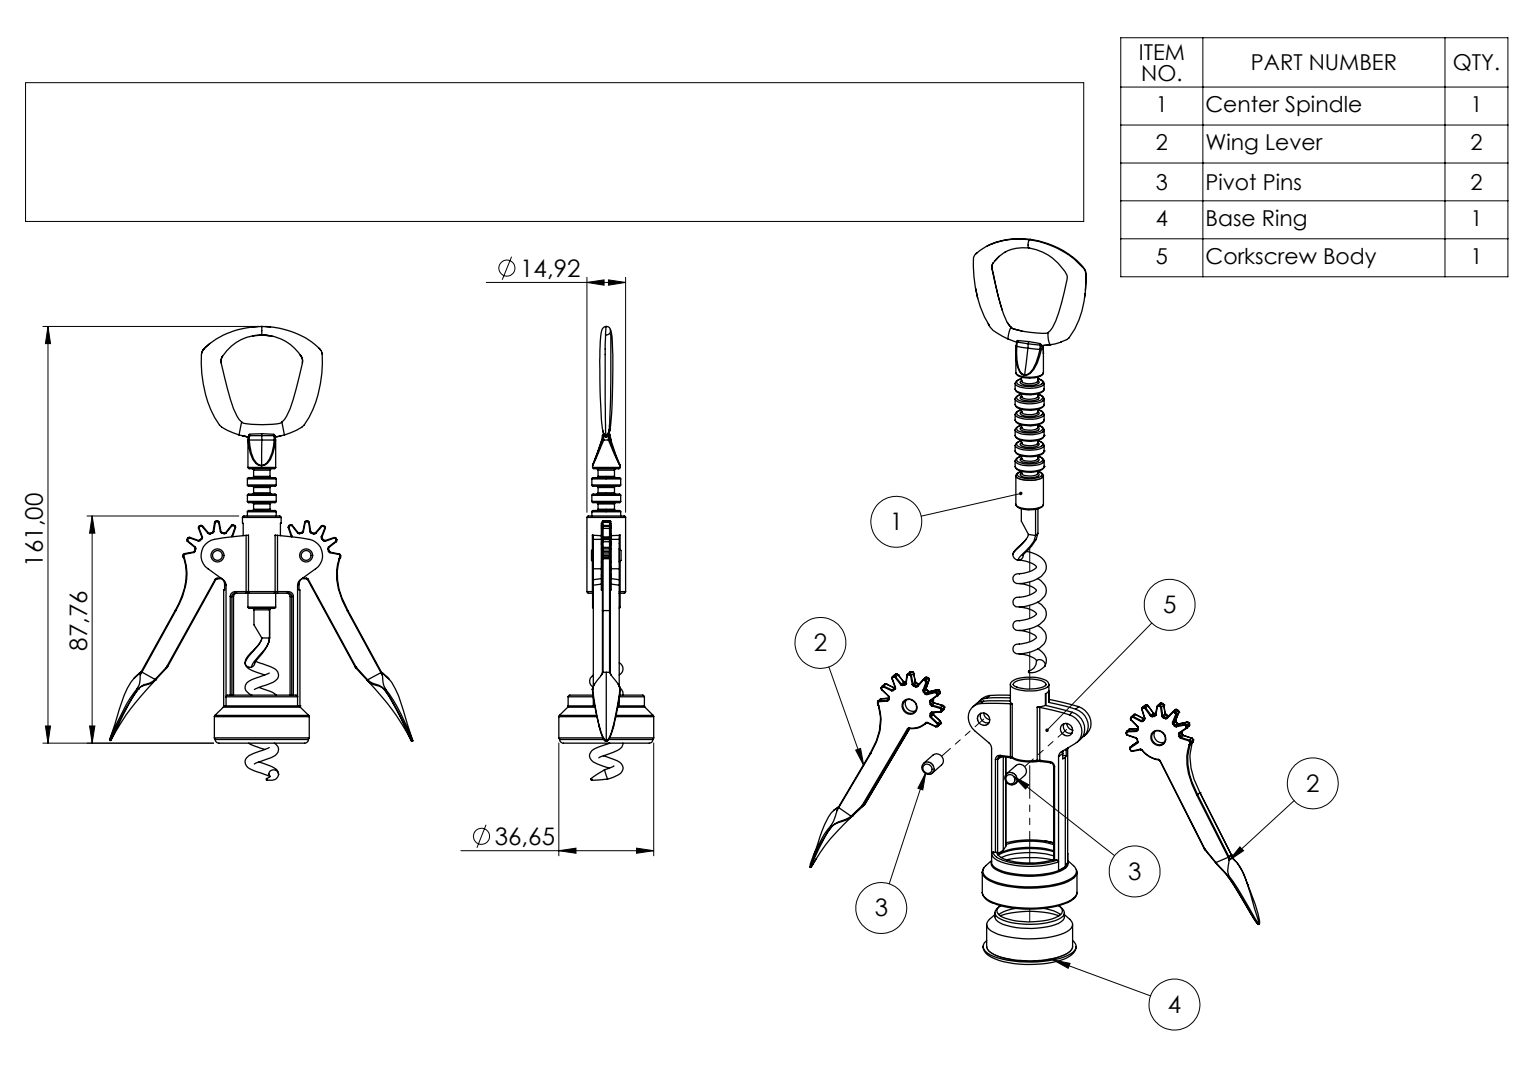
ISO-10303-21;
HEADER;
FILE_DESCRIPTION (('STEP AP214'),
    '1' );
FILE_NAME ('MAS-162',
    '2026-10-06T14:27:08',
    ( '' ),
    ( '' ),
    'SwSTEP 2.0',
    'SolidWorks 2020',
    '' );
FILE_SCHEMA (( 'AUTOMOTIVE_DESIGN' ));
ENDSEC;

DATA;
#1 = CARTESIAN_POINT ( 'NONE',  ( -2.902940568641317665, 107.8364052097302306, -4.470325690468441415 ) ) ;
#2 = CARTESIAN_POINT ( 'NONE',  ( 4.750191988411978095, 117.8920247151937843, 0.9103219801276267731 ) ) ;
#3 = CARTESIAN_POINT ( 'NONE',  ( 3.177488185987922709, -14.13217061847354472, 2.003775387181677026 ) ) ;
#4 = CARTESIAN_POINT ( 'NONE',  ( -6.473539731754439863, 155.4519854478747902, -1.179574399179393440 ) ) ;
#5 = CARTESIAN_POINT ( 'NONE',  ( -2.402553827781328089, 115.7029513687917017, -1.700315609833690900 ) ) ;
#6 = CARTESIAN_POINT ( 'NONE',  ( -3.112628982284441737, 108.2625926757257844, 4.181986096990026880 ) ) ;
#7 = CARTESIAN_POINT ( 'NONE',  ( -47.84919564605845466, 19.39087073395056393, 5.212699772323899694 ) ) ;
#8 = CARTESIAN_POINT ( 'NONE',  ( 0.1065646865914872399, 105.8844662015456777, -5.332932678536313809 ) ) ;
#9 = CARTESIAN_POINT ( 'NONE',  ( -8.921947645407078298, 154.9128698100208794, -1.713759150786742458 ) ) ;
#10 = CARTESIAN_POINT ( 'NONE',  ( 15.73471677570929117, 120.8416612192442159, 0.3144170877234249706 ) ) ;
#11 = CARTESIAN_POINT ( 'NONE',  ( -0.02969003158485089208, 157.1787724364823760, 1.485810588193620552 ) ) ;
#12 = CARTESIAN_POINT ( 'NONE',  ( -2.946616183681363133, 115.7030909710271231, 1.559688585259455307 ) ) ;
#13 = CARTESIAN_POINT ( 'NONE',  ( -5.328734912435950655, 121.3512789622145931, -0.03376412672994712899 ) ) ;
#14 = CARTESIAN_POINT ( 'NONE',  ( 3.102408547967445696, -0.5812848888516047863, -3.453265078539196509 ) ) ;
#16 = ORIENTED_EDGE ( 'NONE', *, *, #18091, .T. ) ;
#15 = CARTESIAN_POINT ( 'NONE',  ( 22.61937536341548238, 150.3405807453409579, 1.175526429919688587 ) ) ;
#17 = CARTESIAN_POINT ( 'NONE',  ( 16.60960244842765832, 9.026346327358513832, 0.000000000000000000 ) ) ;
#18 = CARTESIAN_POINT ( 'NONE',  ( 3.256234316240316229, -15.49904601598017706, 3.966862439782909533 ) ) ;
#19 = CARTESIAN_POINT ( 'NONE',  ( -19.06441997122223597, 145.0145856610025987, 1.755053680361626567 ) ) ;
#20 = CARTESIAN_POINT ( 'NONE',  ( 0.9007433063219677516, 2.300345052497278608, 0.3717552062572989091 ) ) ;
#21 = CARTESIAN_POINT ( 'NONE',  ( 0.003746264460233806812, 116.6481217037470373, -0.1874783927187336496 ) ) ;
#22 = CARTESIAN_POINT ( 'NONE',  ( -0.8226642509504364931, 2.890957568680109446, -0.5268263738024351328 ) ) ;
#23 = ORIENTED_EDGE ( 'NONE', *, *, #33925, .T. ) ;
#24 = CIRCLE ( 'NONE', #38114, 2.540000000000000480 ) ;
#25 = VERTEX_POINT ( 'NONE', #23978 ) ;
#26 = CARTESIAN_POINT ( 'NONE',  ( -45.52520984822221095, 18.49555408152312452, 0.5880787195337303652 ) ) ;
#27 = CARTESIAN_POINT ( 'NONE',  ( 4.040061035763102382, 117.6466181296975151, 0.9125624508345167030 ) ) ;
#28 = SHAPE_DEFINITION_REPRESENTATION ( #10271, #23419 ) ;
#29 = CARTESIAN_POINT ( 'NONE',  ( -1.787077659700294863, 156.4219299504922844, 0.8362026816545217178 ) ) ;
#30 = CARTESIAN_POINT ( 'NONE',  ( 3.821280252649200460, -11.76149679029331274, 0.6556923638117722053 ) ) ;
#31 = CARTESIAN_POINT ( 'NONE',  ( 12.33128838443251674, 153.5964916033214820, -1.587645809864455471 ) ) ;
#32 = CARTESIAN_POINT ( 'NONE',  ( -1.237267194679803950, 118.7146927282448132, -0.6928808259403732572 ) ) ;
#33 = CARTESIAN_POINT ( 'NONE',  ( -5.946078212987909062, 28.42590610009758123, 0.3016625663984517924 ) ) ;
#34 = CARTESIAN_POINT ( 'NONE',  ( 2.671714809844681238, -14.97371442308345380, 4.574436322856921144 ) ) ;
#35 = CARTESIAN_POINT ( 'NONE',  ( -2.623680569203113766, 34.84621527371866989, 1.140749429358363987 ) ) ;
#36 = CARTESIAN_POINT ( 'NONE',  ( 14.28939804845276740, 138.9852717218771261, -0.04639197223238045870 ) ) ;
#37 = ORIENTED_EDGE ( 'NONE', *, *, #18826, .T. ) ;
#38 = CYLINDRICAL_SURFACE ( 'NONE', #12263, 2.540000000000000480 ) ;
#39 = CARTESIAN_POINT ( 'NONE',  ( -8.428339483816529309, 74.57444062528223583, -1.523999999999996913 ) ) ;
#40 = CARTESIAN_POINT ( 'NONE',  ( -58.67410397513675235, -0.3138866149764163449, 0.3147537707000222507 ) ) ;
#41 = DIRECTION ( 'NONE',  ( -5.188838149069471174E-16, 1.699382548006136313E-16, 1.000000000000000000 ) ) ;
#42 = CARTESIAN_POINT ( 'NONE',  ( 15.65715779584547462, 120.8241032224722176, 0.2083191676592779373 ) ) ;
#43 = CARTESIAN_POINT ( 'NONE',  ( -6.321818188556177276, 120.0717973201777511, 0.2011600071967686865 ) ) ;
#44 = AXIS2_PLACEMENT_3D ( 'NONE', #23205, #7689, #33679 ) ;
#45 = CARTESIAN_POINT ( 'NONE',  ( -1.563156853714933625, 118.1287640443500351, 0.8777957133630984732 ) ) ;
#46 = CARTESIAN_POINT ( 'NONE',  ( -10.32169608105474090, 17.14500000000000313, 4.040823496909975887 ) ) ;
#47 = CARTESIAN_POINT ( 'NONE',  ( -0.1480340175562135652, 37.01381769933495747, -0.7398847138023396663 ) ) ;
#48 = CARTESIAN_POINT ( 'NONE',  ( 20.93418857319365500, 149.0309112320384486, 2.352213276463849034 ) ) ;
#49 = CARTESIAN_POINT ( 'NONE',  ( -2.673854242087471356, 19.56896771519852862, 3.769861741755948348 ) ) ;
#50 = CARTESIAN_POINT ( 'NONE',  ( -8.093932337251422027, 31.18171294578705854, -2.467657647566553258 ) ) ;
#51 = CARTESIAN_POINT ( 'NONE',  ( -2.171567613555696941, 116.7785827647842751, -0.5120155132742859605 ) ) ;
#52 = CARTESIAN_POINT ( 'NONE',  ( -2.327868625978157358, 124.9344662015457175, -0.04651635516647353863 ) ) ;
#53 = DIRECTION ( 'NONE',  ( -1.000000000000000000, -9.933992704233682996E-16, 0.000000000000000000 ) ) ;
#54 = CARTESIAN_POINT ( 'NONE',  ( 5.348924234570989533, 56.51499999999999346, 4.492130288940735738 ) ) ;
#55 = CARTESIAN_POINT ( 'NONE',  ( 3.195898997675873598, 105.1238757837674314, 4.272339236703191823 ) ) ;
#56 = CARTESIAN_POINT ( 'NONE',  ( 4.419457123578296454, 17.78516144714274105, -1.360477052881604143 ) ) ;
#57 = FACE_OUTER_BOUND ( 'NONE', #41013, .T. ) ;
#58 = DIRECTION ( 'NONE',  ( 0.6850534820564689875, -0.7284927773988614241, 8.537024980200769556E-16 ) ) ;
#59 = CARTESIAN_POINT ( 'NONE',  ( 2.461817612451524084, -15.00653475910608492, 4.866425834902347702 ) ) ;
#60 = CARTESIAN_POINT ( 'NONE',  ( 1.642663419667585778, 119.5945091202099348, -0.5769171603192788655 ) ) ;
#61 = CARTESIAN_POINT ( 'NONE',  ( -19.82178279981189206, 128.7876384977266468, 0.3398896782655025928 ) ) ;
#62 = ORIENTED_EDGE ( 'NONE', *, *, #26845, .T. ) ;
#63 = CARTESIAN_POINT ( 'NONE',  ( 5.241362157049035631, 88.73331249999999670, 5.310945289804168468 ) ) ;
#64 =( BOUNDED_SURFACE ( )  B_SPLINE_SURFACE ( 3, 2, ( 
 ( #13288, #26273, #2675 ),
 ( #25450, #22223, #6076 ),
 ( #23483, #20083, #948 ),
 ( #10925, #7750, #33106 ),
 ( #39712, #10513, #30310 ),
 ( #17523, #39496, #3725 ),
 ( #3937, #26910, #7329 ),
 ( #23697, #40345, #23915 ),
 ( #16896, #36508, #14119 ),
 ( #36717, #7538, #17320 ),
 ( #27333, #20287, #27119 ),
 ( #20500, #33315, #33527 ),
 ( #4144, #29899, #40134 ),
 ( #37135, #17106, #30523 ),
 ( #16684, #30108, #10716 ),
 ( #4360, #1154, #36307 ) ),
 .UNSPECIFIED., .F., .F., .T. ) 
 B_SPLINE_SURFACE_WITH_KNOTS ( ( 4, 2, 2, 2, 2, 2, 2, 4 ),
 ( 3, 3 ),
 ( -4.336808689942017736E-17, 0.002643305330645566355, 0.003964957995968371000, 0.005286610661291176079, 0.01057322132258239553, 0.01321652665322800395, 0.01585983198387361237, 0.02114644264516483269 ),
 ( 0.000000000000000000, 1.000000000000000000 ),
 .UNSPECIFIED. ) 
 GEOMETRIC_REPRESENTATION_ITEM ( )  RATIONAL_B_SPLINE_SURFACE ( (
 ( 1.000000000000000000, 0.7071067811865429098, 1.000000000000000000),
 ( 1.000000000000000000, 0.7071067811865429098, 1.000000000000000000),
 ( 1.000000000000000000, 0.7071067811865475727, 1.000000000000000000),
 ( 1.000000000000000000, 0.7071067811865475727, 1.000000000000000000),
 ( 1.000000000000000000, 0.7071067811865481278, 1.000000000000000000),
 ( 1.000000000000000000, 0.7071067811865481278, 1.000000000000000000),
 ( 1.000000000000000000, 0.7071067811865477948, 1.000000000000000000),
 ( 1.000000000000000000, 0.7071067811865477948, 1.000000000000000000),
 ( 1.000000000000000000, 0.7071067811865477948, 1.000000000000000000),
 ( 1.000000000000000000, 0.7071067811865477948, 1.000000000000000000),
 ( 1.000000000000000000, 0.7071067811865481278, 1.000000000000000000),
 ( 1.000000000000000000, 0.7071067811865481278, 1.000000000000000000),
 ( 1.000000000000000000, 0.7071067811865477948, 1.000000000000000000),
 ( 1.000000000000000000, 0.7071067811865477948, 1.000000000000000000),
 ( 1.000000000000000000, 0.7071067811865521247, 1.000000000000000000),
 ( 1.000000000000000000, 0.7071067811865521247, 1.000000000000000000) ) ) 
 REPRESENTATION_ITEM ( '' )  SURFACE ( )  );
#65 = ORIENTED_EDGE ( 'NONE', *, *, #10499, .F. ) ;
#66 = DIRECTION ( 'NONE',  ( -4.017660918040594346E-17, 1.000000000000000000, 2.376309959284834438E-19 ) ) ;
#67 = CARTESIAN_POINT ( 'NONE',  ( 6.083905389560601229, -14.65912421694762280, 0.09720023197589457153 ) ) ;
#68 = CARTESIAN_POINT ( 'NONE',  ( -10.16662615958544258, 120.4647147465577461, 1.171017801134732306 ) ) ;
#69 = AXIS2_PLACEMENT_3D ( 'NONE', #15499, #34901, #12099 ) ;
#70 = CARTESIAN_POINT ( 'NONE',  ( 8.033985789952966527, 118.2752802814886053, -0.7207832311977435680 ) ) ;
#71 = CARTESIAN_POINT ( 'NONE',  ( -0.9211762648548540433, 10.43857344512876040, -4.529598961101950927 ) ) ;
#72 = EDGE_CURVE ( 'NONE', #18166, #40365, #25788, .T. ) ;
#73 = CARTESIAN_POINT ( 'NONE',  ( -58.60980283399052837, -0.2526951616049680216, -0.4333512024961975739 ) ) ;
#74 = EDGE_LOOP ( 'NONE', ( #32492, #14883, #24594, #27507 ) ) ;
#75 = CARTESIAN_POINT ( 'NONE',  ( -58.36994270878630431, -0.2918297664318836304, -0.01629410684330124051 ) ) ;
#76 = CARTESIAN_POINT ( 'NONE',  ( 0.4140400251255503261, 124.3520329708341023, 0.07144784443200485891 ) ) ;
#77 = B_SPLINE_SURFACE_WITH_KNOTS ( 'NONE', 3, 3, ( 
 ( #14540, #40555, #8162, #21131, #40760, #17945, #30947, #37549, #8372, #19416, #22802, #3464, #6441, #12415, #15798, #3049, #32000, #22177, #35627, #273, #26019, #36045, #39028, #2839, #28807, #25407, #22595, #41823, #16428, #16007, #12820, #12617, #29006, #29432, #18996 ),
 ( #19831, #22385, #25604, #6860, #6034, #10045, #59, #38612, #9418, #35839, #19618, #35410, #16212, #32422, #23017, #6238, #6654, #19208, #2632, #3252, #41605, #32631, #32216, #38814, #42023, #29216, #13247, #25808, #13027, #9628, #26231, #38409, #9220, #39235, #9836 ),
 ( #15591, #28596, #35208, #26870, #26447, #30479, #39450, #29856, #33061, #694, #17063, #40089, #23872, #20042, #16640, #10253, #37096, #7710, #36677, #36467, #7498, #36892, #10469, #3892, #23226, #24086, #36258, #17280, #4316, #20458, #33274, #39878, #16856, #33487, #486 ),
 ( #4103, #13666, #30066, #7286, #903, #7914, #13877, #26658, #32846, #23438, #29648, #27081, #30269, #10884, #33696, #1110, #13459, #39665, #10675, #20248, #7079, #23657, #1323, #14078, #3676, #20672, #4520, #17482, #14280, #27290, #40305, #11098, #21294, #31110, #4939 ),
 ( #27704, #34322, #1947, #34530, #27909, #30900, #11305, #40711, #21497, #37923, #37498, #30685, #33904, #41344, #41127, #8113, #17898, #18520, #8746, #5150, #11507, #24493, #21088, #14906, #34732, #40916, #21708, #12146, #2370, #8323, #18105, #31311, #15115, #5356, #8537 ),
 ( #5563, #1740, #11722, #24709, #1535, #37714, #25138, #24925, #18309, #31526, #14490, #27503, #4733, #2155, #28118, #11933, #15328, #28335, #38142, #20879, #17685, #40511, #24290, #37295, #34112, #14699, #592, #26769, #26338, #33171, #13564, #29110, #29753, #3999, #6755 ),
 ( #10149, #19309, #22701, #16957, #32313, #6542, #9939, #19943, #29326, #23119, #22910, #25915, #35943, #35731, #35517, #19517, #6972, #20148, #10365, #3143, #38923, #29956, #26554, #23336, #13348, #16106, #32525, #19724, #9733, #42128, #382, #7189, #32962, #796, #3788 ),
 ( #32743, #170, #39344, #3356, #13140, #39560, #36155, #13772, #36373, #16323, #3576, #16537, #16748, #29548, #26132, #12924, #39133, #9522, #22489, #6338, #7389, #10573, #17998, #17787, #26978, #36783, #37396, #27595, #40197, #4423, #1220, #39988, #20775, #11404, #7813 ),
 ( #10779, #1425, #40604, #10992, #37191, #30371, #21185, #33374, #36573, #24391, #23760, #4627, #27183, #20350, #14382, #30996, #1636, #30586, #8213, #4206, #17170, #23552, #27391, #40402, #8013, #20984, #5043, #23974, #34005, #34214, #17582, #36992, #17381, #30169, #14179 ),
 ( #11196, #1837, #30786, #1010, #14590, #14801, #33799, #24182, #4835, #13974, #39779, #7599, #20561, #33590, #28228, #28442, #31422, #28011, #12468, #41234, #38459, #34415, #31637, #9277, #11830, #18415, #12037, #2687, #18203, #25028, #2264, #38031, #32055, #8851, #41020 ),
 ( #12253, #15228, #2893, #15439, #5675, #21815, #18633, #34841, #41448, #25246, #2047, #2478, #38249, #21389, #25463, #5248, #24817, #37812, #8637, #9066, #35060, #18843, #15012, #11613, #31204, #27804, #15644, #22032, #5881, #31847, #28649, #5455, #21600, #34628, #19050 ),
 ( #41660, #22235, #35263, #6087, #40812, #24597, #37604, #8431, #10316, #38669, #12878, #16274, #26288, #35685, #29494, #29278, #32271, #123, #29064, #41874, #42084, #13301, #26506, #16697, #25662, #3101, #39511, #20097, #32908, #6494, #335, #7140, #22651, #39296, #19472 ),
 ( #36109, #29702, #19678, #9476, #25867, #13087, #16062, #35469, #6710, #13517, #10103, #33121, #23075, #38873, #9685, #22440, #35899, #32479, #543, #26079, #39087, #3308, #9889, #23285, #22862, #36322, #32694, #15855, #3528, #16488, #28862, #19263, #12673, #6923, #19893 ),
 ( #6292, #3739, #33328, #961, #1591, #33962, #4373, #10730, #7553, #4158, #27134, #17742, #14132, #20937, #24347, #27557, #23711, #36730, #14335, #40357, #30538, #33541, #40147, #39727, #14548, #10526, #13930, #17120, #26925, #30324, #11152, #37147, #30121, #29912, #23496 ),
 ( #23929, #17333, #20513, #36523, #1168, #7969, #21140, #20729, #40564, #4791, #7342, #24139, #11362, #10940, #36944, #7765, #13725, #33753, #4579, #17537, #39938, #1377, #27345, #30742, #37354, #8172, #3950, #16911, #20301, #751, #26719, #18160, #24770, #5413, #9020 ),
 ( #2640, #38416, #21983, #11780, #5627, #25415, #40977, #18585, #37768, #9228, #8592, #18790, #18368, #21556, #5836, #17954, #28603, #12423, #31803, #27758, #1795, #25198, #31375, #34584, #40769, #2219, #15178, #21767, #14966, #28182, #12209, #24985, #34169, #35016, #41187 ),
 ( #31593, #11990, #2004, #24552, #37984, #34794, #15600, #8809, #14758, #4996, #30955, #38203, #21346, #31163, #41613, #11567, #2430, #15391, #28397, #34372, #41402, #37557, #8382, #5205, #27968, #3687, #42033, #12828, #32640, #16435, #6662, #9843, #67, #32429, #13037 ),
 ( #9635, #2847, #26027, #6246, #22810, #32007, #35418, #16648, #15807, #19215, #22603, #3473, #25816, #35848, #35635, #38622, #6449, #32225, #6042, #3057, #19625, #32855, #23025, #28815, #9425, #29655, #26456, #39245, #38824, #29442, #13467, #29013, #281, #19423, #39460 ),
 ( #36055, #39036, #41830, #16014, #3260, #22395, #12624, #13254, #19841, #26238, #22186, #10054, #16220, #29226, #25612, #6868, #495, #35216, #19004, #20465, #36474, #10683, #37103, #26666, #11104, #7506, #27510, #30074, #33282, #1541, #13675, #17692, #7717, #39674, #10477 ),
 ( #30486, #23446, #7294, #7921, #40311, #23664, #17071, #13885, #20255, #33494, #24093, #4324, #27296, #30691, #33911, #911, #26878, #20681, #4526, #36898, #40096, #30277, #17288, #1118, #14087, #23879, #10892, #4111, #39886, #27088, #3901, #20887, #16864, #36684, #33705 ),
 ( #17490, #1329, #14287, #14496, #4739, #10261, #23234, #36269, #7089, #20051, #29864, #33070, #704, #15553, #15125, #21933, #31536, #17905, #18531, #34962, #37723, #34742, #28128, #2380, #41354, #2166, #8120, #11515, #40924, #27711, #30909, #31322, #38152, #21718, #31750 ),
 ( #40720, #21094, #18320, #24500, #12156, #11730, #8547, #37505, #24719, #25148, #14706, #8965, #21506, #40518, #18112, #21301, #2593, #1747, #5785, #37933, #8331, #34330, #15340, #28345, #5158, #11944, #41138, #18740, #31117, #11310, #1954, #24297, #24935, #37303, #34118 ),
 ( #4945, #14914, #27918, #34539, #8756, #5573, #5365, #16167, #6400, #38774, #19370, #9585, #18, #29172, #2799, #15964, #22554, #22135, #26189, #35164, #25562, #28761, #38566, #12777, #35794, #19577, #15756, #12371, #5991, #32804, #3418, #32376, #32169, #3205, #32585 ),
 ( #18954, #19785, #31960, #12984, #25977, #38985, #28962, #35584, #12575, #9794, #38364, #41775, #22973, #9178, #9379, #41978, #22761, #6196, #6606, #25767, #22343, #16385, #35366, #25359, #19165, #29390, #39193, #230, #3005, #13206, #10001, #3635, #36003, #6815, #28555 ),
 ( #41563, #13413, #26831, #7457, #39838, #30229, #4270, #33021, #4062, #10635, #10210, #14240, #23180, #13623, #16814, #26614, #860, #23827, #7666, #3850, #443, #36215, #20836, #33654, #20414, #20207, #33443, #20624, #36429, #29816, #7036, #7874, #20003, #1068, #14036 ),
 ( #13833, #33234, #23614, #26402, #17233, #23397, #17021, #39621, #30020, #27040, #36635, #655, #1282, #40049, #27246, #10427, #10842, #40262, #7248, #36847, #4479, #17439, #30436, #11056, #24041, #37056, #33860, #16599, #29608, #39407, #24452, #1490, #41086, #21453, #24883 ),
 ( #8280, #18477, #30647, #41299, #25092, #31482, #40470, #14447, #37880, #31064, #21250, #11261, #18061, #37456, #34483, #27659, #34280, #8703, #37673, #8912, #5519, #11462, #5109, #14865, #18266, #11677, #14655, #37255, #1902, #5315, #21666, #27868, #27457, #17645, #38097 ),
 ( #31269, #2111, #12103, #34072, #34690, #21047, #21878, #15075, #24247, #2327, #40876, #24664, #4899, #8496, #15287, #28075, #11894, #28292, #4689, #8073, #17854, #30855, #1700, #40670, #12937, #29341, #32120, #38515, #15914, #2541, #22503, #41718, #35320, #2749, #6147 ) ),
 .UNSPECIFIED., .T., .F., .F.,
 ( 4, 2, 2, 2, 1, 2, 2, 2, 2, 2, 2, 1, 2, 2, 4 ),
 ( 4, 1, 1, 1, 1, 1, 1, 1, 1, 1, 1, 1, 1, 1, 1, 1, 1, 1, 1, 1, 1, 1, 1, 1, 1, 1, 1, 1, 1, 1, 1, 1, 4 ),
 ( 0.000000000000000000, 0.06249999999999900080, 0.1249999999999978906, 0.2499999999999956701, 0.2812499999999951150, 0.3749999999999934497, 0.4374999999999933387, 0.5000000000000000000, 0.5624999999999930056, 0.6249999999999928946, 0.7500000000000000000, 0.7812499999999951150, 0.8749999999999963363, 0.9374999999999982236, 1.000000000000000000 ),
 ( 0.000000000000000000, 0.02711375962671787321, 0.05385523109991235263, 0.08027126036152537614, 0.1064096946071439176, 0.1323192412471900226, 0.1580495177521483718, 0.1882118685537063907, 0.2182788543618764954, 0.2483346178351386324, 0.2784631806910429774, 0.3054937156393619513, 0.3327069032348308197, 0.3601597580799023035, 0.3879077415152338837, 0.4160045136367338525, 0.4445017332217630623, 0.4734489055539064517, 0.5028932750457014711, 0.5328797594123376724, 0.5634509204570880003, 0.5946469669818265080, 0.6265057848166851739, 0.6590629893014032792, 0.6923519956652609553, 0.7264041031822485728, 0.7612485893105871426, 0.7986318966073006065, 0.8369441774603861850, 0.8762126957585177900, 0.9164627945539034481, 0.9577180065289634392, 1.000000000000000000 ),
 .UNSPECIFIED. ) ;
#78 = CARTESIAN_POINT ( 'NONE',  ( -11.07124803888946296, 123.5714170083676748, 1.086458317614992231 ) ) ;
#79 = DIRECTION ( 'NONE',  ( -0.8745520943968315697, 0.4849315768086414624, -4.878299988686196152E-16 ) ) ;
#80 = CARTESIAN_POINT ( 'NONE',  ( 14.75721126660338811, 152.8628051715174365, -1.735400109512246880 ) ) ;
#81 = AXIS2_PLACEMENT_3D ( 'NONE', #23637, #14261, #11485 ) ;
#82 = CARTESIAN_POINT ( 'NONE',  ( -13.57054970571782704, 121.9345505566020194, -1.704910367088877221 ) ) ;
#83 = CARTESIAN_POINT ( 'NONE',  ( -6.072850655491211391, 78.87349744216251679, 4.348040511725084656 ) ) ;
#84 = ORIENTED_EDGE ( 'NONE', *, *, #36137, .T. ) ;
#85 = CARTESIAN_POINT ( 'NONE',  ( 4.532197386373657544, 118.1209942587670980, -0.4791226501333581411 ) ) ;
#86 = EDGE_CURVE ( 'NONE', #35923, #21980, #18976, .T. ) ;
#87 = CARTESIAN_POINT ( 'NONE',  ( 16.10174665100975488, 146.3760696504137684, -0.5323012926561621061 ) ) ;
#88 = ORIENTED_EDGE ( 'NONE', *, *, #11328, .F. ) ;
#89 = CARTESIAN_POINT ( 'NONE',  ( -17.42038752474488561, 148.2779598588913643, -2.227836471057101697 ) ) ;
#90 = CARTESIAN_POINT ( 'NONE',  ( 3.162278034637682200, -15.50568859125470134, 4.121945908858189789 ) ) ;
#91 = CARTESIAN_POINT ( 'NONE',  ( -3.552207995971087051, 105.1233060067599610, -3.981573230609858793 ) ) ;
#92 = CARTESIAN_POINT ( 'NONE',  ( 5.106395947886037234, 78.95054594174946772, -1.904999999999999583 ) ) ;
#93 = B_SPLINE_CURVE_WITH_KNOTS ( 'NONE', 3,
 ( #362, #13328, #570, #10344 ),
 .UNSPECIFIED., .F., .F.,
 ( 4, 4 ),
 ( 0.5010344700412979746, 1.000000000000000000 ),
 .UNSPECIFIED. ) ;
#94 = CARTESIAN_POINT ( 'NONE',  ( -4.827457070893626856, 117.7658616683732618, 0.8357213340295019943 ) ) ;
#95 = CARTESIAN_POINT ( 'NONE',  ( 7.266810130343707819, 121.1388872696715282, 1.097806971394259312 ) ) ;
#96 = CARTESIAN_POINT ( 'NONE',  ( -46.78089565521681692, 25.32111429335293451, 1.738356225806948929 ) ) ;
#97 = AXIS2_PLACEMENT_3D ( 'NONE', #15136, #24944, #28139 ) ;
#98 = CARTESIAN_POINT ( 'NONE',  ( 1.523114390242035210, -9.429190846093893796, -8.291516064885865234 ) ) ;
#99 = CARTESIAN_POINT ( 'NONE',  ( 4.578033532675482853, 121.1907927009877000, 0.1597499619731680698 ) ) ;
#100 = DIRECTION ( 'NONE',  ( 0.9998501190848640974, 0.01731298258485272981, 8.537024980200786319E-16 ) ) ;
#101 = ADVANCED_FACE ( 'NONE', ( #2270 ), #4717, .T. ) ;
#102 = EDGE_CURVE ( 'NONE', #36001, #40376, #18003, .T. ) ;
#104 = EDGE_LOOP ( 'NONE', ( #16225, #25822, #7892, #35896 ) ) ;
#103 = CARTESIAN_POINT ( 'NONE',  ( -49.81365592435692236, 14.60358288955459294, -2.185970286000775253 ) ) ;
#105 = CARTESIAN_POINT ( 'NONE',  ( -2.180832807216472435, 116.2031176879599599, -0.1302529176791268339 ) ) ;
#106 = CARTESIAN_POINT ( 'NONE',  ( 13.43845804798103316, 156.9141898299356512, 0.2685323735513602261 ) ) ;
#107 = VECTOR ( 'NONE', #35757, 1000.000000000000000 ) ;
#108 = FACE_OUTER_BOUND ( 'NONE', #15765, .T. ) ;
#109 = CARTESIAN_POINT ( 'NONE',  ( -48.74093372970734350, 18.21380663047653314, 5.157544856658800470 ) ) ;
#110 = CARTESIAN_POINT ( 'NONE',  ( 5.078986093043053707, 79.34146620154574236, 0.1014902294541244060 ) ) ;
#111 = ADVANCED_FACE ( 'NONE', ( #24605 ), #3343, .T. ) ;
#112 = CARTESIAN_POINT ( 'NONE',  ( -5.241362157049125337, 53.58606250000000415, 5.310945289804168468 ) ) ;
#113 = CYLINDRICAL_SURFACE ( 'NONE', #28014, 3.175000000000001155 ) ;
#114 = CARTESIAN_POINT ( 'NONE',  ( -53.63638764239521350, 11.23543775674477807, 3.971736527645110648 ) ) ;
#115 = CARTESIAN_POINT ( 'NONE',  ( -55.41603145274652320, 6.826612083464994818, 3.210495615568572436 ) ) ;
#116 = CARTESIAN_POINT ( 'NONE',  ( -23.30518390908433091, 149.0397177335360652, -0.1341373440727923194 ) ) ;
#117 = VERTEX_POINT ( 'NONE', #21192 ) ;
#118 = CARTESIAN_POINT ( 'NONE',  ( -51.90232906080404263, 16.51944673254565643, -2.845700375512763891 ) ) ;
#119 = CARTESIAN_POINT ( 'NONE',  ( 6.067968699521611775, 121.4399612899160843, 0.1149339127001053201 ) ) ;
#120 = VERTEX_POINT ( 'NONE', #22037 ) ;
#121 = CARTESIAN_POINT ( 'NONE',  ( 4.588798433226582318, 115.7029491485453150, -1.333296534009075662 ) ) ;
#122 = CARTESIAN_POINT ( 'NONE',  ( -5.931002064882670233, 121.5392726388429168, -0.1896088198168328631 ) ) ;
#123 = CARTESIAN_POINT ( 'NONE',  ( 4.852936394019410571, -14.31369683153947747, 4.236952399839363892 ) ) ;
#124 = CARTESIAN_POINT ( 'NONE',  ( -13.60293432442229999, 121.5020190402118203, 1.066732574264078748 ) ) ;
#125 = CARTESIAN_POINT ( 'NONE',  ( 5.974493989214552769, 78.88147413144905329, -5.016499999999998849 ) ) ;
#126 = CARTESIAN_POINT ( 'NONE',  ( 16.12231377365572982, 121.3783152868344075, 0.5570369914769761621 ) ) ;
#127 = CARTESIAN_POINT ( 'NONE',  ( 9.090272512956175888, 124.2201288364615266, 0.2714231486187235198 ) ) ;
#128 = CARTESIAN_POINT ( 'NONE',  ( -25.81615557310160369, 74.46796499802707103, -1.270000000000005791 ) ) ;
#129 = CARTESIAN_POINT ( 'NONE',  ( 0.7643174330569572072, 9.588751494893990923, -0.6113830025413525826 ) ) ;
#130 = CARTESIAN_POINT ( 'NONE',  ( -13.61156529719784558, 119.6358206793323404, -0.4233406866235920885 ) ) ;
#131 = DIRECTION ( 'NONE',  ( -5.206863593109713661E-17, 1.000000000000000000, -1.077750396879097183E-30 ) ) ;
#132 = DIRECTION ( 'NONE',  ( -0.1538570343431813203, -0.9876883405951371042, -0.02827993697916746443 ) ) ;
#133 = CARTESIAN_POINT ( 'NONE',  ( 8.672122787176258285, 118.2242029276344510, 0.9375713879804109530 ) ) ;
#134 = ORIENTED_EDGE ( 'NONE', *, *, #31655, .T. ) ;
#135 = CARTESIAN_POINT ( 'NONE',  ( -58.30601194912756569, -0.1568608524855368003, -0.3211567528579405972 ) ) ;
#136 = CARTESIAN_POINT ( 'NONE',  ( 14.23594795111937295, 121.8555783441548073, 1.592150851459066319 ) ) ;
#137 = CARTESIAN_POINT ( 'NONE',  ( 19.51325853822217127, 141.0981142166620259, -1.725252114789138203 ) ) ;
#138 = CARTESIAN_POINT ( 'NONE',  ( -0.1482875670852983607, 5.528424516503947395, -0.9633795868741713564 ) ) ;
#140 = AXIS2_PLACEMENT_3D ( 'NONE', #10662, #17050, #30466 ) ;
#139 = CARTESIAN_POINT ( 'NONE',  ( -0.4581589521676752153, 10.92003791307801208, 8.418874016967684781 ) ) ;
#141 = CARTESIAN_POINT ( 'NONE',  ( -12.23848595143957141, 156.6574886424908470, -1.779988832801368437 ) ) ;
#142 = CARTESIAN_POINT ( 'NONE',  ( 4.767275108742798473, 117.8956358391749717, -0.7413279629693602102 ) ) ;
#143 = CIRCLE ( 'NONE', #8295, 14.91798719394653716 ) ;
#144 = CARTESIAN_POINT ( 'NONE',  ( 9.138499898145592937, 117.7878261280527425, 0.1826089763859914672 ) ) ;
#145 = CARTESIAN_POINT ( 'NONE',  ( 4.403754988258198111, 120.5100497556178567, -0.5130326506441984513 ) ) ;
#146 = CARTESIAN_POINT ( 'NONE',  ( -11.83770080265077951, 152.0103986367769551, -0.1887002032782128802 ) ) ;
#147 = ORIENTED_EDGE ( 'NONE', *, *, #35169, .T. ) ;
#148 = CARTESIAN_POINT ( 'NONE',  ( -16.28588378367234313, 151.0861551944122141, -2.361334407247334788 ) ) ;
#149 = CARTESIAN_POINT ( 'NONE',  ( 5.396943489592968213, -15.24705710738187570, 2.503009974473451749 ) ) ;
#150 = CARTESIAN_POINT ( 'NONE',  ( 4.782580095254411745, 118.5931160184169073, 0.9661571381561826488 ) ) ;
#151 = CARTESIAN_POINT ( 'NONE',  ( -47.20791569504334717, 21.28685671521062517, -4.803936552638846891 ) ) ;
#152 = ORIENTED_EDGE ( 'NONE', *, *, #37062, .F. ) ;
#153 = CARTESIAN_POINT ( 'NONE',  ( 4.244755607818279763, 119.7015364213435333, 0.9259100998607280308 ) ) ;
#154 = DIRECTION ( 'NONE',  ( -0.9998004120163609398, 0.000000000000000000, -0.01997839162482749689 ) ) ;
#155 = ADVANCED_FACE ( 'NONE', ( #14807 ), #32569, .T. ) ;
#156 = CARTESIAN_POINT ( 'NONE',  ( -9.795036404550216957, 65.29837086945681790, -1.523999999999996025 ) ) ;
#157 = CARTESIAN_POINT ( 'NONE',  ( -5.575611629172074757, 123.3023672762779910, -0.03632235649590531690 ) ) ;
#158 = CARTESIAN_POINT ( 'NONE',  ( 7.184910528696541121, -14.53812136005497280, -4.413989948622978332 ) ) ;
#159 = CARTESIAN_POINT ( 'NONE',  ( 9.525206088249063896, 124.2661852542617709, 0.6183897905712308907 ) ) ;
#160 = CARTESIAN_POINT ( 'NONE',  ( 4.852593915752285270, 117.2114307359545649, -0.4396237197203589631 ) ) ;
#161 = CARTESIAN_POINT ( 'NONE',  ( -4.854186777038641765, 117.7557277303023966, -0.9091791526384296329 ) ) ;
#162 = DIRECTION ( 'NONE',  ( -1.000000000000000000, 1.365923996832131856E-16, 0.000000000000000000 ) ) ;
#163 = AXIS2_PLACEMENT_3D ( 'NONE', #1534, #902, #4938 ) ;
#164 = ADVANCED_FACE ( 'NONE', ( #34633 ), #16332, .T. ) ;
#165 = CARTESIAN_POINT ( 'NONE',  ( -15.96050253218469983, 121.0385544001969436, -0.3018840724360822847 ) ) ;
#166 = ORIENTED_EDGE ( 'NONE', *, *, #11201, .F. ) ;
#167 = CARTESIAN_POINT ( 'NONE',  ( 8.259156552716179434, 120.4369397177006960, -1.103309705185253842 ) ) ;
#168 = CARTESIAN_POINT ( 'NONE',  ( 23.29144772315967771, 149.3526176766912101, 0.4654185560736371352 ) ) ;
#169 = CARTESIAN_POINT ( 'NONE',  ( -9.418980095613695980, 123.9587481073520223, -0.7032982658115916053 ) ) ;
#170 = CARTESIAN_POINT ( 'NONE',  ( 2.004955844419833877, -15.09631637516548075, 5.820374350103214134 ) ) ;
#171 = CARTESIAN_POINT ( 'NONE',  ( -31.57591258916109922, 52.94298397416076085, 1.523999999999993582 ) ) ;
#172 = CARTESIAN_POINT ( 'NONE',  ( 20.51686376604209983, 129.1072961674477710, 0.4099757654675942331 ) ) ;
#173 = ORIENTED_EDGE ( 'NONE', *, *, #9182, .T. ) ;
#174 = CARTESIAN_POINT ( 'NONE',  ( -0.9211762648548540433, 10.43857344512876040, -4.529598961101950927 ) ) ;
#175 = CARTESIAN_POINT ( 'NONE',  ( -8.216926545874587262, 117.5004104479096583, -0.1641937475849288286 ) ) ;
#176 = CARTESIAN_POINT ( 'NONE',  ( -16.86202032626315628, 155.2029898760372646, -0.3369432954968343275 ) ) ;
#177 = DIRECTION ( 'NONE',  ( -0.8745520943968251304, 0.4849315768086532863, -5.424246918827961050E-16 ) ) ;
#178 = CARTESIAN_POINT ( 'NONE',  ( -6.120715547033301007, 121.1078720221529466, 0.4856508595550485530 ) ) ;
#179 = AXIS2_PLACEMENT_3D ( 'NONE', #33313, #30308, #33738 ) ;
#180 = CARTESIAN_POINT ( 'NONE',  ( 3.087053954869741101, 14.59627045569285286, -3.440871586639639990 ) ) ;
#181 = CARTESIAN_POINT ( 'NONE',  ( 21.46783008853678609, 136.6907720476960435, 1.692068800591147282 ) ) ;
#182 = CARTESIAN_POINT ( 'NONE',  ( -0.08519874065850288614, 108.5751225745497948, 4.263693374914160117 ) ) ;
#184 = CARTESIAN_POINT ( 'NONE',  ( 2.800559387825661606, 158.6924860557018064, -1.442603686385967032 ) ) ;
#183 = FACE_OUTER_BOUND ( 'NONE', #18213, .T. ) ;
#185 = CARTESIAN_POINT ( 'NONE',  ( 4.506137822554599381, 3.376467715207942533, 1.027655576270160243 ) ) ;
#186 = CARTESIAN_POINT ( 'NONE',  ( -14.63850908477053991, 156.0817623197167450, -1.342817726712510318 ) ) ;
#187 = ORIENTED_EDGE ( 'NONE', *, *, #10423, .F. ) ;
#188 = CARTESIAN_POINT ( 'NONE',  ( -15.46148294186166439, 147.8441550597069352, 0.1409636975754419985 ) ) ;
#189 = CARTESIAN_POINT ( 'NONE',  ( 3.228727248129140026, -15.23899909574484646, 5.612614099740361517 ) ) ;
#190 = CARTESIAN_POINT ( 'NONE',  ( -6.615214180512292604E-14, 94.32746620154571815, -2.829521569843129660E-18 ) ) ;
#191 = CARTESIAN_POINT ( 'NONE',  ( 2.969447359227861405, -13.80100253337253946, 0.9847735008004718793 ) ) ;
#192 = ORIENTED_EDGE ( 'NONE', *, *, #36999, .T. ) ;
#193 = CARTESIAN_POINT ( 'NONE',  ( 2.329084838958874748, 118.9063233352275972, 0.7992829875212342783 ) ) ;
#194 = DIRECTION ( 'NONE',  ( 1.000000000000000000, 0.000000000000000000, 0.000000000000000000 ) ) ;
#195 = DIRECTION ( 'NONE',  ( -1.000000000000000000, 9.627370216492861475E-17, 0.000000000000000000 ) ) ;
#196 = CARTESIAN_POINT ( 'NONE',  ( -22.74464968533201414, 149.4207734315791072, 0.6238039466385616461 ) ) ;
#197 = CARTESIAN_POINT ( 'NONE',  ( 23.16228472148464235, 149.2833505036244048, -0.1324855245534189985 ) ) ;
#198 = EDGE_CURVE ( 'NONE', #31926, #33162, #2052, .T. ) ;
#199 = CARTESIAN_POINT ( 'NONE',  ( -5.354045385512117505, 57.14999999999997726, -5.213862164334880589 ) ) ;
#200 = CARTESIAN_POINT ( 'NONE',  ( -46.74948388161530488, 25.87427737361800339, 1.400905913749466380 ) ) ;
#201 = CARTESIAN_POINT ( 'NONE',  ( -47.14788814370446346, 23.76379789425250166, 2.690610990139707059 ) ) ;
#203 = ADVANCED_FACE ( 'NONE', ( #18208 ), #14201, .F. ) ;
#202 = CARTESIAN_POINT ( 'NONE',  ( 2.109804961112711652, -15.28918944155240034, 5.362628413980365494 ) ) ;
#204 = CARTESIAN_POINT ( 'NONE',  ( -53.68435271313694557, 11.12367579685427721, 3.945100831076007619 ) ) ;
#205 = DIRECTION ( 'NONE',  ( -5.206863593109713661E-17, 1.000000000000000000, -1.077750396879097183E-30 ) ) ;
#206 = CARTESIAN_POINT ( 'NONE',  ( -4.535815920756029129, 118.0878757016629521, 0.6031417657034798818 ) ) ;
#207 = PLANE ( 'NONE',  #933 ) ;
#208 = ORIENTED_EDGE ( 'NONE', *, *, #17060, .T. ) ;
#209 = ORIENTED_EDGE ( 'NONE', *, *, #20675, .T. ) ;
#210 = CARTESIAN_POINT ( 'NONE',  ( -0.3650308193387738487, 118.7629491485454025, -1.279690690685891807 ) ) ;
#211 = CARTESIAN_POINT ( 'NONE',  ( 6.034264073414651541, 119.2911550975486676, -1.026770045858946823 ) ) ;
#212 = CARTESIAN_POINT ( 'NONE',  ( -3.903247448917784190, 109.8183322527596602, -3.677532532511333052 ) ) ;
#213 = CARTESIAN_POINT ( 'NONE',  ( 4.607970095737445426, 117.9806936862427449, 0.9111728063042895398 ) ) ;
#214 = CARTESIAN_POINT ( 'NONE',  ( -46.68395179480138069, 26.03198510454123848, -1.397000000000007569 ) ) ;
#215 = CARTESIAN_POINT ( 'NONE',  ( -10.17133788503933900, 124.0743415861677903, -1.120692231141950934 ) ) ;
#216 = AXIS2_PLACEMENT_3D ( 'NONE', #23878, #24296, #37504 ) ;
#217 = CARTESIAN_POINT ( 'NONE',  ( -2.225528185412928295, 115.7029491485453576, -1.707866438218498040 ) ) ;
#218 = CARTESIAN_POINT ( 'NONE',  ( -2.874359970738451509, 107.8415691140158543, 4.365465615796717103 ) ) ;
#219 = CARTESIAN_POINT ( 'NONE',  ( -4.791894246051028539, 117.8359990171110780, -0.9363294005345770277 ) ) ;
#220 = CARTESIAN_POINT ( 'NONE',  ( 5.257173101725930664, 116.1034411669277375, -1.028648520082846352 ) ) ;
#221 = CARTESIAN_POINT ( 'NONE',  ( -10.56433624517455705, 123.7931190674884050, -1.348085882050163331 ) ) ;
#222 = CARTESIAN_POINT ( 'NONE',  ( -13.51785991797445341, 17.08228783296376818, -5.016500000000000625 ) ) ;
#223 = CARTESIAN_POINT ( 'NONE',  ( -0.01596947694136538129, 156.4635559983122448, 0.7991779281049289363 ) ) ;
#224 = CARTESIAN_POINT ( 'NONE',  ( -2.827941042956166662, 115.7033332087140138, 1.571145331901102171 ) ) ;
#225 = CARTESIAN_POINT ( 'NONE',  ( -15.78496548096122076, 146.2362003282640615, -0.2482417383768280028 ) ) ;
#226 = CARTESIAN_POINT ( 'NONE',  ( 1.360477052538118681, -3.804838552850991817, 4.419457122809256511 ) ) ;
#228 = ORIENTED_EDGE ( 'NONE', *, *, #36703, .T. ) ;
#227 = CARTESIAN_POINT ( 'NONE',  ( 23.03149411880787767, 148.7220611141358404, 1.316198435982438797 ) ) ;
#229 = DIRECTION ( 'NONE',  ( -0.8745520943968235761, 0.4849315768086558398, -5.691349986800547879E-16 ) ) ;
#230 = CARTESIAN_POINT ( 'NONE',  ( 3.491209331645790837, -14.97137451562302601, 1.144833103274278230 ) ) ;
#231 = CARTESIAN_POINT ( 'NONE',  ( -8.255438862926547827, 156.5149677146980309, 1.736665298733278906 ) ) ;
#232 = CARTESIAN_POINT ( 'NONE',  ( 0.5639076275445228381, 13.94848098472073161, -0.7944722417661187475 ) ) ;
#233 = CARTESIAN_POINT ( 'NONE',  ( -21.68922513019262510, 151.4054434770023363, -1.149106048033103011 ) ) ;
#234 = CIRCLE ( 'NONE', #18562, 0.6350000000000036726 ) ;
#235 = CARTESIAN_POINT ( 'NONE',  ( 0.6857505489063979720, -9.425274534614802135, -0.6942005185601292094 ) ) ;
#236 = ORIENTED_EDGE ( 'NONE', *, *, #38437, .F. ) ;
#237 = CARTESIAN_POINT ( 'NONE',  ( -43.02406770836220318, 21.15087974136648086, 0.6363192884523977133 ) ) ;
#238 = CARTESIAN_POINT ( 'NONE',  ( 7.588497335288401757, 124.2943531750336490, 0.1606663149101728583 ) ) ;
#239 = SHAPE_DEFINITION_REPRESENTATION ( #33079, #30767 ) ;
#240 = CARTESIAN_POINT ( 'NONE',  ( -11.01086703061210414, 126.1652090859982707, 0.5547642914263289926 ) ) ;
#241 = CARTESIAN_POINT ( 'NONE',  ( 2.933303798676236696, -14.66982100897798524, 5.370674165220748364 ) ) ;
#242 = CARTESIAN_POINT ( 'NONE',  ( 4.329049305160035388, 120.0471566133196291, -0.6733469523851639549 ) ) ;
#243 = CARTESIAN_POINT ( 'NONE',  ( -16.05419991788312473, 128.5601350900737998, -2.191829208737125612 ) ) ;
#244 = CARTESIAN_POINT ( 'NONE',  ( -11.66725022231030628, 17.14499999999999957, -5.016499999999999737 ) ) ;
#245 = CARTESIAN_POINT ( 'NONE',  ( 2.663950356258127705, -13.19741034273377878, 0.1528337951401303463 ) ) ;
#246 = CARTESIAN_POINT ( 'NONE',  ( -5.943370056925232348, 31.21256582444267380, 0.1301312493255015745 ) ) ;
#247 = CARTESIAN_POINT ( 'NONE',  ( 11.97065782032992587, 130.4318746828361100, 0.03484989721007641927 ) ) ;
#248 = ORIENTED_EDGE ( 'NONE', *, *, #30050, .T. ) ;
#249 = CARTESIAN_POINT ( 'NONE',  ( -4.780654621982846741, 111.8765634536314906, 2.439804913899639605 ) ) ;
#250 = DIRECTION ( 'NONE',  ( -5.188838149069471174E-16, 1.699382548006136313E-16, 1.000000000000000000 ) ) ;
#251 = CIRCLE ( 'NONE', #36280, 5.588000000000006295 ) ;
#252 = CARTESIAN_POINT ( 'NONE',  ( -6.135835944515187101, 77.40800365160224317, 1.270000000000003793 ) ) ;
#253 = CARTESIAN_POINT ( 'NONE',  ( -58.64207371057519680, -0.3086014758121452539, 0.3447476069572601998 ) ) ;
#254 = AXIS2_PLACEMENT_3D ( 'NONE', #10805, #1032, #33194 ) ;
#255 = CARTESIAN_POINT ( 'NONE',  ( 3.297133786507668418, 159.4684106755469202, 0.01890815954692008985 ) ) ;
#256 = CARTESIAN_POINT ( 'NONE',  ( -6.540839804427584170, 120.6338824379019172, 0.1347920106280767472 ) ) ;
#257 = CIRCLE ( 'NONE', #34949, 0.6350000000000006750 ) ;
#258 = CARTESIAN_POINT ( 'NONE',  ( -1.044188858242598439, 115.6909491485452435, 1.710615210114453166 ) ) ;
#259 = CARTESIAN_POINT ( 'NONE',  ( 4.529186081025091681, -11.15152372915077095, -0.9203776863585164669 ) ) ;
#260 = CARTESIAN_POINT ( 'NONE',  ( -2.340953058884871485, 34.37024003021338103, 0.7097582906893736832 ) ) ;
#261 = EDGE_CURVE ( 'NONE', #2461, #25488, #15017, .T. ) ;
#262 = CARTESIAN_POINT ( 'NONE',  ( 14.62144676724393300, 123.3142630313093377, 1.799443978378394648 ) ) ;
#263 = CARTESIAN_POINT ( 'NONE',  ( -2.394960105286914942, 16.54535949628658997, -3.951836011466995036 ) ) ;
#264 = CARTESIAN_POINT ( 'NONE',  ( -4.020893062959163267, -8.947226795047690473, 7.425401991387179379 ) ) ;
#265 = CARTESIAN_POINT ( 'NONE',  ( -5.483673445576510375, 117.2147343480241091, -0.8092650553969497063 ) ) ;
#266 = CARTESIAN_POINT ( 'NONE',  ( -0.8420595575569044255, 109.5507526474568607, -3.867914470699519658 ) ) ;
#267 = DIRECTION ( 'NONE',  ( -5.188838149069471174E-16, 1.699382548006136313E-16, 1.000000000000000000 ) ) ;
#268 = CARTESIAN_POINT ( 'NONE',  ( -9.638062024671791406, 56.51499999999998636, 3.341163682266966022E-16 ) ) ;
#269 = CARTESIAN_POINT ( 'NONE',  ( -2.880622083164609215, 104.6144662015456959, 4.502939351893831876 ) ) ;
#270 = CARTESIAN_POINT ( 'NONE',  ( 3.979181138743986601, 26.09377549647152961, 2.406711837290479661 ) ) ;
#271 = CARTESIAN_POINT ( 'NONE',  ( 2.081416901521091933, -15.50639809317535089, 5.943648939154567934 ) ) ;
#272 = CARTESIAN_POINT ( 'NONE',  ( -14.60500000000000220, 71.11999999999999034, -5.080000000000000959 ) ) ;
#273 = CARTESIAN_POINT ( 'NONE',  ( 3.216700609619024931, -14.42020774479446921, 2.887214088933996337 ) ) ;
#274 = CARTESIAN_POINT ( 'NONE',  ( 2.327868625978029016, 124.9344662015457175, 0.04651635516647314311 ) ) ;
#275 = CARTESIAN_POINT ( 'NONE',  ( -14.42641459765142820, 120.3907653763288579, 0.3011401359519875198 ) ) ;
#276 = VERTEX_POINT ( 'NONE', #11409 ) ;
#277 = DIRECTION ( 'NONE',  ( 0.8572391118119510045, 0.5149185422762100339, 3.573031421855330583E-16 ) ) ;
#278 = ORIENTED_EDGE ( 'NONE', *, *, #32111, .F. ) ;
#279 = CARTESIAN_POINT ( 'NONE',  ( -5.174735437441460917, 115.7029491485453576, 1.071059064073374589 ) ) ;
#280 = AXIS2_PLACEMENT_3D ( 'NONE', #23824, #4267, #36844 ) ;
#281 = CARTESIAN_POINT ( 'NONE',  ( 5.898825546834660649, -14.84738759216856785, 0.02597052417917125600 ) ) ;
#282 = CARTESIAN_POINT ( 'NONE',  ( -13.14453721617490523, 122.4605402651681487, 1.292199650740640138 ) ) ;
#283 = CARTESIAN_POINT ( 'NONE',  ( 9.329873057606279829, 118.8811571165754941, -0.8296725728930305355 ) ) ;
#284 = CARTESIAN_POINT ( 'NONE',  ( -4.627450822138572839, 2.892058097378844117, -0.1328416527703782657 ) ) ;
#285 = CARTESIAN_POINT ( 'NONE',  ( -58.63219855361986532, -0.2943491849813937300, -0.3701125355236437042 ) ) ;
#286 = EDGE_LOOP ( 'NONE', ( #24202, #14041, #34463, #28082 ) ) ;
#287 = CARTESIAN_POINT ( 'NONE',  ( -17.76856900107737403, 61.81127730225986738, 1.269999999999999352 ) ) ;
#288 = CARTESIAN_POINT ( 'NONE',  ( 0.2094794444022589075, 111.5577547982948801, 3.149697633913104866 ) ) ;
#289 = CARTESIAN_POINT ( 'NONE',  ( -4.765692302950382597, 117.6625622553268471, 0.9423543906840938789 ) ) ;
#290 = CARTESIAN_POINT ( 'NONE',  ( -17.01014995307831867, 147.0740084267719396, 1.247012517048586844 ) ) ;
#291 = CARTESIAN_POINT ( 'NONE',  ( 5.111850311340921493, 116.9863990472329931, 0.4425446553583142206 ) ) ;
#292 = CARTESIAN_POINT ( 'NONE',  ( 5.080524353911745727, 119.7208665877771665, -0.8394179162009564044 ) ) ;
#293 = CARTESIAN_POINT ( 'NONE',  ( 0.02969037535068572500, 158.7301711276701894, -1.485827791648137053 ) ) ;
#294 = CARTESIAN_POINT ( 'NONE',  ( -57.83637253161431602, 2.237724655402451024, -1.757929103219309397 ) ) ;
#295 = CIRCLE ( 'NONE', #24741, 0.7620000000000015650 ) ;
#296 = VERTEX_POINT ( 'NONE', #28017 ) ;
#297 = CARTESIAN_POINT ( 'NONE',  ( 4.483427315476480324, 118.1297255826064401, -0.5360345877169139239 ) ) ;
#298 = CARTESIAN_POINT ( 'NONE',  ( 9.732488649496215061, 124.0009531390599591, -0.4956537337270181531 ) ) ;
#299 = ORIENTED_EDGE ( 'NONE', *, *, #22158, .F. ) ;
#300 = CARTESIAN_POINT ( 'NONE',  ( -1.368713796474945177, 119.6596719632383383, -0.6021288208518275065 ) ) ;
#301 = CARTESIAN_POINT ( 'NONE',  ( 3.819321967970790599, -15.20641387874817418, 0.06971680219106241028 ) ) ;
#302 = EDGE_CURVE ( 'NONE', #37691, #28646, #26431, .T. ) ;
#303 = AXIS2_PLACEMENT_3D ( 'NONE', #10017, #38788, #25577 ) ;
#304 = CARTESIAN_POINT ( 'NONE',  ( -4.782196433634765320, 105.1214876792004560, -2.388545300328469345 ) ) ;
#305 = CARTESIAN_POINT ( 'NONE',  ( -16.04309792416813707, 12.96416000000000146, 5.016499999999999737 ) ) ;
#306 = ADVANCED_FACE ( 'NONE', ( #31428 ), #28233, .F. ) ;
#307 = CARTESIAN_POINT ( 'NONE',  ( -4.980589814694351247, 117.5315369307823801, 0.7737963060445882668 ) ) ;
#308 = CARTESIAN_POINT ( 'NONE',  ( 17.04317705290379692, 148.4623951536435698, 2.145728921095965358 ) ) ;
#309 = CARTESIAN_POINT ( 'NONE',  ( -2.803395127021860223, 31.26063551530791074, 0.8708390753670083306 ) ) ;
#310 = AXIS2_PLACEMENT_3D ( 'NONE', #29921, #20311, #10947 ) ;
#311 = EDGE_CURVE ( 'NONE', #34241, #32706, #19639, .T. ) ;
#312 = CARTESIAN_POINT ( 'NONE',  ( 8.369700380136936957, -11.69135346447765933, 0.7700151973242596037 ) ) ;
#313 = CARTESIAN_POINT ( 'NONE',  ( 9.115443861533906400, 124.0847320388339625, 0.2671161660598814769 ) ) ;
#314 = DIRECTION ( 'NONE',  ( -0.8745520943968235761, 0.4849315768086558398, -5.691349986800547879E-16 ) ) ;
#315 =( BOUNDED_SURFACE ( )  B_SPLINE_SURFACE ( 3, 1, ( 
 ( #22075, #40860 ),
 ( #8688, #31254 ),
 ( #11879, #24648 ),
 ( #15059, #5300 ),
 ( #28059, #24868 ),
 ( #9112, #41495 ),
 ( #34264, #31896 ),
 ( #12300, #21650 ),
 ( #38293, #41069 ),
 ( #37864, #18888 ),
 ( #31468, #35102 ),
 ( #2311, #28277 ),
 ( #8896, #41282 ),
 ( #5720, #18676 ),
 ( #31683, #2733 ),
 ( #28487, #15688 ) ),
 .UNSPECIFIED., .T., .F., .T. ) 
 B_SPLINE_SURFACE_WITH_KNOTS ( ( 4, 1, 1, 1, 1, 1, 2, 1, 1, 1, 1, 1, 4 ),
 ( 2, 2 ),
 ( 0.000000000000000000, 0.02374999999999993783, 0.1365624999999999478, 0.2493749999999999578, 0.3621874999999999956, 0.4749999999999999778, 0.5000000000000000000, 0.5250000000000000222, 0.6378125000000000044, 0.7506249999999999867, 0.8634374999999999689, 0.9762499999999999512, 1.000000000000000000 ),
 ( 0.000000000000000000, 1.000000000000000000 ),
 .UNSPECIFIED. ) 
 GEOMETRIC_REPRESENTATION_ITEM ( )  RATIONAL_B_SPLINE_SURFACE ( (
 ( 1.000000000000000000, 1.000000000000000000),
 ( 1.000000000000000222, 1.000000000000000000),
 ( 0.8208939328743548591, 1.000000000000000000),
 ( 0.5876145654044752087, 1.000000000000000000),
 ( 0.4813067448364888867, 1.000000000000000000),
 ( 0.5852845309810671415, 1.000000000000000000),
 ( 0.8180077452667815496, 1.000000000000000000),
 ( 0.9982788296041308351, 1.000000000000000000),
 ( 0.9982788296041308351, 1.000000000000000000),
 ( 0.8180077452667815496, 1.000000000000000000),
 ( 0.5852845309810672525, 1.000000000000000000),
 ( 0.4813067448364889422, 1.000000000000000000),
 ( 0.5876145654044749866, 1.000000000000000000),
 ( 0.8208939328743545261, 1.000000000000000000),
 ( 1.000000000000000000, 1.000000000000000000),
 ( 1.000000000000000000, 1.000000000000000000) ) ) 
 REPRESENTATION_ITEM ( '' )  SURFACE ( )  );
#316 = CARTESIAN_POINT ( 'NONE',  ( -46.49274047292066570, 18.53875678104565594, -2.063467562158697088 ) ) ;
#317 = CARTESIAN_POINT ( 'NONE',  ( 5.564716835327648603, 116.6996553459067485, 0.05384121919325710742 ) ) ;
#318 = DIRECTION ( 'NONE',  ( -0.8572391118119438991, -0.5149185422762221354, -3.573031421855274870E-16 ) ) ;
#319 = CARTESIAN_POINT ( 'NONE',  ( -46.79329363240532302, 25.76054971305726937, -1.464668473915645253 ) ) ;
#320 = DIRECTION ( 'NONE',  ( -5.206863593109713661E-17, 1.000000000000000000, -1.077750396879097183E-30 ) ) ;
#321 = CARTESIAN_POINT ( 'NONE',  ( -4.855072294470598848, 115.7029491485453718, 1.279409886141107178 ) ) ;
#322 = CARTESIAN_POINT ( 'NONE',  ( -5.305748947172281405, 65.30181249999996851, 5.247078976224250013 ) ) ;
#323 = CARTESIAN_POINT ( 'NONE',  ( -14.73200000000000109, 57.78499999999998948, 0.000000000000000000 ) ) ;
#324 = CARTESIAN_POINT ( 'NONE',  ( -25.56614996202194590, 73.65611136973726047, -1.524000000000005572 ) ) ;
#325 = CARTESIAN_POINT ( 'NONE',  ( -57.34105142390577470, 4.241571993195747403, 0.1395372036359874557 ) ) ;
#326 = CARTESIAN_POINT ( 'NONE',  ( -57.57967628038989005, 1.451576601202181349, 1.494865757154131725 ) ) ;
#327 = EDGE_CURVE ( 'NONE', #29906, #24559, #18939, .T. ) ;
#328 = CARTESIAN_POINT ( 'NONE',  ( -6.912985389844515716, 117.2044255678715814, 0.04371034868568312443 ) ) ;
#329 = VERTEX_POINT ( 'NONE', #35268 ) ;
#330 = CARTESIAN_POINT ( 'NONE',  ( -50.78366386294959511, 19.84645248585079003, -1.614153572948420212 ) ) ;
#331 = CARTESIAN_POINT ( 'NONE',  ( -6.058547263772821267, 121.4334988323120683, -0.1247128170359407956 ) ) ;
#332 = VERTEX_POINT ( 'NONE', #9690 ) ;
#333 = CARTESIAN_POINT ( 'NONE',  ( -5.332922648341591909, 115.7029491485453718, -0.1072025963776009894 ) ) ;
#334 = CARTESIAN_POINT ( 'NONE',  ( -15.38115207166226561, 147.8278496344100859, -0.4352178850651138853 ) ) ;
#335 = CARTESIAN_POINT ( 'NONE',  ( 5.987854329437395151, -12.83555092537783082, 1.339350064115379935 ) ) ;
#336 = CARTESIAN_POINT ( 'NONE',  ( -20.77691070360842929, 149.9184980045912425, 1.462349339025473371 ) ) ;
#337 = CARTESIAN_POINT ( 'NONE',  ( 1.325333094648095011, 19.28447512809159292, -4.440015753949128730 ) ) ;
#338 = CARTESIAN_POINT ( 'NONE',  ( 23.02690842483876565, 149.8694456586574972, 0.9127416204503947528 ) ) ;
#339 = CARTESIAN_POINT ( 'NONE',  ( 2.116771290498892899, -15.66388792789737217, 5.610892275307695520 ) ) ;
#340 = CARTESIAN_POINT ( 'NONE',  ( 4.771882511409050842, 118.5266822147775940, -0.8399436299859415200 ) ) ;
#341 = CARTESIAN_POINT ( 'NONE',  ( 0.8400667230086624748, -1.857414735510459547, 0.5005776846920441114 ) ) ;
#342 = CARTESIAN_POINT ( 'NONE',  ( 0.001640166039734963777, 159.6041700698465036, -0.08208061555506483697 ) ) ;
#343 = CARTESIAN_POINT ( 'NONE',  ( -0.1058213901579529159, 105.9761915687834914, 5.295735085524055030 ) ) ;
#344 = DIRECTION ( 'NONE',  ( -1.000000000000000000, -6.353134868986659519E-16, 0.000000000000000000 ) ) ;
#345 = ORIENTED_EDGE ( 'NONE', *, *, #41321, .T. ) ;
#346 = CARTESIAN_POINT ( 'NONE',  ( -5.552382799689717707, 117.0635824090028194, 0.4511715980537314707 ) ) ;
#347 = ORIENTED_EDGE ( 'NONE', *, *, #18115, .F. ) ;
#348 = CARTESIAN_POINT ( 'NONE',  ( -7.569905091580626078, 156.0351187175861867, 1.610277000873165276 ) ) ;
#349 = FACE_OUTER_BOUND ( 'NONE', #29106, .T. ) ;
#350 = CARTESIAN_POINT ( 'NONE',  ( 16.25125256408137986, 125.3309463260932830, 1.843050201054562187 ) ) ;
#351 = CARTESIAN_POINT ( 'NONE',  ( 1.119065284002195959, 158.2739225783580537, -1.587016747512054016 ) ) ;
#352 = CARTESIAN_POINT ( 'NONE',  ( -0.6988831915142799112, -0.7227331674307564402, 0.6786060147580050828 ) ) ;
#353 = CARTESIAN_POINT ( 'NONE',  ( -20.44519586420853585, 150.9797539340098069, -2.100688152434084799 ) ) ;
#354 = CARTESIAN_POINT ( 'NONE',  ( 4.677671540821375373, 117.9838357377442293, -0.6916929324824377945 ) ) ;
#355 = DIRECTION ( 'NONE',  ( -0.8745520943968243532, 0.4849315768086547296, -6.829619984160642269E-16 ) ) ;
#356 = EDGE_CURVE ( 'NONE', #12580, #5531, #25752, .T. ) ;
#357 = CARTESIAN_POINT ( 'NONE',  ( 16.46834812293193195, 148.4304801786341272, -1.248264531716813286 ) ) ;
#358 = CARTESIAN_POINT ( 'NONE',  ( -0.0005468344959711694646, 156.3034662015456604, 0.02736583427618486872 ) ) ;
#359 = VERTEX_POINT ( 'NONE', #29070 ) ;
#360 = CARTESIAN_POINT ( 'NONE',  ( -3.340139884075267851, 119.4525916976722897, -0.8552862985148331765 ) ) ;
#361 = CARTESIAN_POINT ( 'NONE',  ( 5.741009826001572947, -15.03722989464144355, 1.207582410354154145 ) ) ;
#362 = CARTESIAN_POINT ( 'NONE',  ( -5.332935381406168851, 115.7029491485442634, -0.1065653510733624160 ) ) ;
#363 = EDGE_CURVE ( 'NONE', #1559, #17444, #28654, .T. ) ;
#364 = CARTESIAN_POINT ( 'NONE',  ( -47.07934102874902749, 22.98505637820369429, -3.579966862081945145 ) ) ;
#365 = ORIENTED_EDGE ( 'NONE', *, *, #1402, .T. ) ;
#366 = CARTESIAN_POINT ( 'NONE',  ( -0.03153862713815891450, 157.4657262375360176, 1.578321868909182690 ) ) ;
#367 = CYLINDRICAL_SURFACE ( 'NONE', #41319, 0.2540000000000012248 ) ;
#368 = CARTESIAN_POINT ( 'NONE',  ( 5.011242901787458237, 115.7029491485453008, 1.398755999327908839 ) ) ;
#369 = CARTESIAN_POINT ( 'NONE',  ( -2.226623034866326289, 116.5145642697238344, 1.365476420808193536 ) ) ;
#370 = CARTESIAN_POINT ( 'NONE',  ( -3.240848860066210868, 23.83156553091082230, 7.781828003744739597 ) ) ;
#371 = CARTESIAN_POINT ( 'NONE',  ( 4.491182069977868174, 120.9948550335633115, 0.4087774027959020229 ) ) ;
#372 = CARTESIAN_POINT ( 'NONE',  ( 15.41192216945090898, 121.3506620944898060, -0.4643526128083734772 ) ) ;
#373 = FACE_OUTER_BOUND ( 'NONE', #39695, .T. ) ;
#374 = CARTESIAN_POINT ( 'NONE',  ( -58.36930655268525214, -0.2905277127126757453, 0.02713858147964411452 ) ) ;
#375 = EDGE_CURVE ( 'NONE', #4024, #2187, #33931, .T. ) ;
#376 = CARTESIAN_POINT ( 'NONE',  ( -3.302029177305334073, 159.4671159221996959, -0.06598240135525369754 ) ) ;
#377 = MECHANICAL_DESIGN_GEOMETRIC_PRESENTATION_REPRESENTATION (  '', ( #2412 ), #24155 ) ;
#378 = ORIENTED_EDGE ( 'NONE', *, *, #26047, .T. ) ;
#379 = CARTESIAN_POINT ( 'NONE',  ( -6.605722241764236280, 120.6764655449730981, -1.089203411656264553 ) ) ;
#380 = CARTESIAN_POINT ( 'NONE',  ( 2.112156314984550143, -15.50190413873483664, 5.930787297944131176 ) ) ;
#381 = CARTESIAN_POINT ( 'NONE',  ( -10.47888833811902920, 153.0637448873655728, -0.6176438153593468705 ) ) ;
#382 = CARTESIAN_POINT ( 'NONE',  ( 4.301541689408341362, -12.13840576482722078, 1.420409876116004222 ) ) ;
#383 = CARTESIAN_POINT ( 'NONE',  ( -15.08259856265902599, 121.6710330000183546, 0.7362983101480767845 ) ) ;
#384 = CARTESIAN_POINT ( 'NONE',  ( -7.784012322544769269, 122.6313477034873074, -0.1555430911242075831 ) ) ;
#385 = CARTESIAN_POINT ( 'NONE',  ( 15.19377495473398021, 156.0906695176550443, 0.3258312939631712868 ) ) ;
#386 = ORIENTED_EDGE ( 'NONE', *, *, #4860, .T. ) ;
#387 = CARTESIAN_POINT ( 'NONE',  ( -0.2480930319908794535, 10.21371511114847053, -4.635561276548324727 ) ) ;
#388 = CARTESIAN_POINT ( 'NONE',  ( -2.732111087507159475, 116.5293111276780849, -0.05459408159141344169 ) ) ;
#389 = DIRECTION ( 'NONE',  ( -0.9998004120163608288, 0.000000000000000000, -0.01997839162482747608 ) ) ;
#390 = DIRECTION ( 'NONE',  ( -0.8745520943968240202, 0.4849315768086553402, -6.829619984160650158E-16 ) ) ;
#391 = CARTESIAN_POINT ( 'NONE',  ( -5.945396627788727351, 120.3459718913957772, 0.7896226015759897354 ) ) ;
#392 = EDGE_CURVE ( 'NONE', #39604, #25560, #6092, .T. ) ;
#393 = CARTESIAN_POINT ( 'NONE',  ( 2.298459491326434900, 5.325542553220859787, -4.024866414273244430 ) ) ;
#394 = CARTESIAN_POINT ( 'NONE',  ( 13.98195098595639152, 120.5923583732999873, 1.177051350580812894 ) ) ;
#395 = CARTESIAN_POINT ( 'NONE',  ( -6.580517660824093636E-14, 85.69146620154573668, -4.881702850681514412E-18 ) ) ;
#397 = CARTESIAN_POINT ( 'NONE',  ( 3.107221341096611855, 117.9340107969418341, -0.6831876054667451736 ) ) ;
#396 = CARTESIAN_POINT ( 'NONE',  ( -14.38915334913366806, 80.27078028363496287, -1.270000000000000906 ) ) ;
#398 = CARTESIAN_POINT ( 'NONE',  ( 4.615940417482057967, 3.801270455692813410, -0.2501868467277520436 ) ) ;
#399 = CARTESIAN_POINT ( 'NONE',  ( -3.857972943339743388, 117.0975898859979054, -0.5726864223607189830 ) ) ;
#400 = ORIENTED_EDGE ( 'NONE', *, *, #39413, .T. ) ;
#401 = LINE ( 'NONE', #26358, #32745 ) ;
#402 = CARTESIAN_POINT ( 'NONE',  ( -15.34424630368622999, 148.0267799683202554, 0.1426181633603112453 ) ) ;
#403 = ADVANCED_FACE ( 'NONE', ( #6714 ), #2778, .F. ) ;
#404 = CARTESIAN_POINT ( 'NONE',  ( 2.294645149923727701, -15.44887909491890454, 5.922367448919703570 ) ) ;
#405 = CARTESIAN_POINT ( 'NONE',  ( -46.47694366848595848, 20.52739116796146135, 4.723822614977957635 ) ) ;
#406 = EDGE_CURVE ( 'NONE', #11585, #11444, #23712, .T. ) ;
#407 = CARTESIAN_POINT ( 'NONE',  ( -0.4875235816601763972, 105.8261742744559513, -5.318508263945600945 ) ) ;
#408 = ORIENTED_EDGE ( 'NONE', *, *, #24603, .T. ) ;
#409 = CARTESIAN_POINT ( 'NONE',  ( 19.37512658372770602, 148.3988719805327037, 2.511650730565585299 ) ) ;
#410 = CARTESIAN_POINT ( 'NONE',  ( 3.009276887026298031, 50.42904571186020490, -1.210121013456480377 ) ) ;
#411 = CARTESIAN_POINT ( 'NONE',  ( 9.049782359939477772, 124.0675141969884692, 0.1808361888366267212 ) ) ;
#412 = CARTESIAN_POINT ( 'NONE',  ( -6.906891541952466795, 117.5897289630162987, 0.4768185843253518463 ) ) ;
#413 = CARTESIAN_POINT ( 'NONE',  ( -8.406874004389072397, 27.76653542065474056, -0.1818807619882521764 ) ) ;
#414 = CARTESIAN_POINT ( 'NONE',  ( 18.50641704078256566, 154.1703991122031994, -0.1853567545699118246 ) ) ;
#415 = CARTESIAN_POINT ( 'NONE',  ( -5.813542725971299063, 56.51499999999999346, -4.384680539058477322 ) ) ;
#416 = CARTESIAN_POINT ( 'NONE',  ( -48.72131418994864305, 18.20897304993750865, 5.123370244626707759 ) ) ;
#417 = CARTESIAN_POINT ( 'NONE',  ( -49.93085365557847410, 21.08514737284949803, 1.613137678015111209 ) ) ;
#418 = CARTESIAN_POINT ( 'NONE',  ( 2.033723713787972009, -15.06201970758669262, 5.669216239185479012 ) ) ;
#419 = CARTESIAN_POINT ( 'NONE',  ( -53.17586183559576085, 10.67386474145934372, 4.017225210190868978 ) ) ;
#420 = CARTESIAN_POINT ( 'NONE',  ( -58.76893202732499333, -0.3048440090616499898, 0.2012342470266328676 ) ) ;
#421 = CARTESIAN_POINT ( 'NONE',  ( -4.380715115686576233, 118.1845394087038272, 0.4311985218286477073 ) ) ;
#422 = CARTESIAN_POINT ( 'NONE',  ( -58.11144429832075531, 0.1746852717545294142, -1.017628075538466478E-14 ) ) ;
#423 = PRODUCT_DEFINITION_SHAPE ( 'NONE', 'NONE',  #42165 ) ;
#424 = ORIENTED_EDGE ( 'NONE', *, *, #18869, .T. ) ;
#425 = CARTESIAN_POINT ( 'NONE',  ( -47.11704014324646295, 20.18577099567727373, 5.127035723291425207 ) ) ;
#426 = CARTESIAN_POINT ( 'NONE',  ( 8.373209961036389259, 119.8814485504210126, -1.110484165621906660 ) ) ;
#427 = CARTESIAN_POINT ( 'NONE',  ( -7.277551686224490446, 123.0424313102424492, -0.2142739940110133801 ) ) ;
#428 = CARTESIAN_POINT ( 'NONE',  ( 4.615868816244335981, 118.0368944136972971, 0.7918170276731736346 ) ) ;
#429 = CARTESIAN_POINT ( 'NONE',  ( -15.92638198489195211, 148.2453349897154737, -1.585317681524597733 ) ) ;
#430 = CARTESIAN_POINT ( 'NONE',  ( -2.661596506648667759, 115.7033367343655073, -1.688174420981334078 ) ) ;
#431 = CARTESIAN_POINT ( 'NONE',  ( -6.059261036834475256, 57.15000000000000568, 5.016499999999999737 ) ) ;
#432 = CARTESIAN_POINT ( 'NONE',  ( 5.069034061154215287, 114.3796182124986984, -1.753882200456532425 ) ) ;
#433 = EDGE_CURVE ( 'NONE', #15317, #27003, #40662, .T. ) ;
#434 = CARTESIAN_POINT ( 'NONE',  ( -13.21686059441255701, 128.5100244389050204, -1.738961528769450426 ) ) ;
#435 = CARTESIAN_POINT ( 'NONE',  ( -6.529493367164978770E-14, 72.99146620154573384, -7.899616498973244731E-18 ) ) ;
#436 = CARTESIAN_POINT ( 'NONE',  ( -0.02156508032628448243, 159.2730288250082538, 1.079204802879467850 ) ) ;
#437 = AXIS2_PLACEMENT_3D ( 'NONE', #20686, #27092, #27925 ) ;
#438 = CARTESIAN_POINT ( 'NONE',  ( 8.107080057029456555, 121.1657703571624012, -0.9663533087782769648 ) ) ;
#439 = CARTESIAN_POINT ( 'NONE',  ( -9.093843756948800205, 124.2201256219595251, -0.09191904702568627628 ) ) ;
#440 = CARTESIAN_POINT ( 'NONE',  ( 0.4343283552818534288, -9.202337043772711667, -4.603842121470758997 ) ) ;
#441 = CARTESIAN_POINT ( 'NONE',  ( 15.72348727998148732, 121.4292885696920621, 0.9291061361373527117 ) ) ;
#442 = DIRECTION ( 'NONE',  ( -5.188838149069472160E-16, 1.699382548006136559E-16, 1.000000000000000000 ) ) ;
#443 = CARTESIAN_POINT ( 'NONE',  ( 3.393951437975996743, -15.00105261681208901, 2.580228093083809071 ) ) ;
#444 = CARTESIAN_POINT ( 'NONE',  ( -19.24794053165973295, 147.9830121424878939, 1.736014841626597693 ) ) ;
#445 = CARTESIAN_POINT ( 'NONE',  ( 0.9605196170170531289, 3.153480984720312019, -0.1630338022177024171 ) ) ;
#446 = CARTESIAN_POINT ( 'NONE',  ( -15.70934801585154439, 121.2535323456646523, -0.8362899507430229251 ) ) ;
#447 = CARTESIAN_POINT ( 'NONE',  ( 0.9581433470387596962, -10.92824219907890360, 0.1848338584972420151 ) ) ;
#448 = B_SPLINE_CURVE_WITH_KNOTS ( 'NONE', 3,
 ( #28992, #13011, #471, #26642, #39436, #9405, #45, #10239, #29633, #3877 ),
 .UNSPECIFIED., .F., .F.,
 ( 4, 2, 2, 2, 4 ),
 ( 0.0001363461699588103975, 0.001296643753711174303, 0.002456941337463538263, 0.003617238921215902223, 0.004777536504968266616 ),
 .UNSPECIFIED. ) ;
#449 = VERTEX_POINT ( 'NONE', #15861 ) ;
#450 = VERTEX_POINT ( 'NONE', #12678 ) ;
#451 = CARTESIAN_POINT ( 'NONE',  ( -46.43071087740785430, 19.11736041196146374, 2.831212230509037031 ) ) ;
#452 = CARTESIAN_POINT ( 'NONE',  ( 7.253313547007579132, 123.0461458356614628, 0.2138788351844319036 ) ) ;
#453 = CARTESIAN_POINT ( 'NONE',  ( -9.588254403178179786, 123.8224200044116827, 0.4900104160083063043 ) ) ;
#454 = CARTESIAN_POINT ( 'NONE',  ( 3.745401017337624872, -13.88268793655436717, 4.204469449000409753 ) ) ;
#455 = CARTESIAN_POINT ( 'NONE',  ( 17.22014391273205547, 144.2986879860016529, -1.480874425454277166 ) ) ;
#456 = CARTESIAN_POINT ( 'NONE',  ( -12.70548372655400904, 122.4237789811383550, -1.817438969878694577 ) ) ;
#457 = DIRECTION ( 'NONE',  ( 5.188838149069472160E-16, -1.699382548006136559E-16, -1.000000000000000000 ) ) ;
#458 = EDGE_CURVE ( 'NONE', #25310, #10068, #9439, .T. ) ;
#459 = CARTESIAN_POINT ( 'NONE',  ( 3.197553254331486183, -13.99644925588092192, 2.254757065552156714 ) ) ;
#460 = CARTESIAN_POINT ( 'NONE',  ( -5.685436017834463840, 31.78209642239458788, 1.206328258593732272 ) ) ;
#461 = CARTESIAN_POINT ( 'NONE',  ( 11.88810549871044486, 151.9737369308441544, -0.07145411264644065119 ) ) ;
#462 = ORIENTED_EDGE ( 'NONE', *, *, #9429, .T. ) ;
#463 = CARTESIAN_POINT ( 'NONE',  ( -3.729000260451577731, 109.6950671057684588, 3.590446461533148170 ) ) ;
#464 = DIRECTION ( 'NONE',  ( 0.000000000000000000, 0.000000000000000000, 1.000000000000000000 ) ) ;
#465 = CARTESIAN_POINT ( 'NONE',  ( 4.560443946511397506, -11.68866997254031936, 0.6947937310338139216 ) ) ;
#466 = VECTOR ( 'NONE', #25714, 1000.000000000000000 ) ;
#467 = FACE_OUTER_BOUND ( 'NONE', #8526, .T. ) ;
#468 = TOROIDAL_SURFACE ( 'NONE', #24241, 0.7620000000000000107, 0.2540000000000000036 ) ;
#469 = CARTESIAN_POINT ( 'NONE',  ( 23.10641284836728815, 149.8968678342272653, 0.3080169626343542966 ) ) ;
#470 = CARTESIAN_POINT ( 'NONE',  ( -4.503688181905225463, 111.2539628214143903, 2.957939639849824776 ) ) ;
#471 = CARTESIAN_POINT ( 'NONE',  ( -3.877963262798508559, 118.0214462806859927, 0.8169714283994556903 ) ) ;
#472 = FACE_OUTER_BOUND ( 'NONE', #6866, .T. ) ;
#473 = CARTESIAN_POINT ( 'NONE',  ( -2.920903721094229244, 32.16307183204811082, 0.9800304932835676164 ) ) ;
#474 = CARTESIAN_POINT ( 'NONE',  ( 6.753855533487119978, 118.7881172115286148, 1.217991184693928863 ) ) ;
#475 = CARTESIAN_POINT ( 'NONE',  ( 3.308978306493741250, 24.09187545982852541, -3.235542752117448018 ) ) ;
#476 = CARTESIAN_POINT ( 'NONE',  ( -4.294125178196657622, -12.16697637372164564, -7.253078015393731981 ) ) ;
#477 = CARTESIAN_POINT ( 'NONE',  ( 5.557917761466073969, 117.8868906345641676, -0.8474712118571966490 ) ) ;
#478 = CARTESIAN_POINT ( 'NONE',  ( -0.6699575554302183988, 116.0160817474902331, -1.654834682733560491 ) ) ;
#479 = CARTESIAN_POINT ( 'NONE',  ( -5.749535644243536581, 78.89971493812807068, 5.036102041843079746 ) ) ;
#480 = CARTESIAN_POINT ( 'NONE',  ( -7.921807157844599878, 72.80702234259206307, 1.524000000000002242 ) ) ;
#481 = CARTESIAN_POINT ( 'NONE',  ( 0.8028203427309564821, 104.6144662015435216, 5.284712525425792506 ) ) ;
#482 = CIRCLE ( 'NONE', #24259, 6.350000000000004974 ) ;
#483 = CARTESIAN_POINT ( 'NONE',  ( -4.598301960400187127, 22.30806413504685537, 0.5496829067130363233 ) ) ;
#484 = DIRECTION ( 'NONE',  ( 5.188838149069472160E-16, -1.699382548006136559E-16, -1.000000000000000000 ) ) ;
#485 = CARTESIAN_POINT ( 'NONE',  ( -19.21741104974024594, 79.92823415920659613, -1.270000000000003348 ) ) ;
#486 = CARTESIAN_POINT ( 'NONE',  ( 2.744913772555794385, -12.89811552070117884, 0.2544447123532062038 ) ) ;
#487 = CARTESIAN_POINT ( 'NONE',  ( 3.315449255180855204, 124.9344662015457743, 0.06625056644921985260 ) ) ;
#488 = CARTESIAN_POINT ( 'NONE',  ( -19.54046365593634960, 128.7319734376252143, 0.5398260955622252721 ) ) ;
#489 = CARTESIAN_POINT ( 'NONE',  ( 4.976458764963934023, 117.4076063131326606, -0.8841951503558329595 ) ) ;
#490 = ORIENTED_EDGE ( 'NONE', *, *, #7890, .T. ) ;
#491 = CARTESIAN_POINT ( 'NONE',  ( -6.589702033682734540E-14, 87.97746620154572383, -4.338478393988997516E-18 ) ) ;
#492 = CONICAL_SURFACE ( 'NONE', #1854, 13.46199999999999619, 0.7853981633974482790 ) ;
#493 = ORIENTED_EDGE ( 'NONE', *, *, #10911, .T. ) ;
#494 = DIRECTION ( 'NONE',  ( -0.9998004120163608288, 0.000000000000000000, -0.01997839162482749342 ) ) ;
#495 = CARTESIAN_POINT ( 'NONE',  ( 4.389818247250405037, -15.68135102926887470, 3.766867903159812681 ) ) ;
#496 = CARTESIAN_POINT ( 'NONE',  ( -20.02944843481990844, 148.6304843473828043, 1.700276915703844427 ) ) ;
#497 = CARTESIAN_POINT ( 'NONE',  ( 19.32406529451186117, 152.1947311750261065, -1.288948053361433033 ) ) ;
#498 = CARTESIAN_POINT ( 'NONE',  ( 0.9442757308971110319, 28.15415565245834628, -0.2560175424543267297 ) ) ;
#499 = CARTESIAN_POINT ( 'NONE',  ( -58.67914983968596232, -0.3139907887120958474, -0.3103399889725807492 ) ) ;
#500 = VERTEX_POINT ( 'NONE', #19477 ) ;
#501 = CARTESIAN_POINT ( 'NONE',  ( -4.881263862402589027, 117.4111615705287477, -1.144645852924967455 ) ) ;
#502 = AXIS2_PLACEMENT_3D ( 'NONE', #34156, #17941, #1783 ) ;
#503 = CARTESIAN_POINT ( 'NONE',  ( 0.3562073053188078986, 119.8383472832136931, 0.7014361403029917286 ) ) ;
#504 = CARTESIAN_POINT ( 'NONE',  ( 4.807157299559274399, 117.4049453230273343, 1.198158832445191724 ) ) ;
#505 = CARTESIAN_POINT ( 'NONE',  ( -16.58715205660940128, 148.2569838091642964, 1.247478730927799928 ) ) ;
#506 = CARTESIAN_POINT ( 'NONE',  ( -7.213960532363663525, 83.56599999999998829, -1.904999999999999805 ) ) ;
#507 = CARTESIAN_POINT ( 'NONE',  ( 18.50543525367148945, 148.3462492009778373, -1.698196615343024574 ) ) ;
#508 = CARTESIAN_POINT ( 'NONE',  ( -14.76979702826417196, 154.6636077862465015, -2.174438252133946481 ) ) ;
#509 = CARTESIAN_POINT ( 'NONE',  ( -57.69570286664291103, 2.558035660193719529, -1.875687456014384802 ) ) ;
#510 = ORIENTED_EDGE ( 'NONE', *, *, #6687, .F. ) ;
#511 = CARTESIAN_POINT ( 'NONE',  ( 4.371200167350260735, 118.1836009977106272, -0.4408363070965656827 ) ) ;
#512 = CARTESIAN_POINT ( 'NONE',  ( 8.277497327054904375, 122.7564308547279666, -0.2971990107970637895 ) ) ;
#513 = B_SPLINE_CURVE_WITH_KNOTS ( 'NONE', 3,
 ( #3567, #25496, #16528, #3780, #22481, #13341 ),
 .UNSPECIFIED., .F., .F.,
 ( 4, 2, 4 ),
 ( 0.000000000000000000, 0.0001547602548093537271, 0.0003095205096187074543 ),
 .UNSPECIFIED. ) ;
#514 = VERTEX_POINT ( 'NONE', #32485 ) ;
#515 = CARTESIAN_POINT ( 'NONE',  ( -17.73873607445684186, 146.7645792007554633, -2.242890973037755309 ) ) ;
#516 = CARTESIAN_POINT ( 'NONE',  ( 2.233744238265779281, -15.22787141332636374, 5.055619554762198931 ) ) ;
#517 = CARTESIAN_POINT ( 'NONE',  ( -3.676066591212550527, 105.1230425560760011, -3.867827736016857809 ) ) ;
#518 = VECTOR ( 'NONE', #3109, 1000.000000000000114 ) ;
#519 = CARTESIAN_POINT ( 'NONE',  ( -58.36994270878681590, -0.2918297664328134422, 0.01629410684326380171 ) ) ;
#520 = CARTESIAN_POINT ( 'NONE',  ( 2.298459491326434900, 5.325542553220859787, -4.024866414273244430 ) ) ;
#521 = CARTESIAN_POINT ( 'NONE',  ( 17.47633463031920797, 147.2926247242496345, 2.162249527696345375 ) ) ;
#522 = CARTESIAN_POINT ( 'NONE',  ( -2.535133856325437751, 31.19167863242842742, 1.091392955096686768 ) ) ;
#523 = CARTESIAN_POINT ( 'NONE',  ( 3.263621351691376571, 8.939281053574255509, -3.290156819607050753 ) ) ;
#524 = CARTESIAN_POINT ( 'NONE',  ( 11.89867495700680067, 130.3805625696445816, 0.3456363086864550627 ) ) ;
#525 = DIRECTION ( 'NONE',  ( -5.188838149069471174E-16, 1.699382548006136313E-16, 1.000000000000000000 ) ) ;
#526 = VECTOR ( 'NONE', #36681, 1000.000000000000000 ) ;
#527 = CARTESIAN_POINT ( 'NONE',  ( -55.83515739322318439, 4.224161455597882586, -1.000857388952954637E-14 ) ) ;
#528 = CARTESIAN_POINT ( 'NONE',  ( 8.798384430222753849, 117.6845712652260545, 0.1566951038920376127 ) ) ;
#529 = CARTESIAN_POINT ( 'NONE',  ( 5.078986093043054595, 66.13346620154574396, 0.1014902294541243921 ) ) ;
#530 = CARTESIAN_POINT ( 'NONE',  ( -6.640726327341849406E-14, 100.6774662015457409, -1.320564745697255449E-18 ) ) ;
#531 = CARTESIAN_POINT ( 'NONE',  ( -7.842268484490568348, 73.30875693322846587, -1.269999999999996243 ) ) ;
#532 = CARTESIAN_POINT ( 'NONE',  ( -5.177913976931302287, 77.01756250000002524, 5.372099999999996989 ) ) ;
#533 = DIRECTION ( 'NONE',  ( -1.000000000000000000, 1.011795553208986377E-16, 0.000000000000000000 ) ) ;
#534 = CARTESIAN_POINT ( 'NONE',  ( -57.40598286442868670, 3.481741809872221260, 1.566274799519910887 ) ) ;
#535 = CARTESIAN_POINT ( 'NONE',  ( -58.24002838079472610, 0.001074765447070524793, 0.6562585879479657658 ) ) ;
#536 = CARTESIAN_POINT ( 'NONE',  ( -5.806485631242245482, 116.9771394561422539, 0.05772921648981179515 ) ) ;
#537 = VERTEX_POINT ( 'NONE', #16279 ) ;
#538 = CARTESIAN_POINT ( 'NONE',  ( -51.27035844764527184, 15.91047978596967560, -4.316378984520668816 ) ) ;
#539 = CARTESIAN_POINT ( 'NONE',  ( 6.066927103458539250, 121.4399465332669052, 0.1138985383779980987 ) ) ;
#540 = ORIENTED_EDGE ( 'NONE', *, *, #11582, .F. ) ;
#541 = CARTESIAN_POINT ( 'NONE',  ( -5.237832120027548832, 115.7029491485453860, -1.023639123012231034 ) ) ;
#542 = CARTESIAN_POINT ( 'NONE',  ( -15.26387433774262803, 148.0131224598485744, -0.4327379813662101671 ) ) ;
#543 = CARTESIAN_POINT ( 'NONE',  ( 5.090702275550843758, -14.49510550894771121, 4.025111979839017806 ) ) ;
#544 = CARTESIAN_POINT ( 'NONE',  ( -18.63828149932700740, 131.8045874826418071, 1.403896228398082258 ) ) ;
#545 = CARTESIAN_POINT ( 'NONE',  ( 3.465721614298269415, 18.43485028915299750, -3.064284189100199729 ) ) ;
#546 = CARTESIAN_POINT ( 'NONE',  ( 14.67516008282137108, 120.3119357913517291, 0.6057029122735548832 ) ) ;
#547 = CIRCLE ( 'NONE', #3954, 0.3810000000000032250 ) ;
#548 = CARTESIAN_POINT ( 'NONE',  ( 2.077680606031648836, -15.60673140158441718, 5.873410514533511595 ) ) ;
#549 = CARTESIAN_POINT ( 'NONE',  ( 4.619096255015035624, 27.05588869245799089, -0.3994036469054788596 ) ) ;
#550 = CARTESIAN_POINT ( 'NONE',  ( -0.9568942166608355171, -5.529307923341535869, 0.1941686039811585662 ) ) ;
#551 = CARTESIAN_POINT ( 'NONE',  ( -23.31615218609863760, 149.0517038676186417, -0.6965919665178228470 ) ) ;
#552 = CARTESIAN_POINT ( 'NONE',  ( 6.059261036834406866, 57.14999999999999858, -5.016499999999999737 ) ) ;
#553 = DIRECTION ( 'NONE',  ( 0.9876665170007974393, -0.1565721916417901483, 8.537024980200831679E-16 ) ) ;
#554 = CARTESIAN_POINT ( 'NONE',  ( 2.189241082030666696, 116.2106850124662998, 0.08689766813257669698 ) ) ;
#555 = ORIENTED_EDGE ( 'NONE', *, *, #38050, .F. ) ;
#556 = CARTESIAN_POINT ( 'NONE',  ( -17.70889067045670373, 148.6960320134204210, 1.618934763233637719 ) ) ;
#557 = CARTESIAN_POINT ( 'NONE',  ( -58.01365450750562047, 0.4748094611197187787, -0.8404086423206994505 ) ) ;
#558 = CARTESIAN_POINT ( 'NONE',  ( 13.54946078406806542, 121.5020190402118203, 1.609302047640725153 ) ) ;
#559 = CARTESIAN_POINT ( 'NONE',  ( 10.86053312202623289, 155.9024031350590462, -1.736732359437422657 ) ) ;
#560 = CARTESIAN_POINT ( 'NONE',  ( -0.9711860326002300647, -2.018343210913434493, -0.07513956953184577903 ) ) ;
#561 = CARTESIAN_POINT ( 'NONE',  ( -14.08892660837143396, 121.3807765770047666, -1.491720297716245369 ) ) ;
#562 = CARTESIAN_POINT ( 'NONE',  ( 4.543474876628542880, 118.0888849834743155, -0.5958067675172851185 ) ) ;
#563 = CARTESIAN_POINT ( 'NONE',  ( -3.527324519276147541, 50.63946620154572997, 1.707870599815379364 ) ) ;
#564 = EDGE_CURVE ( 'NONE', #9964, #36869, #25095, .T. ) ;
#565 = CARTESIAN_POINT ( 'NONE',  ( 16.45208226155726550, 147.1833543704171348, -0.9460114105336799861 ) ) ;
#566 = CARTESIAN_POINT ( 'NONE',  ( -4.591655703643919395, 121.2030596905490540, -0.06445270968432167957 ) ) ;
#567 = ORIENTED_EDGE ( 'NONE', *, *, #41507, .F. ) ;
#568 = CARTESIAN_POINT ( 'NONE',  ( -18.52244049926389025, 148.0519089404264150, -2.440181727699358483 ) ) ;
#569 = CARTESIAN_POINT ( 'NONE',  ( 2.674787014790545481, -15.76824019788006304, 5.299902074303234123 ) ) ;
#570 = CARTESIAN_POINT ( 'NONE',  ( -5.317765600491472178, 115.7029491485453718, 0.5108555054852879085 ) ) ;
#571 = CARTESIAN_POINT ( 'NONE',  ( -4.547255095654547219, 118.0358984568298268, -0.8569604299583566398 ) ) ;
#572 = CARTESIAN_POINT ( 'NONE',  ( -47.16890147375937659, 22.20336809214646578, -4.187060126831891438 ) ) ;
#573 = LINE ( 'NONE', #23318, #10916 ) ;
#574 = CARTESIAN_POINT ( 'NONE',  ( 12.61679319894177809, 153.7453525671159298, 2.178569956567485200 ) ) ;
#575 = CARTESIAN_POINT ( 'NONE',  ( -27.88833342972739615, 78.11058938209563962, -1.270000000000007345 ) ) ;
#576 =( BOUNDED_CURVE ( )  B_SPLINE_CURVE ( 3, ( #39758, #26535, #19706, #13752, #26747, #39538, #23315 ),
 .UNSPECIFIED., .F., .T. ) 
 B_SPLINE_CURVE_WITH_KNOTS ( ( 4, 3, 4 ),
 ( 0.9253411388830656836, 0.9999999999991224797, 1.000260013143586590 ),
 .UNSPECIFIED. ) 
 CURVE ( )  GEOMETRIC_REPRESENTATION_ITEM ( )  RATIONAL_B_SPLINE_CURVE ( ( 0.7459561198782405089, 0.8157735584700518405, 0.9004548518439716709, 1.000000000000000000, 0.9996533158073767078, 0.9993068118996475402, 0.9989604882768124972 ) ) 
 REPRESENTATION_ITEM ( '' )  );
#577 = CARTESIAN_POINT ( 'NONE',  ( 11.74288454345096788, 118.7273140689154616, 0.2346507796901760867 ) ) ;
#578 =( GEOMETRIC_REPRESENTATION_CONTEXT ( 3 ) GLOBAL_UNCERTAINTY_ASSIGNED_CONTEXT ( ( #38497 ) ) GLOBAL_UNIT_ASSIGNED_CONTEXT ( ( #8767, #25159, #21514 ) ) REPRESENTATION_CONTEXT ( 'NONE', 'WORKASPACE' ) );
#579 = CARTESIAN_POINT ( 'NONE',  ( -5.114723271350774425, 118.2545999410811106, 0.5144770513779390875 ) ) ;
#580 = CARTESIAN_POINT ( 'NONE',  ( -8.093932337251422027, 31.18171294578705854, -2.467657647566553258 ) ) ;
#581 = CARTESIAN_POINT ( 'NONE',  ( 12.02994987064020371, 151.9703418938154584, 0.9209848757141020359 ) ) ;
#582 = CARTESIAN_POINT ( 'NONE',  ( 14.73113557689540798, 120.8948172685174001, -0.5329945393104402740 ) ) ;
#583 = CARTESIAN_POINT ( 'NONE',  ( 5.965356522962858676, 57.14999999999998437, 5.016499999999999737 ) ) ;
#584 = ORIENTED_EDGE ( 'NONE', *, *, #327, .T. ) ;
#585 = FACE_BOUND ( 'NONE', #36365, .T. ) ;
#586 = EDGE_CURVE ( 'NONE', #26988, #6334, #37150, .T. ) ;
#587 = CARTESIAN_POINT ( 'NONE',  ( -23.45022726768242549, 146.8469795362756258, -0.4427096500589554617 ) ) ;
#588 = VERTEX_POINT ( 'NONE', #40151 ) ;
#589 = CARTESIAN_POINT ( 'NONE',  ( 6.820670703200751639, 121.2541756018108714, -0.6270318998841969416 ) ) ;
#590 = CARTESIAN_POINT ( 'NONE',  ( -6.085514072855107208E-14, 88.48546620154573361, 9.693882645925084535E-17 ) ) ;
#591 = CARTESIAN_POINT ( 'NONE',  ( -15.85571122620645390, 146.2799285973741519, -0.7709397856434241358 ) ) ;
#592 = CARTESIAN_POINT ( 'NONE',  ( 3.951736590037845609, -12.73914099834651203, 2.215835717905272784 ) ) ;
#593 = CARTESIAN_POINT ( 'NONE',  ( -14.74288075364469464, 121.6338672040446767, 0.8423781477486337321 ) ) ;
#594 = CARTESIAN_POINT ( 'NONE',  ( -1.561582345843753217, 156.2588034088681184, -0.03120413162939504950 ) ) ;
#595 = CARTESIAN_POINT ( 'NONE',  ( 8.067923148479861695, 158.6666700270975525, 0.2162342711943723572 ) ) ;
#596 = ORIENTED_EDGE ( 'NONE', *, *, #19285, .T. ) ;
#597 = CARTESIAN_POINT ( 'NONE',  ( -2.070226828232369254, -8.352695179381779411, -4.151654383260235726 ) ) ;
#598 = CARTESIAN_POINT ( 'NONE',  ( 4.980330008247731755, 105.1217463992231984, 1.919414732010889413 ) ) ;
#599 = DIRECTION ( 'NONE',  ( 1.000000000000000000, 0.000000000000000000, -3.035386659626960118E-16 ) ) ;
#600 = CARTESIAN_POINT ( 'NONE',  ( 3.884039321165668746, 109.3893297329433381, 3.664381571631352141 ) ) ;
#601 = CARTESIAN_POINT ( 'NONE',  ( 6.775796848276115725, 120.4130524060792169, 1.184928199607375943 ) ) ;
#602 = CARTESIAN_POINT ( 'NONE',  ( 1.391598188199559161, 15.24595356501894017, -4.406646451508545503 ) ) ;
#603 = CARTESIAN_POINT ( 'NONE',  ( 14.80859988127084925, 121.7713424311148032, 1.438396347550856991 ) ) ;
#604 = CARTESIAN_POINT ( 'NONE',  ( -47.85244527695891037, 19.39403540832955386, -5.219971639306618449 ) ) ;
#606 = CARTESIAN_POINT ( 'NONE',  ( 6.856369467415130536, 157.9234729166680040, -1.555392933271966927 ) ) ;
#605 = CARTESIAN_POINT ( 'NONE',  ( 6.059261036834405978, 57.14999999999999858, 5.016500000000000625 ) ) ;
#607 = CARTESIAN_POINT ( 'NONE',  ( 2.099109474952898236, -4.195072059908932616, -4.137704358558784712 ) ) ;
#608 = CARTESIAN_POINT ( 'NONE',  ( -18.14731753714293205, 154.1160801429439857, -1.378418044792611319 ) ) ;
#609 = CARTESIAN_POINT ( 'NONE',  ( -5.177913976931298734, 78.94499979771843812, 5.372100000000002318 ) ) ;
#610 = EDGE_CURVE ( 'NONE', #41136, #7000, #5386, .T. ) ;
#611 = ORIENTED_EDGE ( 'NONE', *, *, #26444, .T. ) ;
#612 = CARTESIAN_POINT ( 'NONE',  ( -14.75792966017397312, 148.8440819608433969, 0.1510343195432204133 ) ) ;
#614 = CARTESIAN_POINT ( 'NONE',  ( 3.432440172432007053, -15.40242305089609154, 5.447709670318832131 ) ) ;
#613 = AXIS2_PLACEMENT_3D ( 'NONE', #33524, #14532, #31148 ) ;
#615 = AXIS2_PLACEMENT_3D ( 'NONE', #13234, #13012, #26005 ) ;
#616 = DIRECTION ( 'NONE',  ( -0.4849315768086427392, -0.8745520943968311256, -4.371515779989697137E-15 ) ) ;
#617 = CARTESIAN_POINT ( 'NONE',  ( 3.075357915497110017, -13.94103813162880989, 1.416127232796946966 ) ) ;
#618 = ADVANCED_FACE ( 'NONE', ( #13731 ), #41434, .T. ) ;
#619 = ORIENTED_EDGE ( 'NONE', *, *, #5064, .T. ) ;
#620 = CARTESIAN_POINT ( 'NONE',  ( 19.13795181553994951, 149.5120288530235655, 2.492102325696694987 ) ) ;
#621 = DIRECTION ( 'NONE',  ( -5.206863593109713661E-17, 1.000000000000000000, -1.077750396879097183E-30 ) ) ;
#622 = DIRECTION ( 'NONE',  ( -4.017660918040594346E-17, 1.000000000000000000, 2.376309959284834438E-19 ) ) ;
#623 = CARTESIAN_POINT ( 'NONE',  ( -22.36672427266407936, 142.2114994846844240, 0.8677673306393178798 ) ) ;
#624 = CARTESIAN_POINT ( 'NONE',  ( 5.482275759465073506, 24.31437370403141784, -6.390863428313894978 ) ) ;
#625 = CARTESIAN_POINT ( 'NONE',  ( 8.534279067096685267, 122.4751019636825049, 0.9739960529120708088 ) ) ;
#626 = CARTESIAN_POINT ( 'NONE',  ( 21.27466159042545613, 132.4531229209162575, -0.1171209876626083529 ) ) ;
#627 = CARTESIAN_POINT ( 'NONE',  ( -6.059261036834475256, 57.14999999999997016, -5.016499999999997961 ) ) ;
#628 = CARTESIAN_POINT ( 'NONE',  ( -4.958249173792594888, 117.6484007699707206, 0.6696174729038590900 ) ) ;
#629 = CARTESIAN_POINT ( 'NONE',  ( -47.23483502501005660, 23.02499599010462816, 3.263444997004413484 ) ) ;
#630 = CARTESIAN_POINT ( 'NONE',  ( -4.757248705868250660, 117.4032733054483799, -1.206458839318209408 ) ) ;
#631 = CARTESIAN_POINT ( 'NONE',  ( -55.03109054507046238, 6.816801101491506643, 3.135084751894912980 ) ) ;
#632 = CARTESIAN_POINT ( 'NONE',  ( -58.18166364753805908, 0.6689161199004037828, 1.158115574925229874 ) ) ;
#633 = EDGE_CURVE ( 'NONE', #4427, #35981, #26379, .T. ) ;
#634 = CARTESIAN_POINT ( 'NONE',  ( -4.483631243783302800, 118.1297507219403826, 0.5359420136376905619 ) ) ;
#635 = DIRECTION ( 'NONE',  ( -4.017660918040594346E-17, 1.000000000000000000, 2.376309959284834438E-19 ) ) ;
#636 = EDGE_LOOP ( 'NONE', ( #9709, #30418, #35800, #17027 ) ) ;
#637 = CARTESIAN_POINT ( 'NONE',  ( -43.24646561529713296, 21.63922848039483071, 2.381786957946262273 ) ) ;
#638 = ADVANCED_FACE ( 'NONE', ( #39516 ), #20691, .T. ) ;
#639 = CIRCLE ( 'NONE', #1999, 5.080000000000006288 ) ;
#640 = CARTESIAN_POINT ( 'NONE',  ( 3.984814155878985797, 119.0966718691183956, -0.7651888519286457191 ) ) ;
#641 = CARTESIAN_POINT ( 'NONE',  ( -2.913298842129383281, 107.8271213589905386, -4.473571949258134950 ) ) ;
#642 = CARTESIAN_POINT ( 'NONE',  ( 4.528137707338466100, 118.0895881931546825, 0.7656966491790531126 ) ) ;
#643 = CARTESIAN_POINT ( 'NONE',  ( -16.14046266016593023, 146.7365623387580342, -1.292066526867235776 ) ) ;
#644 = EDGE_CURVE ( 'NONE', #33497, #18509, #30539, .T. ) ;
#645 = DIRECTION ( 'NONE',  ( -0.01997839162482737546, -1.040247600000940825E-18, 0.9998004120163610509 ) ) ;
#646 = CARTESIAN_POINT ( 'NONE',  ( 5.274668375481190274, 116.0897965414613964, -1.029904101180854514 ) ) ;
#647 = CARTESIAN_POINT ( 'NONE',  ( -12.92681072397291864, 152.2092440956282076, -1.775214794609845326 ) ) ;
#648 = CARTESIAN_POINT ( 'NONE',  ( -5.306918775014303868, 116.0444662015457169, 1.063204892635948307 ) ) ;
#649 = CARTESIAN_POINT ( 'NONE',  ( -0.008148259816615344500, 159.5682499516715040, 0.4077722408685187649 ) ) ;
#650 = DIRECTION ( 'NONE',  ( -4.017660918040594346E-17, 1.000000000000000000, 2.376309959284834438E-19 ) ) ;
#651 = CARTESIAN_POINT ( 'NONE',  ( -4.198627658836969090, 155.8781008607725767, 0.05950270295165668161 ) ) ;
#652 = CARTESIAN_POINT ( 'NONE',  ( 3.895047602890354010, -2.730319773039217690, 2.488009491782988469 ) ) ;
#653 = CARTESIAN_POINT ( 'NONE',  ( 6.894332492628085340, 117.4533518774869947, 0.6472591412684411960 ) ) ;
#654 = CARTESIAN_POINT ( 'NONE',  ( 5.219197883255967341, 105.1221402665274525, -1.156025970443059991 ) ) ;
#655 = CARTESIAN_POINT ( 'NONE',  ( 2.944601773672358203, -15.01875103642165499, 4.065120351795452613 ) ) ;
#656 = CARTESIAN_POINT ( 'NONE',  ( -11.73216920131865670, 154.7938929448963279, 1.733846838993656547 ) ) ;
#657 = CARTESIAN_POINT ( 'NONE',  ( -0.8194340683325834762, 6.824753112428224355, -0.5254904297167376503 ) ) ;
#658 = CARTESIAN_POINT ( 'NONE',  ( -23.13755856728675653, 142.6111785389246336, -1.063510652947476931 ) ) ;
#659 = CARTESIAN_POINT ( 'NONE',  ( 0.8486417380921021936, -9.850041244260159701, -0.4793021190969105616 ) ) ;
#660 = ORIENTED_EDGE ( 'NONE', *, *, #1717, .T. ) ;
#661 = CARTESIAN_POINT ( 'NONE',  ( -45.37978287637889707, 19.43610829578849675, 1.699483007375117261 ) ) ;
#662 = CARTESIAN_POINT ( 'NONE',  ( 5.131660560485880929, 115.4810986995850755, 1.508144361588664051 ) ) ;
#663 = CONTEXT_DEPENDENT_SHAPE_REPRESENTATION ( #35242, #33422 ) ;
#664 = CARTESIAN_POINT ( 'NONE',  ( -1.530333064024551160, 120.5919059741422217, 0.2783515840389084728 ) ) ;
#665 = CARTESIAN_POINT ( 'NONE',  ( 4.230101149094581459, -11.70512343023444402, 0.7321030916320588888 ) ) ;
#666 = CARTESIAN_POINT ( 'NONE',  ( 17.26811951358304498, 148.1877419978735873, -1.462309189260816655 ) ) ;
#667 = CARTESIAN_POINT ( 'NONE',  ( -13.59052456474564430, 154.1626644387825991, -2.292254590369200873 ) ) ;
#668 = CARTESIAN_POINT ( 'NONE',  ( 1.938979755120314952, 104.6144662015456959, 4.428504999179026846 ) ) ;
#669 = CARTESIAN_POINT ( 'NONE',  ( 3.220330141560203696, -14.30903721375789317, 2.546581355196453345 ) ) ;
#670 = CARTESIAN_POINT ( 'NONE',  ( -4.860329684765736680, 117.5461367057571636, -1.119675193854307249 ) ) ;
#671 = CARTESIAN_POINT ( 'NONE',  ( 9.105893302116596644, 123.9936668703698075, 0.02250835519154697345 ) ) ;
#672 = ORIENTED_EDGE ( 'NONE', *, *, #20953, .T. ) ;
#673 = CARTESIAN_POINT ( 'NONE',  ( -3.563491213075201891, 108.3861669196204360, 3.960735735213689157 ) ) ;
#674 = DIRECTION ( 'NONE',  ( -5.188838149069472160E-16, 1.699382548006136559E-16, 1.000000000000000000 ) ) ;
#675 = AXIS2_PLACEMENT_3D ( 'NONE', #9781, #12563, #22749 ) ;
#676 = DIRECTION ( 'NONE',  ( 6.353134868986659519E-16, -1.000000000000000000, -0.000000000000000000 ) ) ;
#677 = EDGE_CURVE ( 'NONE', #32690, #22720, #25591, .T. ) ;
#678 = CARTESIAN_POINT ( 'NONE',  ( 22.98049992366328809, 150.1579452496398801, 0.3057203305217678357 ) ) ;
#679 = CARTESIAN_POINT ( 'NONE',  ( -5.302326897023659669, 116.4520502601644409, 0.8833424955642700249 ) ) ;
#680 = CARTESIAN_POINT ( 'NONE',  ( -1.614223865627344434, 118.7629491485454167, 1.182319156186325548 ) ) ;
#681 = CARTESIAN_POINT ( 'NONE',  ( 11.42297701379736097, 55.88459609804032624, 4.463034230327253660 ) ) ;
#682 = CARTESIAN_POINT ( 'NONE',  ( -4.975175664203050907, 32.06598106186588382, 0.7459204072935275986 ) ) ;
#683 = CARTESIAN_POINT ( 'NONE',  ( 17.00694855514563741, 128.5677977248401476, 2.111551361116177361 ) ) ;
#684 = CARTESIAN_POINT ( 'NONE',  ( 4.518289034361447243, 23.24227448397437001, -0.9983406360900146659 ) ) ;
#685 = CARTESIAN_POINT ( 'NONE',  ( 7.419718609332475623, 16.48482641057854892, 3.982871883899435250 ) ) ;
#686 = CARTESIAN_POINT ( 'NONE',  ( -8.622446851455114469, 118.4541269161059773, -1.064047717557140116 ) ) ;
#687 = CARTESIAN_POINT ( 'NONE',  ( -1.585818144368670746, 119.1892773189224783, -0.7268676395674203983 ) ) ;
#688 = CARTESIAN_POINT ( 'NONE',  ( -6.057513928997661168, 86.35999999999998522, 1.904999999999996030 ) ) ;
#689 = CARTESIAN_POINT ( 'NONE',  ( -3.682264917456323783, 84.67546620154573134, -0.07358041635423968885 ) ) ;
#690 = CARTESIAN_POINT ( 'NONE',  ( -4.247245584637960647, 22.75789413176893206, 1.861891798430825862 ) ) ;
#691 = EDGE_CURVE ( 'NONE', #32986, #18705, #32617, .T. ) ;
#692 = DIRECTION ( 'NONE',  ( 0.1565721916417901483, 0.9876665170007974393, 0.000000000000000000 ) ) ;
#693 = CARTESIAN_POINT ( 'NONE',  ( -15.56076557484951906, 120.7233670659557419, -0.3109411287493939469 ) ) ;
#694 = CARTESIAN_POINT ( 'NONE',  ( 2.781118144868611974, -14.77119122201073154, 4.489572933734862659 ) ) ;
#695 = CARTESIAN_POINT ( 'NONE',  ( 3.315740949751757149, 124.7872298565087021, 0.06001882965729966185 ) ) ;
#696 = CARTESIAN_POINT ( 'NONE',  ( -22.01496335533490978, 136.8935083344700558, 0.5016514318445888243 ) ) ;
#697 = AXIS2_PLACEMENT_3D ( 'NONE', #7791, #34985, #20752 ) ;
#698 = ADVANCED_FACE ( 'NONE', ( #22165 ), #38397, .F. ) ;
#699 = CARTESIAN_POINT ( 'NONE',  ( -4.095482865093057256, 71.62450171983788039, -1.523999999999994026 ) ) ;
#700 = VERTEX_POINT ( 'NONE', #35196 ) ;
#701 = CARTESIAN_POINT ( 'NONE',  ( -8.539387426415398608, 74.43734692935288422, 1.270000000000002460 ) ) ;
#702 = VERTEX_POINT ( 'NONE', #31989 ) ;
#703 = CARTESIAN_POINT ( 'NONE',  ( 1.122158211225881885, 34.81801111161350804, -0.09678150280622686841 ) ) ;
#704 = CARTESIAN_POINT ( 'NONE',  ( 3.555176734920527437, -15.70662665601262020, 4.164229356387482817 ) ) ;
#705 = CARTESIAN_POINT ( 'NONE',  ( -4.664640489119783240, 158.0471523224993859, 1.621167461353164807 ) ) ;
#706 = CARTESIAN_POINT ( 'NONE',  ( 14.11223987312410522, 121.6707806233237363, -1.016201875498928153 ) ) ;
#707 = CARTESIAN_POINT ( 'NONE',  ( 4.560200836559435977, -11.68919918208664122, 0.6963878748952898601 ) ) ;
#708 = CARTESIAN_POINT ( 'NONE',  ( -58.61966295912883140, -0.2719594648587958519, -0.4054877843427013850 ) ) ;
#709 = ORIENTED_EDGE ( 'NONE', *, *, #5033, .T. ) ;
#710 = CARTESIAN_POINT ( 'NONE',  ( -4.784543075752243801, 117.4060574113812265, -1.200192385861798883 ) ) ;
#711 = CARTESIAN_POINT ( 'NONE',  ( 2.096106201831287930, 122.9394440205640961, 0.1965313455681951260 ) ) ;
#712 = CARTESIAN_POINT ( 'NONE',  ( -16.63213601294270561, 144.0643239018434940, 1.266953209168787176 ) ) ;
#713 = DIRECTION ( 'NONE',  ( 0.4849315768086534528, 0.8745520943968250194, 1.030032898892974942E-16 ) ) ;
#714 = CARTESIAN_POINT ( 'NONE',  ( 16.09548914235255168, 150.9843922791743296, -1.671617783681723424 ) ) ;
#715 = CARTESIAN_POINT ( 'NONE',  ( -8.897726962874944689, 119.7003323559047061, -1.444919796022273051 ) ) ;
#716 = DIRECTION ( 'NONE',  ( -4.017660918040594346E-17, 1.000000000000000000, 2.376309959284832031E-19 ) ) ;
#717 = ORIENTED_EDGE ( 'NONE', *, *, #6839, .T. ) ;
#718 = CARTESIAN_POINT ( 'NONE',  ( 4.529352846675309685, 118.1222063800068867, -0.4828943068153593865 ) ) ;
#719 = CARTESIAN_POINT ( 'NONE',  ( 15.67979071779206457, 147.9168465093495399, -0.5330609057418901342 ) ) ;
#720 = EDGE_LOOP ( 'NONE', ( #24810, #4180, #22560, #38384 ) ) ;
#721 = CARTESIAN_POINT ( 'NONE',  ( 3.208040786519721355, -14.49217647381938257, 1.686337311097440894 ) ) ;
#722 = CARTESIAN_POINT ( 'NONE',  ( -4.030424611563636184, 105.1222741834141345, -3.510259462146176013 ) ) ;
#723 = FACE_OUTER_BOUND ( 'NONE', #37524, .T. ) ;
#724 = CARTESIAN_POINT ( 'NONE',  ( -1.290833045837797455, 0.8901568857254957834, 4.466177308409287505 ) ) ;
#725 = CARTESIAN_POINT ( 'NONE',  ( 9.120583164541022470, 155.0058477609193801, 1.824713877226967984 ) ) ;
#726 = CARTESIAN_POINT ( 'NONE',  ( 2.802822085653141837, 37.46604678162410096, -0.5169543402998219017 ) ) ;
#727 = CARTESIAN_POINT ( 'NONE',  ( 2.003160574663116034, 15.61121511114846960, 4.187759092076685619 ) ) ;
#728 = CARTESIAN_POINT ( 'NONE',  ( 14.68908181661150358, 148.8396455022467535, 0.5202010721049652453 ) ) ;
#729 = CARTESIAN_POINT ( 'NONE',  ( -3.836572904814790075, 108.9297306800247895, 3.710741818055595775 ) ) ;
#730 = EDGE_CURVE ( 'NONE', #19419, #35057, #10104, .T. ) ;
#731 = CARTESIAN_POINT ( 'NONE',  ( -55.75614604655159923, 4.795084387130554404, -1.238208353029769393 ) ) ;
#732 = CARTESIAN_POINT ( 'NONE',  ( 5.563298544691044789, 116.7240770658327449, -0.06738706188448287393 ) ) ;
#733 = DIRECTION ( 'NONE',  ( -0.8745520943968235761, 0.4849315768086558398, -4.268512490100410909E-16 ) ) ;
#734 = DIRECTION ( 'NONE',  ( 5.188838149069472160E-16, -1.699382548006136559E-16, -1.000000000000000000 ) ) ;
#735 = CARTESIAN_POINT ( 'NONE',  ( -5.719305292821792008, 76.92870498041706639, -1.523999999999995802 ) ) ;
#736 = CARTESIAN_POINT ( 'NONE',  ( -26.07955644221209113, 72.55303096390359485, -1.524000000000005794 ) ) ;
#737 = VECTOR ( 'NONE', #34279, 1000.000000000000000 ) ;
#738 = EDGE_CURVE ( 'NONE', #20977, #19747, #15581, .T. ) ;
#739 = CARTESIAN_POINT ( 'NONE',  ( -5.706177858098648414, 57.14999999999999147, 5.041924732081957572 ) ) ;
#740 = CARTESIAN_POINT ( 'NONE',  ( -14.50851225146815615, 78.09971119798315442, -5.392902600000144986 ) ) ;
#741 = CARTESIAN_POINT ( 'NONE',  ( -58.07447437077728125, 1.735896131820596766, 1.499107834811089557 ) ) ;
#742 = CARTESIAN_POINT ( 'NONE',  ( -58.40597088826705630, 0.2738206778524349128, 0.9753506901443759203 ) ) ;
#743 = CARTESIAN_POINT ( 'NONE',  ( -15.83110339195400051, 121.2341309109925334, 0.1099079758964732340 ) ) ;
#744 = ORIENTED_EDGE ( 'NONE', *, *, #5220, .T. ) ;
#745 = CARTESIAN_POINT ( 'NONE',  ( -57.87117896969294861, 2.397448601660856493, -0.9757051360025802422 ) ) ;
#746 = CARTESIAN_POINT ( 'NONE',  ( 6.987640295846608396, 121.9536763068500846, 0.09064736684296234581 ) ) ;
#747 = ORIENTED_EDGE ( 'NONE', *, *, #36377, .F. ) ;
#748 = FACE_OUTER_BOUND ( 'NONE', #31178, .T. ) ;
#750 = CARTESIAN_POINT ( 'NONE',  ( -9.144532176012628355, 124.1724329610943300, -0.2170005234668579974 ) ) ;
#749 = VECTOR ( 'NONE', #9550, 1000.000000000000114 ) ;
#751 = CARTESIAN_POINT ( 'NONE',  ( 6.243909332557862513, -14.15813981987112946, 1.248599486541194681 ) ) ;
#752 = CARTESIAN_POINT ( 'NONE',  ( -0.01023305610376992747, 117.8848902025789158, 0.5121039721716188486 ) ) ;
#753 = CARTESIAN_POINT ( 'NONE',  ( -3.290491044589036740, 30.52917213649525507, -3.264312889705288878 ) ) ;
#754 = CARTESIAN_POINT ( 'NONE',  ( 11.61197380483875818, 118.7506923092098674, 0.5208889651483786798 ) ) ;
#755 = CARTESIAN_POINT ( 'NONE',  ( 15.63882844255756055, 147.2230043458672242, 0.5131701251512970074 ) ) ;
#756 = CARTESIAN_POINT ( 'NONE',  ( 2.739727753987758252, 28.35525327666260864, -3.728201022356329553 ) ) ;
#757 = CARTESIAN_POINT ( 'NONE',  ( -0.5327793704965378963, 2.243135046448306191, -0.8176680881360027797 ) ) ;
#758 = CARTESIAN_POINT ( 'NONE',  ( 0.003073183581686570603, 116.5806198863164838, -0.1537946732117059789 ) ) ;
#759 = CARTESIAN_POINT ( 'NONE',  ( -30.44847906516384128, 70.61110078258337808, -1.270000000000007345 ) ) ;
#760 = CARTESIAN_POINT ( 'NONE',  ( 4.973296405157103806, 117.3984635962171126, 0.9753329598428331915 ) ) ;
#761 = CARTESIAN_POINT ( 'NONE',  ( -2.216312923931310408, 116.2476184459632691, 0.05817610133434990283 ) ) ;
#762 = CARTESIAN_POINT ( 'NONE',  ( -15.69153790699154349, 150.8349565870724120, 1.587821608835076725 ) ) ;
#763 = CARTESIAN_POINT ( 'NONE',  ( -57.81393215990352275, 0.9072688167287735750, -1.084054936344124753 ) ) ;
#764 = CARTESIAN_POINT ( 'NONE',  ( 2.782193507150679590, 158.7847427699215928, 1.504205172470084895 ) ) ;
#765 = CARTESIAN_POINT ( 'NONE',  ( 0.03245814172804981773, 158.1186941186938952, -1.624338139048501439 ) ) ;
#766 = CARTESIAN_POINT ( 'NONE',  ( 0.8497018901738310204, -5.914940278964642140, -0.4796499176142879906 ) ) ;
#767 = CARTESIAN_POINT ( 'NONE',  ( -2.957233306982606447, 159.1263692740743068, -1.212116333074086061 ) ) ;
#768 = CARTESIAN_POINT ( 'NONE',  ( 4.620269582450577062, 118.0223433806428233, -0.6741668739178967584 ) ) ;
#769 = DIRECTION ( 'NONE',  ( 0.9734199927291280474, 0.2290273297124694185, 8.537024980200812943E-16 ) ) ;
#770 = CARTESIAN_POINT ( 'NONE',  ( 8.403980202277340439, 154.6912814427390970, -0.9387012965349952331 ) ) ;
#771 = CARTESIAN_POINT ( 'NONE',  ( -2.829134042005175598, 121.0305217392013759, -0.03030232591675474305 ) ) ;
#772 = ORIENTED_EDGE ( 'NONE', *, *, #41947, .T. ) ;
#773 = CARTESIAN_POINT ( 'NONE',  ( -4.201129436297949660, 119.4047208153655646, -0.9741049750989214662 ) ) ;
#774 = CARTESIAN_POINT ( 'NONE',  ( 1.930844028328122519, -15.65960119559217745, 5.531553210582124791 ) ) ;
#775 = CARTESIAN_POINT ( 'NONE',  ( -10.39456080247343905, 81.94606122948148652, -1.523999999999999133 ) ) ;
#776 = CARTESIAN_POINT ( 'NONE',  ( -4.688800654935717738, 117.9735489986441905, -0.8264284708620113218 ) ) ;
#777 = CIRCLE ( 'NONE', #24537, 0.5079999999999997851 ) ;
#778 = CARTESIAN_POINT ( 'NONE',  ( -49.66210360255988832, 16.76989353321783227, -4.946330335750499962 ) ) ;
#779 = CARTESIAN_POINT ( 'NONE',  ( 4.065926199369043204, 118.2429491485453354, 0.3080910687088499467 ) ) ;
#780 = CARTESIAN_POINT ( 'NONE',  ( 2.417314592637331394, 119.3768144667271542, 0.7569762546260364600 ) ) ;
#781 = CARTESIAN_POINT ( 'NONE',  ( -5.878298779570172883, 78.21245918282636467, -1.269999999999996243 ) ) ;
#782 = VECTOR ( 'NONE', #16189, 1000.000000000000227 ) ;
#783 = CARTESIAN_POINT ( 'NONE',  ( 17.31377588638417819, 122.7721875394316555, 0.3459704467065360944 ) ) ;
#784 = CARTESIAN_POINT ( 'NONE',  ( 5.116497545627949783, 15.83618160547830911, 6.690270154343205711 ) ) ;
#785 = CARTESIAN_POINT ( 'NONE',  ( 10.59645057104354926, 153.0636280899912549, 0.8695332296301788721 ) ) ;
#786 = CARTESIAN_POINT ( 'NONE',  ( 22.63811803559990921, 149.3758529064199934, -0.7269731895922278975 ) ) ;
#787 = CARTESIAN_POINT ( 'NONE',  ( -44.21430376968341847, 21.24218795319825404, -2.931160726117711945 ) ) ;
#788 = ORIENTED_EDGE ( 'NONE', *, *, #21628, .T. ) ;
#789 = DIRECTION ( 'NONE',  ( 0.5149185422762221354, -0.8572391118119438991, 4.128606161907600514E-16 ) ) ;
#790 = EDGE_CURVE ( 'NONE', #20793, #10681, #4692, .T. ) ;
#791 = CARTESIAN_POINT ( 'NONE',  ( -23.35271726849064322, 148.8653451956335516, -0.3123667622787952292 ) ) ;
#792 = EDGE_LOOP ( 'NONE', ( #21978, #15513, #15968, #18508 ) ) ;
#793 = CARTESIAN_POINT ( 'NONE',  ( -5.638488239624087406, 120.9463007187987529, -0.6439909558628548192 ) ) ;
#794 = DIRECTION ( 'NONE',  ( 0.8745520943968249084, -0.4849315768086533418, 5.311926654347176508E-16 ) ) ;
#795 = CARTESIAN_POINT ( 'NONE',  ( -6.089391457280442843, 155.3491548655973133, -0.5861119247043796721 ) ) ;
#796 = CARTESIAN_POINT ( 'NONE',  ( 4.230101149094581459, -11.70512343023444402, 0.7321030916320588888 ) ) ;
#797 = CARTESIAN_POINT ( 'NONE',  ( -22.13784291382281566, 148.5290936231802448, 1.147597636374165342 ) ) ;
#798 = CARTESIAN_POINT ( 'NONE',  ( 10.92199999999999704, 56.51500000000000057, 5.016499999999999737 ) ) ;
#799 = AXIS2_PLACEMENT_3D ( 'NONE', #34127, #41784, #3016 ) ;
#800 = CARTESIAN_POINT ( 'NONE',  ( 5.779653879267166339, 116.9360814311326777, 0.1581498910197089158 ) ) ;
#801 = ORIENTED_EDGE ( 'NONE', *, *, #5335, .F. ) ;
#802 = CARTESIAN_POINT ( 'NONE',  ( -2.395914033174281865, 1.367755174955888275, -3.957843245732672877 ) ) ;
#803 = CARTESIAN_POINT ( 'NONE',  ( -16.17518884900012566, 121.2571949256804089, -0.3403554851049457319 ) ) ;
#804 = PLANE ( 'NONE',  #34407 ) ;
#805 = DIRECTION ( 'NONE',  ( 0.01997839162482749689, 1.040247600000945640E-18, -0.9998004120163610509 ) ) ;
#806 = CARTESIAN_POINT ( 'NONE',  ( -8.182749385635133876, 120.8045967382623473, 1.052528022748003167 ) ) ;
#807 = CARTESIAN_POINT ( 'NONE',  ( -4.227217475240903077, -11.31673468295422147, -1.889206449475258509 ) ) ;
#808 = CARTESIAN_POINT ( 'NONE',  ( 12.77893255256110372, 120.0678233105195716, 1.216039656670922398 ) ) ;
#809 = CARTESIAN_POINT ( 'NONE',  ( -57.60629982073510291, 1.412843483090786334, -1.546595473639808871 ) ) ;
#811 = CARTESIAN_POINT ( 'NONE',  ( 1.179722549733654091, 118.0995038195805904, -0.6028833020595596448 ) ) ;
#810 = DIRECTION ( 'NONE',  ( -0.8745520943968243532, 0.4849315768086547296, -6.829619984160642269E-16 ) ) ;
#812 = AXIS2_PLACEMENT_3D ( 'NONE', #2923, #3130, #15676 ) ;
#813 = CARTESIAN_POINT ( 'NONE',  ( -4.324967070706027705, -0.5217348546298695711, 1.653223044864502222 ) ) ;
#814 = CARTESIAN_POINT ( 'NONE',  ( -21.30289582938792847, 151.2846570542378117, -1.588627997894106247 ) ) ;
#815 = EDGE_LOOP ( 'NONE', ( #35010, #24388, #10696, #2697 ) ) ;
#816 = CARTESIAN_POINT ( 'NONE',  ( -9.242439611670359767, 123.9961275534082148, 0.1349267066575720320 ) ) ;
#817 = CARTESIAN_POINT ( 'NONE',  ( 6.086938242954471612, -13.85866328171454853, 1.967354546201298682 ) ) ;
#818 = CARTESIAN_POINT ( 'NONE',  ( 5.586884702347364673, 92.04146620154574521, 0.1116392523995368424 ) ) ;
#819 = CARTESIAN_POINT ( 'NONE',  ( -6.439703808512989190E-14, 63.33946620154573282, 4.463794035948134848E-29 ) ) ;
#820 = ORIENTED_EDGE ( 'NONE', *, *, #9466, .T. ) ;
#821 = CARTESIAN_POINT ( 'NONE',  ( 18.52749500581553477, 150.2488615152233820, 2.471439233876493446 ) ) ;
#822 = CARTESIAN_POINT ( 'NONE',  ( 4.914877656105587356, 117.6230825708500305, 0.9484198851692730026 ) ) ;
#823 = CARTESIAN_POINT ( 'NONE',  ( -46.59331663807144253, 25.66825226916589031, -1.575831774160291188 ) ) ;
#824 = VECTOR ( 'NONE', #37244, 1000.000000000000000 ) ;
#825 = TOROIDAL_SURFACE ( 'NONE', #25283, 3.683000000000000718, 0.5080000000000000071 ) ;
#826 = CARTESIAN_POINT ( 'NONE',  ( -0.007599820978812334323, 117.2191897141855179, 0.3803261187632672735 ) ) ;
#827 = CARTESIAN_POINT ( 'NONE',  ( 1.329249052905784323, 1.652534479431654546, 8.327223686629459110 ) ) ;
#828 = CARTESIAN_POINT ( 'NONE',  ( 16.04436118421907054, 148.0691544347876345, 1.589228464704729005 ) ) ;
#829 = CARTESIAN_POINT ( 'NONE',  ( -18.10310074716289819, 60.88085900918027704, 4.514343177587270439 ) ) ;
#830 = EDGE_CURVE ( 'NONE', #3380, #4530, #15208, .T. ) ;
#831 = CARTESIAN_POINT ( 'NONE',  ( 21.71781664064052464, 151.4054434770023363, -0.2817300504337350020 ) ) ;
#832 = CARTESIAN_POINT ( 'NONE',  ( 5.332935397695204749, 62.83146620154573014, 0.1065647409268304785 ) ) ;
#833 = CARTESIAN_POINT ( 'NONE',  ( -55.83462464969977646, 5.104280077925408499, 2.555929569707788396 ) ) ;
#834 = CARTESIAN_POINT ( 'NONE',  ( -49.70354115100154502, 23.42381831551578486, 0.3024929150989305038 ) ) ;
#835 = CARTESIAN_POINT ( 'NONE',  ( -4.426222872263863906, 117.3993836135536952, 1.092072450647614046 ) ) ;
#836 = CARTESIAN_POINT ( 'NONE',  ( -56.80697847991661575, 4.636179106009441497, 2.484889565616565488 ) ) ;
#837 = CARTESIAN_POINT ( 'NONE',  ( -58.62921133459555989, -0.2893463222253165879, 0.3783962402783414003 ) ) ;
#838 = ADVANCED_FACE ( 'NONE', ( #21965 ), #39369, .T. ) ;
#839 = CARTESIAN_POINT ( 'NONE',  ( -4.462445684601345164, 118.1590134028923700, 0.4283344254013793928 ) ) ;
#840 = CARTESIAN_POINT ( 'NONE',  ( 3.729890348113323650, 109.6950698699627225, -3.590377456412748636 ) ) ;
#841 = ORIENTED_EDGE ( 'NONE', *, *, #41067, .T. ) ;
#842 = CARTESIAN_POINT ( 'NONE',  ( -45.39816439898302036, 21.06106408185672763, 4.080402960186377825 ) ) ;
#843 = AXIS2_PLACEMENT_3D ( 'NONE', #9004, #2627, #21753 ) ;
#844 = CARTESIAN_POINT ( 'NONE',  ( 6.071325138224676898, 119.3725698982003394, -1.023810605546056074 ) ) ;
#845 = CARTESIAN_POINT ( 'NONE',  ( -1.375939976466558967, 106.2431249238853894, -5.170880015306797084 ) ) ;
#846 = CARTESIAN_POINT ( 'NONE',  ( 4.574376597671965250, 118.0199863044615256, 0.8705714316668682340 ) ) ;
#847 = CARTESIAN_POINT ( 'NONE',  ( -6.483461908857862888, 121.4942169270607053, -0.6390524964423260901 ) ) ;
#848 = CARTESIAN_POINT ( 'NONE',  ( -0.7503968993307388313, 115.7029095610640184, -1.755757167250588280 ) ) ;
#849 = CARTESIAN_POINT ( 'NONE',  ( 0.8116844938904650419, 118.1651004003055618, -0.8535674157383565941 ) ) ;
#850 = CARTESIAN_POINT ( 'NONE',  ( 5.793465281260485433, 118.4310156723767307, -0.4331262667984489556 ) ) ;
#851 = CARTESIAN_POINT ( 'NONE',  ( -10.28893712963056117, 123.4707319107414492, -1.320145760562476678 ) ) ;
#852 = EDGE_CURVE ( 'NONE', #35513, #25, #28474, .T. ) ;
#853 = LINE ( 'NONE', #4473, #7845 ) ;
#854 = CARTESIAN_POINT ( 'NONE',  ( -46.50210365330781315, 20.51386735866382693, 4.739171082384512346 ) ) ;
#855 = CARTESIAN_POINT ( 'NONE',  ( 8.330184522151043325, 120.0920323058251000, -1.118340454250545735 ) ) ;
#856 = CARTESIAN_POINT ( 'NONE',  ( -5.969990878950643065, 121.5454240333526599, -0.007965473844366978071 ) ) ;
#857 = CARTESIAN_POINT ( 'NONE',  ( 4.886022116125724679, 117.7561648045584519, -0.7145573245312663024 ) ) ;
#858 = CARTESIAN_POINT ( 'NONE',  ( 22.95323918608228198, 146.5883926500602001, 1.439717189780889806 ) ) ;
#859 = CARTESIAN_POINT ( 'NONE',  ( 5.965356522962838248, 88.73331249999999670, -5.016499999999999737 ) ) ;
#860 = CARTESIAN_POINT ( 'NONE',  ( 3.283982329611080608, -15.09957111342241731, 3.272784416514652239 ) ) ;
#861 = CARTESIAN_POINT ( 'NONE',  ( -12.09213366837452419, 122.8144071692085504, 1.302296015248258110 ) ) ;
#862 = CARTESIAN_POINT ( 'NONE',  ( -0.09096679801628397566, 0.3556511065658448656, 0.9697834404811940257 ) ) ;
#863 = CARTESIAN_POINT ( 'NONE',  ( -1.385657586283601583, 159.5796833544862352, -0.3718886678235073240 ) ) ;
#864 = TOROIDAL_SURFACE ( 'NONE', #11023, 0.3810000000000005604, 0.2540000000000000036 ) ;
#865 = CARTESIAN_POINT ( 'NONE',  ( 0.07244829501375356362, -8.348772924205562163, -0.9745465824848156267 ) ) ;
#866 = ORIENTED_EDGE ( 'NONE', *, *, #18744, .T. ) ;
#867 = CARTESIAN_POINT ( 'NONE',  ( -44.09535491252989203, 20.89266065238331294, 2.220044762595780874 ) ) ;
#868 = CARTESIAN_POINT ( 'NONE',  ( 2.472230802051491150, 107.2388417251876547, 4.724420784806152795 ) ) ;
#869 = CARTESIAN_POINT ( 'NONE',  ( -0.01133107913651526001, 156.3792106723807649, 0.5670535347366658652 ) ) ;
#870 = EDGE_CURVE ( 'NONE', #12283, #10681, #20973, .T. ) ;
#871 = CARTESIAN_POINT ( 'NONE',  ( 2.867264926914522949, -14.81558118910870903, 5.578245215537346979 ) ) ;
#872 = CARTESIAN_POINT ( 'NONE',  ( 17.62053193735413714, 147.9903219242534078, -1.529691019407824815 ) ) ;
#873 = CARTESIAN_POINT ( 'NONE',  ( -4.990993783036518749, 119.0545008048120366, -1.104648745759416073 ) ) ;
#874 = CARTESIAN_POINT ( 'NONE',  ( -3.831877602099685198, 71.07198261757335445, 1.270000000000004459 ) ) ;
#875 = CARTESIAN_POINT ( 'NONE',  ( 1.831848720338793202, -15.17974794010013007, 5.463771816453670382 ) ) ;
#876 = CARTESIAN_POINT ( 'NONE',  ( -4.848458278871826010, 117.4106395692391516, -1.171953005487281096 ) ) ;
#877 = EDGE_CURVE ( 'NONE', #14016, #35273, #12805, .T. ) ;
#878 = CARTESIAN_POINT ( 'NONE',  ( 6.494470876743749344, 121.7611753534313550, 0.002333837952680517004 ) ) ;
#879 = VECTOR ( 'NONE', #18768, 1000.000000000000000 ) ;
#880 = ORIENTED_EDGE ( 'NONE', *, *, #26050, .F. ) ;
#881 = CYLINDRICAL_SURFACE ( 'NONE', #38363, 0.6349999999999998979 ) ;
#882 = CARTESIAN_POINT ( 'NONE',  ( 3.744664645882537890, 109.0594030058402240, 3.805231549001048208 ) ) ;
#883 = CARTESIAN_POINT ( 'NONE',  ( 5.177913976931214357, 57.15000000000004832, 5.372099999999999653 ) ) ;
#884 = ADVANCED_FACE ( 'NONE', ( #39437, #36878 ), #33047, .F. ) ;
#885 = DIRECTION ( 'NONE',  ( -0.8745520943968241312, 0.4849315768086548406, -5.691349986800536046E-16 ) ) ;
#886 = CARTESIAN_POINT ( 'NONE',  ( 15.18069129733350309, 156.1124880001465556, 0.1695137023582059255 ) ) ;
#887 = VECTOR ( 'NONE', #18519, 1000.000000000000000 ) ;
#888 = CARTESIAN_POINT ( 'NONE',  ( 1.887249359699314732, -15.69731392916340340, 5.578901855154127176 ) ) ;
#889 = DIRECTION ( 'NONE',  ( -0.8745520943968240202, 0.4849315768086551737, -5.361993529360572958E-16 ) ) ;
#890 = CARTESIAN_POINT ( 'NONE',  ( -3.065505632821621251, 31.52364725955965952, 0.7739196574294696651 ) ) ;
#891 = CARTESIAN_POINT ( 'NONE',  ( 20.20973109032203396, 149.9354415288716780, 2.375026552130124369 ) ) ;
#892 = ORIENTED_EDGE ( 'NONE', *, *, #14638, .F. ) ;
#893 = CARTESIAN_POINT ( 'NONE',  ( 6.048790893839320226, 16.06121166075865148, 5.875566521300903844 ) ) ;
#894 = CARTESIAN_POINT ( 'NONE',  ( 5.512831477515243606, 117.4993864815744189, -0.7243090542875012527 ) ) ;
#895 = CARTESIAN_POINT ( 'NONE',  ( -2.170296427606285050, 116.5145642697238344, -1.453337335755149784 ) ) ;
#896 = CARTESIAN_POINT ( 'NONE',  ( -5.285751105923923276, 78.93631598568865115, 5.267410652559463280 ) ) ;
#897 = CARTESIAN_POINT ( 'NONE',  ( -1.761767052800523148, 106.7073752071930102, -4.966636964334769644 ) ) ;
#898 = CARTESIAN_POINT ( 'NONE',  ( -5.074705355603877699, 104.6144662015446869, 1.652004153191725999 ) ) ;
#899 = AXIS2_PLACEMENT_3D ( 'NONE', #27632, #8047, #4662 ) ;
#900 = CARTESIAN_POINT ( 'NONE',  ( 4.219463811995017188, -1.205994944679912306, -1.932895124392335573 ) ) ;
#901 = DIRECTION ( 'NONE',  ( 0.4849315768086556733, 0.8745520943968236871, -8.647447314816538780E-15 ) ) ;
#902 = DIRECTION ( 'NONE',  ( 5.188838149069472160E-16, -1.699382548006136559E-16, -1.000000000000000000 ) ) ;
#903 = CARTESIAN_POINT ( 'NONE',  ( 2.253193219399967973, -14.99063959920543532, 5.175666457621841410 ) ) ;
#904 = CARTESIAN_POINT ( 'NONE',  ( 3.676218128927467799, 120.6652674781340551, -0.2791188998294427681 ) ) ;
#905 = CARTESIAN_POINT ( 'NONE',  ( -16.51027305157944625, 155.2380866766625047, 0.5525915368032878749 ) ) ;
#906 = AXIS2_PLACEMENT_3D ( 'NONE', #17827, #7426, #24216 ) ;
#907 = CARTESIAN_POINT ( 'NONE',  ( 4.999551999793056645, 117.4036825309383119, -0.8308859279095415218 ) ) ;
#908 = LINE ( 'NONE', #14083, #2563 ) ;
#909 = VERTEX_POINT ( 'NONE', #10455 ) ;
#910 = CARTESIAN_POINT ( 'NONE',  ( -5.065021746985605589, 115.7029491485453576, 1.195979280658540755 ) ) ;
#911 = CARTESIAN_POINT ( 'NONE',  ( 4.076841989731768479, -15.73006006892005360, 3.802225825406736259 ) ) ;
#912 = CARTESIAN_POINT ( 'NONE',  ( -0.03153870137021549253, 158.4432089348667319, 1.578325583784928376 ) ) ;
#913 = CARTESIAN_POINT ( 'NONE',  ( -0.8472427164685307766, -8.777537934218566207, -4.544909406875613733 ) ) ;
#914 = EDGE_CURVE ( 'NONE', #2471, #24940, #10804, .T. ) ;
#915 = VERTEX_POINT ( 'NONE', #7696 ) ;
#916 = CARTESIAN_POINT ( 'NONE',  ( -41.23752580366542020, 23.26788267949596190, 1.269999999999994245 ) ) ;
#917 = CARTESIAN_POINT ( 'NONE',  ( 1.644890720626006386, 119.8612358676174949, 0.5912986496483325638 ) ) ;
#918 = CARTESIAN_POINT ( 'NONE',  ( -16.72891957527401630, 148.5304741467402323, 1.365449702224204032 ) ) ;
#919 = CARTESIAN_POINT ( 'NONE',  ( -47.73411474416273137, 19.53609852428665050, 5.217284324673509666 ) ) ;
#920 = ADVANCED_FACE ( 'NONE', ( #1310 ), #35822, .T. ) ;
#921 = CARTESIAN_POINT ( 'NONE',  ( 11.41525058642613288, 122.8492764348241337, -1.228842657910305780 ) ) ;
#922 = AXIS2_PLACEMENT_3D ( 'NONE', #6804, #22543, #10198 ) ;
#923 = CARTESIAN_POINT ( 'NONE',  ( -2.647237659633569606, 158.4754809254847601, -1.642537635467619772 ) ) ;
#924 = CARTESIAN_POINT ( 'NONE',  ( -6.136538366514222075E-14, 101.1854662015457365, 9.995674010754261804E-17 ) ) ;
#925 = CIRCLE ( 'NONE', #13125, 0.2540000000000011693 ) ;
#926 = VERTEX_POINT ( 'NONE', #17468 ) ;
#927 = CARTESIAN_POINT ( 'NONE',  ( 4.387465901250098277, 118.1845649924603379, -0.4239173906933821345 ) ) ;
#928 = CARTESIAN_POINT ( 'NONE',  ( 15.85992372348528434, 147.2950763206921181, -0.4080883723285143594 ) ) ;
#929 = VERTEX_POINT ( 'NONE', #20445 ) ;
#930 = CARTESIAN_POINT ( 'NONE',  ( 3.239928030326187258, -14.81799142783181367, -0.3301716407829758948 ) ) ;
#931 = EDGE_CURVE ( 'NONE', #32109, #25746, #26433, .T. ) ;
#932 = CARTESIAN_POINT ( 'NONE',  ( 11.11710224467026542, 56.30409367656755393, -5.016499999999892268 ) ) ;
#933 = AXIS2_PLACEMENT_3D ( 'NONE', #16577, #26595, #39603 ) ;
#934 = ADVANCED_FACE ( 'NONE', ( #10661 ), #17435, .T. ) ;
#935 = CARTESIAN_POINT ( 'NONE',  ( -49.23283723365464937, 17.42967204962415195, 5.014312523175059155 ) ) ;
#936 = CARTESIAN_POINT ( 'NONE',  ( 3.235533175430977515, 2.501875212487111977, 3.308963532380430284 ) ) ;
#937 = CARTESIAN_POINT ( 'NONE',  ( 12.21508602987348269, 126.0625018263836807, 1.612267168929819583 ) ) ;
#938 = CARTESIAN_POINT ( 'NONE',  ( 2.151558901213805886, 36.10138897990322704, -0.07425415374395130663 ) ) ;
#939 = CARTESIAN_POINT ( 'NONE',  ( -4.319812470756069445, 11.96289413176387129, -1.686699837767231536 ) ) ;
#940 = CARTESIAN_POINT ( 'NONE',  ( 15.64085066085077536, 147.2198192248932571, 0.3637928714071058667 ) ) ;
#941 = DIRECTION ( 'NONE',  ( -0.7071067811865480168, -0.7071067811865470176, 8.659560562354937789E-17 ) ) ;
#942 = CARTESIAN_POINT ( 'NONE',  ( -56.37071950982826252, 3.976973756211601874, -2.203872415222129177 ) ) ;
#943 = CARTESIAN_POINT ( 'NONE',  ( 8.796184242131879216, 117.7096009060177266, 0.009943947433590954663 ) ) ;
#944 = CARTESIAN_POINT ( 'NONE',  ( 16.86202032626302483, 155.2029898760372646, 0.3369432954968345495 ) ) ;
#945 = AXIS2_PLACEMENT_3D ( 'NONE', #37814, #8640, #17790 ) ;
#946 = DIRECTION ( 'NONE',  ( -0.8745520943968240202, 0.4849315768086553402, -5.361993529360572958E-16 ) ) ;
#947 = CARTESIAN_POINT ( 'NONE',  ( -25.81615557310160014, 74.46796499802707103, -1.524000000000005794 ) ) ;
#948 = CARTESIAN_POINT ( 'NONE',  ( -29.67105550542181547, 68.29201113455899019, -1.270000000000484519 ) ) ;
#949 = CARTESIAN_POINT ( 'NONE',  ( 0.1224881284885083327, 5.266211660758980173, 8.431793989537572642 ) ) ;
#950 = CARTESIAN_POINT ( 'NONE',  ( -4.965996940879724875, 56.51500000000000767, 4.710730864944216556 ) ) ;
#951 = FACE_OUTER_BOUND ( 'NONE', #38983, .T. ) ;
#952 = CARTESIAN_POINT ( 'NONE',  ( -58.33777482027512207, 1.113448835244237767, 1.208045587469420701 ) ) ;
#953 = CARTESIAN_POINT ( 'NONE',  ( 0.02135216056118049294, 118.1497763966934258, -1.068549427312639910 ) ) ;
#954 = CARTESIAN_POINT ( 'NONE',  ( -15.62286502883001837, 121.0226940419799462, 0.1111101786179100326 ) ) ;
#955 = ORIENTED_EDGE ( 'NONE', *, *, #9252, .T. ) ;
#956 = CARTESIAN_POINT ( 'NONE',  ( -57.93941708942283952, 2.052042089854988483, -1.628789306319528896 ) ) ;
#957 = CARTESIAN_POINT ( 'NONE',  ( 6.073369455593417676, 121.4395935480491318, 0.1192957112538572118 ) ) ;
#958 = EDGE_LOOP ( 'NONE', ( #31328, #8348, #40597, #40431 ) ) ;
#959 = CARTESIAN_POINT ( 'NONE',  ( -17.14500000000466784, 71.11999999999886768, -1.524000000000000909 ) ) ;
#960 = CARTESIAN_POINT ( 'NONE',  ( -15.72281364106782675, 146.8976350983841144, -0.3655119725415948984 ) ) ;
#961 = CARTESIAN_POINT ( 'NONE',  ( 2.468517452056580463, -15.43523125850157562, 5.870468177969554446 ) ) ;
#962 = CARTESIAN_POINT ( 'NONE',  ( -21.01144550848356829, 149.0309112320384486, 1.514039682450821545 ) ) ;
#963 = CARTESIAN_POINT ( 'NONE',  ( -2.201963191602333225, 30.07953629247752758, -4.075912811544394998 ) ) ;
#964 = CARTESIAN_POINT ( 'NONE',  ( -0.004910662370487759928, 159.5928157220454295, 0.2457496255665023166 ) ) ;
#965 = CARTESIAN_POINT ( 'NONE',  ( 2.076497001697454436, -15.66584657922642876, 5.557590741999150374 ) ) ;
#966 = CARTESIAN_POINT ( 'NONE',  ( 0.2838385327444274964, 29.22985346960623332, -4.617364983570896086 ) ) ;
#967 = CARTESIAN_POINT ( 'NONE',  ( 0.9769954323678800012, -0.8923827921977626199, -0.09387087892739469364 ) ) ;
#968 = CARTESIAN_POINT ( 'NONE',  ( -2.778732907383235862, 116.5968896900294709, -0.2040764120049695651 ) ) ;
#969 = LINE ( 'NONE', #13938, #25666 ) ;
#970 = DIRECTION ( 'NONE',  ( -0.8138664877804109299, 0.5810519254489895369, 0.000000000000000000 ) ) ;
#971 = ORIENTED_EDGE ( 'NONE', *, *, #2183, .F. ) ;
#972 = CARTESIAN_POINT ( 'NONE',  ( 5.531187961632795691, 116.9767413707218253, 0.6070940273833828060 ) ) ;
#973 = CARTESIAN_POINT ( 'NONE',  ( -17.67426794430100401, 144.4767212251450417, 1.594784396078125388 ) ) ;
#974 = CARTESIAN_POINT ( 'NONE',  ( -57.67508898341257151, 1.207211884619313835, -1.229746519219142353 ) ) ;
#975 = CARTESIAN_POINT ( 'NONE',  ( 21.00644369030274206, 149.3892802667211868, 2.301546136566545275 ) ) ;
#976 = CARTESIAN_POINT ( 'NONE',  ( 19.35587726549907117, 148.6897983921382433, -1.735459330159158986 ) ) ;
#977 = VECTOR ( 'NONE', #10715, 1000.000000000000114 ) ;
#978 = CIRCLE ( 'NONE', #24748, 0.7620000000000000107 ) ;
#979 = CARTESIAN_POINT ( 'NONE',  ( -0.8109939492151988505, -12.39128985057688936, -0.5387275711561630986 ) ) ;
#980 = CARTESIAN_POINT ( 'NONE',  ( -2.096789228656116499, 117.6567184779878232, -0.6641637518095836468 ) ) ;
#981 = CARTESIAN_POINT ( 'NONE',  ( -44.36446822842629700, 21.81554158013422651, -2.896954608336749892 ) ) ;
#982 = CARTESIAN_POINT ( 'NONE',  ( 4.307776028491197451, 105.1217194734575884, 3.166495586438745846 ) ) ;
#983 = CARTESIAN_POINT ( 'NONE',  ( 4.675694769581089538, 155.9604050671876792, -0.8934998238159542749 ) ) ;
#984 = CARTESIAN_POINT ( 'NONE',  ( 7.826010746941338247, 122.3856571825914159, 0.6413869067663138246 ) ) ;
#985 = ORIENTED_EDGE ( 'NONE', *, *, #37802, .F. ) ;
#986 = CARTESIAN_POINT ( 'NONE',  ( 0.01051219832176353980, 119.4384375980492194, -0.5260733902271048645 ) ) ;
#987 = CARTESIAN_POINT ( 'NONE',  ( 4.176612884749554944, -15.71584146423912820, 3.621469129306375656 ) ) ;
#988 = CIRCLE ( 'NONE', #32252, 0.5080000000000000071 ) ;
#989 = CARTESIAN_POINT ( 'NONE',  ( -58.82991074935231524, -0.2577531494038359794, -1.058401375502683064E-14 ) ) ;
#990 = CARTESIAN_POINT ( 'NONE',  ( -4.596683656305176058, 118.0615522034898106, -0.7278660542837124270 ) ) ;
#991 = EDGE_CURVE ( 'NONE', #15388, #35792, #6846, .T. ) ;
#992 = CARTESIAN_POINT ( 'NONE',  ( -53.75224695799815322, 9.373383622779334345, -3.688627211158436392 ) ) ;
#993 = DIRECTION ( 'NONE',  ( -0.8745520943968245753, 0.4849315768086539524, -5.691349986800526185E-16 ) ) ;
#994 = CARTESIAN_POINT ( 'NONE',  ( 14.20821676177088300, 128.5469532985352714, 2.008711173933039440 ) ) ;
#995 = CARTESIAN_POINT ( 'NONE',  ( -14.42383115828894624, 69.61113539875873357, 1.270000000000000018 ) ) ;
#996 = CARTESIAN_POINT ( 'NONE',  ( 2.732111087507031133, 116.5293111276780849, 0.05459408159141365680 ) ) ;
#997 = CARTESIAN_POINT ( 'NONE',  ( 5.579263951540290201, 8.940976842658965751, -6.340258638080404019 ) ) ;
#998 = CARTESIAN_POINT ( 'NONE',  ( -0.008148072696649801341, 156.3406798448389168, 0.4077628766201955579 ) ) ;
#999 = CARTESIAN_POINT ( 'NONE',  ( 0.3623072504455067122, 117.0882377308211773, -0.3576919811193869370 ) ) ;
#1000 = CARTESIAN_POINT ( 'NONE',  ( -9.712308604790299782, 65.53852105402241079, -1.523999999999996025 ) ) ;
#1001 = FACE_OUTER_BOUND ( 'NONE', #21889, .T. ) ;
#1002 = CARTESIAN_POINT ( 'NONE',  ( -22.53566265713742567, 150.7862151120626777, -0.3736683405004930791 ) ) ;
#1003 = VERTEX_POINT ( 'NONE', #3662 ) ;
#1004 = CARTESIAN_POINT ( 'NONE',  ( -47.04217617083259029, 23.73857702128102076, -2.948847133965297740 ) ) ;
#1005 = CARTESIAN_POINT ( 'NONE',  ( 5.747156222950085436, 121.0755541023018935, -0.3521415724599298858 ) ) ;
#1006 = FACE_OUTER_BOUND ( 'NONE', #25111, .T. ) ;
#1007 = VERTEX_POINT ( 'NONE', #36453 ) ;
#1008 = CYLINDRICAL_SURFACE ( 'NONE', #1562, 0.2539999999999931202 ) ;
#1009 = CARTESIAN_POINT ( 'NONE',  ( -0.6211475606396847926, 120.8480686026657196, -0.1701230225530362405 ) ) ;
#1010 = CARTESIAN_POINT ( 'NONE',  ( 2.417269819423324861, -15.13903239461346395, 5.861448462117607505 ) ) ;
#1011 = CARTESIAN_POINT ( 'NONE',  ( -12.65084386183224829, 120.1953580586475567, 0.8051295378619942600 ) ) ;
#1012 = CARTESIAN_POINT ( 'NONE',  ( -0.6412933796113865492, 156.3034662015457741, -0.01281456791805603290 ) ) ;
#1013 = CARTESIAN_POINT ( 'NONE',  ( 11.72380150228539186, 118.7251779360019270, 0.2815772452395035597 ) ) ;
#1014 = ORIENTED_EDGE ( 'NONE', *, *, #34488, .F. ) ;
#1015 = CARTESIAN_POINT ( 'NONE',  ( 4.634220987317881679, -1.855718946426311078, -0.01876340930339078644 ) ) ;
#1016 = CARTESIAN_POINT ( 'NONE',  ( -23.21309708346267797, 149.6303025714371131, -0.4895544115752260561 ) ) ;
#1017 = CARTESIAN_POINT ( 'NONE',  ( 6.059261036833978764, 78.87450423423040036, 5.016499999999999737 ) ) ;
#1018 = CARTESIAN_POINT ( 'NONE',  ( 5.078986093043052819, 100.6774662015457409, 0.1014902294541237954 ) ) ;
#1019 = ORIENTED_EDGE ( 'NONE', *, *, #19182, .T. ) ;
#1020 = CARTESIAN_POINT ( 'NONE',  ( -6.355526478890559439, 119.3884140220176988, 1.006251212807348416 ) ) ;
#1021 = CARTESIAN_POINT ( 'NONE',  ( 2.099109474952898236, -4.195072059908932616, -4.137704358558784712 ) ) ;
#1022 = CARTESIAN_POINT ( 'NONE',  ( 3.017629403178959446, 159.2229145144301867, 1.079859862993577613 ) ) ;
#1023 = CARTESIAN_POINT ( 'NONE',  ( -57.89036626108683237, 0.7933261799619758525, -1.256022413937835092 ) ) ;
#1025 = CARTESIAN_POINT ( 'NONE',  ( 20.46179744412665613, 141.4490678312372722, -1.579512522682919418 ) ) ;
#1024 = CARTESIAN_POINT ( 'NONE',  ( -5.078986093043186933, 101.1854662015457365, -0.1014902294541231709 ) ) ;
#1026 = CARTESIAN_POINT ( 'NONE',  ( -3.769861741716944881, -2.021032284792064093, -2.673854242032364326 ) ) ;
#1027 = CARTESIAN_POINT ( 'NONE',  ( -17.57666534335618636, 125.1652531886817172, -1.391946913312247958 ) ) ;
#1028 = ORIENTED_EDGE ( 'NONE', *, *, #29131, .F. ) ;
#1029 = ORIENTED_EDGE ( 'NONE', *, *, #32030, .T. ) ;
#1030 = CARTESIAN_POINT ( 'NONE',  ( -9.057492758458371540, 123.9289873439938674, -0.02221773104347207761 ) ) ;
#1031 = CARTESIAN_POINT ( 'NONE',  ( 5.498302128480847983, -14.40662979408034694, 3.384674516772870234 ) ) ;
#1032 = DIRECTION ( 'NONE',  ( 4.017660918040594346E-17, -1.000000000000000000, -2.376309959284834438E-19 ) ) ;
#1033 = CARTESIAN_POINT ( 'NONE',  ( -3.798767985847472328, 109.6290767857702235, -3.753213138019654505 ) ) ;
#1034 = ORIENTED_EDGE ( 'NONE', *, *, #302, .F. ) ;
#1035 = CARTESIAN_POINT ( 'NONE',  ( 19.28990034181448010, 145.1342744731992127, 2.527759927608660639 ) ) ;
#1036 = CARTESIAN_POINT ( 'NONE',  ( 4.864735862609903982, 117.7358714380141151, 0.9167521008204471133 ) ) ;
#1037 = CARTESIAN_POINT ( 'NONE',  ( -18.58115504727956591, 80.30342350548193053, -1.524000000000003130 ) ) ;
#1038 = CARTESIAN_POINT ( 'NONE',  ( -0.3722574617743142356, 117.2097358735305050, 0.3924287308447402256 ) ) ;
#1039 = CARTESIAN_POINT ( 'NONE',  ( 6.828157356468467221, 12.44753447943134184, 4.948315318077098901 ) ) ;
#1040 = CARTESIAN_POINT ( 'NONE',  ( 5.158718007120178584, 120.8264575521020987, 0.6815868816981847100 ) ) ;
#1041 = CARTESIAN_POINT ( 'NONE',  ( -23.21760062652228385, 78.26400813401573942, -1.270000000000005125 ) ) ;
#1042 = COLOUR_RGB ( '', 0.08235294, 0.09019608, 0.10196078) ;
#1043 = CARTESIAN_POINT ( 'NONE',  ( 15.19762206999197396, 120.8830733721255370, -0.2994679608661979797 ) ) ;
#1044 = CARTESIAN_POINT ( 'NONE',  ( 4.858589416345391321, 117.7980557432572795, -0.7304706717345029743 ) ) ;
#1045 = CARTESIAN_POINT ( 'NONE',  ( -57.39381155807401313, 1.812545739600947892, 1.491594637569517712 ) ) ;
#1046 = CARTESIAN_POINT ( 'NONE',  ( -50.64083584635693569, 22.17031203569813513, -9.591688330814065574E-15 ) ) ;
#1047 = CARTESIAN_POINT ( 'NONE',  ( -4.019356026430203066, 117.3993838141520172, 1.158635538540764731 ) ) ;
#1048 = CARTESIAN_POINT ( 'NONE',  ( -49.01671973967521012, 18.67808020721676954, 5.174630477995038724 ) ) ;
#1049 = CARTESIAN_POINT ( 'NONE',  ( -58.60011173050265398, -0.2330837761818443932, 0.4599256431870107908 ) ) ;
#1050 = CARTESIAN_POINT ( 'NONE',  ( -4.529539828068924301, 118.1222249965676383, 0.4827831673290448600 ) ) ;
#1051 = DIRECTION ( 'NONE',  ( 0.9998004120163608288, -1.039227405372660929E-20, 0.01997839162482763914 ) ) ;
#1052 = ORIENTED_EDGE ( 'NONE', *, *, #4297, .T. ) ;
#1053 = CARTESIAN_POINT ( 'NONE',  ( -44.90991502375803890, 23.16658271142636139, 2.247441098035892981 ) ) ;
#1054 = CARTESIAN_POINT ( 'NONE',  ( 6.127741334488804092, 119.4943318094760372, -1.015363485661166854 ) ) ;
#1055 = CARTESIAN_POINT ( 'NONE',  ( -7.136594729663847225, 122.4194348751405101, -0.2521576392032935376 ) ) ;
#1056 = CARTESIAN_POINT ( 'NONE',  ( 4.486670294817050930, 118.0822176383332902, 0.8003028680957253727 ) ) ;
#1057 = CARTESIAN_POINT ( 'NONE',  ( -13.61103386154299599, 134.2686865373913463, -1.213594671188916729 ) ) ;
#1058 = CARTESIAN_POINT ( 'NONE',  ( -1.071200444556306364, 115.7029399934560701, -1.745870039784299443 ) ) ;
#1059 = DIRECTION ( 'NONE',  ( 0.9998004120163608288, 0.000000000000000000, 0.01997839162482736852 ) ) ;
#1060 = CARTESIAN_POINT ( 'NONE',  ( 2.686051902181449513, 107.2142675576569530, -4.629644704627760454 ) ) ;
#1061 = CARTESIAN_POINT ( 'NONE',  ( -6.507413728078120130, 121.1369950346570192, -0.8796459533030991373 ) ) ;
#1062 = DIRECTION ( 'NONE',  ( -0.8745520943968367877, 0.4849315768086320255, -4.268512490100441970E-16 ) ) ;
#1063 = CARTESIAN_POINT ( 'NONE',  ( 8.020178813429859943, 121.5755450013093366, -0.8283951592328165914 ) ) ;
#1064 = CARTESIAN_POINT ( 'NONE',  ( -6.997652640569123506, 121.9526520484695027, -0.1398297549648395144 ) ) ;
#1065 = DIRECTION ( 'NONE',  ( 0.8745520943968253524, -0.4849315768086530087, 8.537024980200771528E-16 ) ) ;
#1066 = CARTESIAN_POINT ( 'NONE',  ( -0.009748065369249667503, 159.5507987164374981, 0.4878330526048098581 ) ) ;
#1067 = CARTESIAN_POINT ( 'NONE',  ( 5.475330206976798841, 65.30181249999998272, -5.107412922131463695 ) ) ;
#1068 = CARTESIAN_POINT ( 'NONE',  ( 3.043194142253923928, -14.61827878651010515, -0.2680077959190000358 ) ) ;
#1069 = CARTESIAN_POINT ( 'NONE',  ( -15.78846850359705556, 131.3838724160208926, 1.599517327752104423 ) ) ;
#1070 = CARTESIAN_POINT ( 'NONE',  ( -0.3571511390000196573, -0.07365323586406080647, 0.9071407500242820721 ) ) ;
#1071 = CARTESIAN_POINT ( 'NONE',  ( -23.02941925350885555, 142.5499849734818838, -1.196609915892170584 ) ) ;
#1072 = CARTESIAN_POINT ( 'NONE',  ( -0.03357488772870852872, 24.54038786010652728, -0.9749811203568246043 ) ) ;
#1073 = VERTEX_POINT ( 'NONE', #29634 ) ;
#1074 = CARTESIAN_POINT ( 'NONE',  ( -49.14072577824710208, 13.89916973120787524, 0.4067138869237276744 ) ) ;
#1075 = CARTESIAN_POINT ( 'NONE',  ( 5.888892352462119284, 118.9932487913337411, 0.5850130909721118488 ) ) ;
#1076 = AXIS2_PLACEMENT_3D ( 'NONE', #34899, #5731, #18684 ) ;
#1077 = CARTESIAN_POINT ( 'NONE',  ( -15.94526953466043118, 147.3275361421020193, 0.5311500221062651628 ) ) ;
#1078 = CARTESIAN_POINT ( 'NONE',  ( 4.035643413487081332, -14.09208526182970189, 4.581805149448960002 ) ) ;
#1079 = CARTESIAN_POINT ( 'NONE',  ( 2.533752743581966005, 119.8406177399916714, -0.5716348071481810456 ) ) ;
#1080 = EDGE_LOOP ( 'NONE', ( #11911, #34503, #25339, #40906 ) ) ;
#1081 = CARTESIAN_POINT ( 'NONE',  ( -7.606098120227111181, 119.7866739149480253, -1.386975461113101549 ) ) ;
#1082 = CARTESIAN_POINT ( 'NONE',  ( 3.658123981884035647, 115.7029863172577535, 1.617079049715255845 ) ) ;
#1083 = EDGE_CURVE ( 'NONE', #35234, #17174, #37846, .T. ) ;
#1084 = CARTESIAN_POINT ( 'NONE',  ( 2.906309357581933650, -13.72804873580029472, 0.7610837935892840189 ) ) ;
#1085 = CARTESIAN_POINT ( 'NONE',  ( -29.82321757229076908, 71.17901112636586447, -1.524000000000007349 ) ) ;
#1086 = EDGE_CURVE ( 'NONE', #24253, #32761, #16627, .T. ) ;
#1087 = CARTESIAN_POINT ( 'NONE',  ( 4.566879893416641245, 121.1702857069421100, -0.02052890071062566171 ) ) ;
#1088 = VERTEX_POINT ( 'NONE', #7273 ) ;
#1089 = CYLINDRICAL_SURFACE ( 'NONE', #27471, 14.73199999999999577 ) ;
#1090 = CARTESIAN_POINT ( 'NONE',  ( 2.611213466451486109, 107.7056043231343665, 4.533743039264392927 ) ) ;
#1091 = DIRECTION ( 'NONE',  ( 1.011795553208986377E-16, 1.000000000000000000, -0.000000000000000000 ) ) ;
#1092 = CARTESIAN_POINT ( 'NONE',  ( -8.761523658392189162, 74.56051954986229191, 1.270000000000002016 ) ) ;
#1093 = CARTESIAN_POINT ( 'NONE',  ( 13.40764007945148428, 156.9487217736090940, 0.07645926402191062510 ) ) ;
#1094 = CARTESIAN_POINT ( 'NONE',  ( -5.517349593794012463, 28.10803576007639393, 0.4164286583522215368 ) ) ;
#1095 = CARTESIAN_POINT ( 'NONE',  ( 2.006295418716820933, -15.63691049494941865, 5.487271958674783789 ) ) ;
#1096 = CARTESIAN_POINT ( 'NONE',  ( -6.654617103318593247E-14, 104.6144662015457243, 1.534725424433578570E-31 ) ) ;
#1097 = CARTESIAN_POINT ( 'NONE',  ( -3.046231754824816118, 31.09810386281187533, 0.4001267285823233433 ) ) ;
#1098 = CARTESIAN_POINT ( 'NONE',  ( 2.647237659633441265, 158.4754809254847601, 1.642537635467619994 ) ) ;
#1099 = VECTOR ( 'NONE', #37403, 1000.000000000000000 ) ;
#1100 = VERTEX_POINT ( 'NONE', #33261 ) ;
#1101 = CARTESIAN_POINT ( 'NONE',  ( -0.5381045032992836097, 19.73597684265961050, -8.428375251626778919 ) ) ;
#1102 = CARTESIAN_POINT ( 'NONE',  ( -8.658272382007252688, 118.2880589149417148, -0.9754036577767483118 ) ) ;
#1103 = CARTESIAN_POINT ( 'NONE',  ( -5.810938089476440638, 124.3836500214474654, -0.1311214433933293733 ) ) ;
#1104 = CARTESIAN_POINT ( 'NONE',  ( 4.784097136343040013, 117.4060489132068597, 1.200267903224836896 ) ) ;
#1105 = CARTESIAN_POINT ( 'NONE',  ( -29.81357423954495189, 70.62209452652477637, 1.269999999999992690 ) ) ;
#1106 = CARTESIAN_POINT ( 'NONE',  ( -0.001261869788248145890, 124.3520329708341876, 0.06314912420803926729 ) ) ;
#1107 = CARTESIAN_POINT ( 'NONE',  ( 4.586363120317823672, -1.655842793181455663, -0.6244342276643227718 ) ) ;
#1108 = DIRECTION ( 'NONE',  ( -0.9876665170007972172, 0.1565721916417913695, -1.707025578116413603E-15 ) ) ;
#1109 = CARTESIAN_POINT ( 'NONE',  ( -5.153324091253895567, 56.51694919289731445, -4.640537933314518249 ) ) ;
#1110 = CARTESIAN_POINT ( 'NONE',  ( 3.240066224740343781, -14.18897675264189928, 3.749338592554243288 ) ) ;
#1111 = ADVANCED_FACE ( 'NONE', ( #472 ), #30359, .T. ) ;
#1112 = CARTESIAN_POINT ( 'NONE',  ( 4.981054720647222211, 121.2162878128435892, -0.1538846217318251552 ) ) ;
#1113 = CARTESIAN_POINT ( 'NONE',  ( -16.46484310285447350, 122.7513851185756693, 0.4780162726406277929 ) ) ;
#1114 = CARTESIAN_POINT ( 'NONE',  ( 2.411581292501531415, 38.13423181323310729, 1.422810646954211666 ) ) ;
#1115 = PLANE ( 'NONE',  #36582 ) ;
#1116 = VERTEX_POINT ( 'NONE', #13445 ) ;
#1117 = CARTESIAN_POINT ( 'NONE',  ( -5.314273266013044505, 104.6144662015457527, 0.4583182832411464291 ) ) ;
#1118 = CARTESIAN_POINT ( 'NONE',  ( 4.698461193529555935, -15.58032547337365159, 2.177983573914926030 ) ) ;
#1119 = CARTESIAN_POINT ( 'NONE',  ( -8.792132358471173248, 156.9002828235886966, 1.708777300431143731 ) ) ;
#1120 = CARTESIAN_POINT ( 'NONE',  ( 0.09481320634720795393, -4.229605868409334057, 4.636458411128852930 ) ) ;
#1121 = EDGE_LOOP ( 'NONE', ( #34298, #24074 ) ) ;
#1122 = FACE_OUTER_BOUND ( 'NONE', #9226, .T. ) ;
#1123 = CARTESIAN_POINT ( 'NONE',  ( 0.3260985403865587773, 116.4813942609866899, 1.528836360202051381 ) ) ;
#1124 = DIRECTION ( 'NONE',  ( 0.000000000000000000, 0.000000000000000000, 1.000000000000000000 ) ) ;
#1125 = PRODUCT ( 'Base Ring', 'Base Ring', '', ( #16178 ) ) ;
#1126 = CARTESIAN_POINT ( 'NONE',  ( -10.51090385015224804, 123.6668265419868646, 0.9186085726806039187 ) ) ;
#1127 = CARTESIAN_POINT ( 'NONE',  ( 4.610436209567292387, 117.9340757871244847, 0.9619774773656434297 ) ) ;
#1128 = CARTESIAN_POINT ( 'NONE',  ( 10.01831529487285266, 155.4362223408194836, -1.706801840347523136 ) ) ;
#1129 = CARTESIAN_POINT ( 'NONE',  ( -18.06424110348786982, 131.7244750738095149, -2.230326231357608879 ) ) ;
#1130 = FACE_OUTER_BOUND ( 'NONE', #36755, .T. ) ;
#1131 = CIRCLE ( 'NONE', #24910, 0.5080000000000002292 ) ;
#1132 = ADVANCED_FACE ( 'NONE', ( #40076 ), #32397, .T. ) ;
#1133 = CARTESIAN_POINT ( 'NONE',  ( 4.292225393060463468, 118.2141433220078568, -0.3520200080934876019 ) ) ;
#1134 = CARTESIAN_POINT ( 'NONE',  ( 10.62272853480718204, 153.0636280899912549, -0.4455235322555908817 ) ) ;
#1135 = VECTOR ( 'NONE', #1960, 1000.000000000000114 ) ;
#1136 = ORIENTED_EDGE ( 'NONE', *, *, #610, .T. ) ;
#1137 = AXIS2_PLACEMENT_3D ( 'NONE', #21480, #17672, #24694 ) ;
#1138 = CARTESIAN_POINT ( 'NONE',  ( 3.189131052002434963, -14.84934909478852205, 3.295817422932660890 ) ) ;
#1139 = CARTESIAN_POINT ( 'NONE',  ( -49.99157512321825436, 16.20856241626540850, 4.827055480670583876 ) ) ;
#1140 = EDGE_CURVE ( 'NONE', #26949, #14480, #27277, .T. ) ;
#1141 = CARTESIAN_POINT ( 'NONE',  ( -4.422273941422524501, 8.986318502778324557, 1.404945367500548548 ) ) ;
#1142 = CARTESIAN_POINT ( 'NONE',  ( 16.09426298050571802, 139.8573806175465961, 2.037321532313223660 ) ) ;
#1143 = CARTESIAN_POINT ( 'NONE',  ( -2.585859724564241180, 30.03814370764511565, 1.303285975734316926 ) ) ;
#1144 = CARTESIAN_POINT ( 'NONE',  ( -4.544942180623752215, 12.81246518813932589, 0.8472608254572608910 ) ) ;
#1145 = CARTESIAN_POINT ( 'NONE',  ( 10.21163942101050459, 125.9885856776569426, 0.2414886939513459507 ) ) ;
#1146 = CARTESIAN_POINT ( 'NONE',  ( -23.69188486464780752, 78.08202335040543574, 1.523999999999994026 ) ) ;
#1147 = EDGE_CURVE ( 'NONE', #25488, #14172, #10631, .T. ) ;
#1148 = CARTESIAN_POINT ( 'NONE',  ( -56.40799993875704388, 3.472264316502340797, -0.7602746155037358733 ) ) ;
#1149 = CARTESIAN_POINT ( 'NONE',  ( -8.786561437352411019, 117.7207579526419607, -0.3770129002165002463 ) ) ;
#1150 = AXIS2_PLACEMENT_3D ( 'NONE', #33200, #33825, #37022 ) ;
#1151 = CARTESIAN_POINT ( 'NONE',  ( 0.001261869788231272235, 124.3520329708341876, -0.06314912420803690807 ) ) ;
#1152 = FACE_OUTER_BOUND ( 'NONE', #15557, .T. ) ;
#1153 = CARTESIAN_POINT ( 'NONE',  ( -0.4039975341914995299, 105.7852372210178942, 5.327039100247182191 ) ) ;
#1154 = CARTESIAN_POINT ( 'NONE',  ( -33.42971872652992005, 49.93539301574497102, -1.524000000000002020 ) ) ;
#1155 = CARTESIAN_POINT ( 'NONE',  ( -3.946719713907086202, 4.502433826932805694, 7.497755479828382086 ) ) ;
#1156 = CARTESIAN_POINT ( 'NONE',  ( 5.293178828769798727, 115.7029491485453150, 0.7217268129011673583 ) ) ;
#1157 = LINE ( 'NONE', #36934, #4914 ) ;
#1158 = CARTESIAN_POINT ( 'NONE',  ( -58.83227707057483968, -0.08366279997992775996, 0.2458995907044888019 ) ) ;
#1159 = CARTESIAN_POINT ( 'NONE',  ( 0.06282972276035359016, 111.5577547982949227, -3.144256248693377387 ) ) ;
#1160 = CARTESIAN_POINT ( 'NONE',  ( -0.9434990333793340511, 116.6346273530297850, 0.1892539897508100366 ) ) ;
#1161 = VECTOR ( 'NONE', #11393, 1000.000000000000000 ) ;
#1162 = EDGE_LOOP ( 'NONE', ( #510, #2964, #28536, #33915 ) ) ;
#1163 = CARTESIAN_POINT ( 'NONE',  ( -56.90265763162630464, 5.074588416753345044, -1.064700026618667916 ) ) ;
#1164 = CARTESIAN_POINT ( 'NONE',  ( -17.14500000000466784, 71.11999999999886768, 1.269999999999998241 ) ) ;
#1165 = ADVANCED_FACE ( 'NONE', ( #20864 ), #5547, .T. ) ;
#1166 = ORIENTED_EDGE ( 'NONE', *, *, #32177, .F. ) ;
#1167 = CARTESIAN_POINT ( 'NONE',  ( -0.6407465451154844560, 156.3034662015456888, -0.04018040219424089815 ) ) ;
#1168 = CARTESIAN_POINT ( 'NONE',  ( 2.663097075550662662, -15.49037753074605739, 5.782289944512356783 ) ) ;
#1169 = CARTESIAN_POINT ( 'NONE',  ( -15.01775385910461935, 123.1914926142276130, 1.125269324988862119 ) ) ;
#1170 = CARTESIAN_POINT ( 'NONE',  ( -0.003746264460362601790, 116.6481217037470373, 0.1874783927187337884 ) ) ;
#1171 = ADVANCED_FACE ( 'NONE', ( #21692 ), #34448, .T. ) ;
#1172 = CARTESIAN_POINT ( 'NONE',  ( 9.009615515465577928, 124.1466948585039489, 0.3142177148139755349 ) ) ;
#1173 = CARTESIAN_POINT ( 'NONE',  ( -2.201963191602333225, 30.07953629247752758, -4.075912811544394998 ) ) ;
#1174 = CARTESIAN_POINT ( 'NONE',  ( -0.8573366540693068139, -6.603747334586292261, -0.4721712316449505620 ) ) ;
#1175 = CARTESIAN_POINT ( 'NONE',  ( -16.12231377365586127, 121.3783152868344075, -0.5570369914769760511 ) ) ;
#1176 = CARTESIAN_POINT ( 'NONE',  ( -4.856487665647835961, 117.8020098535915565, 0.7286641668683947470 ) ) ;
#1177 = CARTESIAN_POINT ( 'NONE',  ( -14.73199999999999754, 61.59499999999999886, 5.016499999999999737 ) ) ;
#1178 = ORIENTED_EDGE ( 'NONE', *, *, #30777, .T. ) ;
#1179 = CARTESIAN_POINT ( 'NONE',  ( 8.773387014951435248, 117.7735162837325760, 0.4949019102697145844 ) ) ;
#1180 = CARTESIAN_POINT ( 'NONE',  ( -11.08663849088108222, 154.4909003399924643, 1.626836423318808622 ) ) ;
#1181 = CARTESIAN_POINT ( 'NONE',  ( -57.38104596627693610, 1.839918025084400055, -1.502438007877956672 ) ) ;
#1182 = CARTESIAN_POINT ( 'NONE',  ( 12.54292998015191962, 122.5542284311838870, -1.320227961537941086 ) ) ;
#1183 = CARTESIAN_POINT ( 'NONE',  ( 0.7467592606654794851, -15.18718160513664195, -0.6397234560659120772 ) ) ;
#1184 = CARTESIAN_POINT ( 'NONE',  ( -5.008743879648553055, 158.5910778905036977, -1.550406713891092192 ) ) ;
#1185 = CIRCLE ( 'NONE', #18138, 15.21260244842765452 ) ;
#1186 = CARTESIAN_POINT ( 'NONE',  ( -46.40591231939538375, 23.70796668624020853, -2.618124260499401945 ) ) ;
#1187 = TOROIDAL_SURFACE ( 'NONE', #27700, 3.111499999999999488, 0.2540000000000000036 ) ;
#1188 = CARTESIAN_POINT ( 'NONE',  ( 4.303750855738976533, 104.6144662015456817, 2.191315714953503857 ) ) ;
#1189 = CARTESIAN_POINT ( 'NONE',  ( 14.53352838467438524, 150.4300676932417389, -1.118949361739814519 ) ) ;
#1190 = EDGE_CURVE ( 'NONE', #24894, #28559, #8603, .T. ) ;
#1191 = CARTESIAN_POINT ( 'NONE',  ( -9.538359384048678891, 124.8019839352694476, -0.1905991205270208266 ) ) ;
#1192 = VERTEX_POINT ( 'NONE', #8730 ) ;
#1193 = CARTESIAN_POINT ( 'NONE',  ( -11.58192335640140236, 123.0696236843973281, -1.706247406239837394 ) ) ;
#1194 = CARTESIAN_POINT ( 'NONE',  ( 3.016856305723133236, -15.72087675955979869, 4.784217253217923016 ) ) ;
#1195 = DIRECTION ( 'NONE',  ( -0.4849315768086535083, -0.8745520943968250194, -1.030032898892974695E-16 ) ) ;
#1196 = CARTESIAN_POINT ( 'NONE',  ( -4.512655319704103718, 118.1197172503268291, -0.6560251278375922590 ) ) ;
#1197 = CARTESIAN_POINT ( 'NONE',  ( -53.68435271313694557, 11.12367579685427721, -3.945100831076026715 ) ) ;
#1198 = AXIS2_PLACEMENT_3D ( 'NONE', #531, #13504, #10303 ) ;
#1199 = CARTESIAN_POINT ( 'NONE',  ( 4.108387141429195033, 118.2429491485453354, 0.3498641417436846868 ) ) ;
#1200 = CARTESIAN_POINT ( 'NONE',  ( 10.24420426168399700, 122.2012759285571946, 1.550633339661970700 ) ) ;
#1201 = CARTESIAN_POINT ( 'NONE',  ( -0.09153888643297225514, 38.16702564188061331, -1.140315812098650960 ) ) ;
#1202 = CARTESIAN_POINT ( 'NONE',  ( 9.820189317990141831, 117.9942579372833933, 0.1809356799706722807 ) ) ;
#1203 = CARTESIAN_POINT ( 'NONE',  ( 5.972130579385131810, 18.43406553185754504, -5.949252452957764170 ) ) ;
#1204 = CARTESIAN_POINT ( 'NONE',  ( 15.64569453857172654, 147.5723176251010784, 0.9037163853702846472 ) ) ;
#1205 = EDGE_CURVE ( 'NONE', #21382, #34762, #21073, .T. ) ;
#1206 = EDGE_CURVE ( 'NONE', #18870, #14176, #19467, .T. ) ;
#1207 = CARTESIAN_POINT ( 'NONE',  ( 15.30245393414157284, 121.3917326167944708, -0.5382413912410556334 ) ) ;
#1208 = CARTESIAN_POINT ( 'NONE',  ( -8.584304875092012566, 68.18838345945393087, 1.270000000000003348 ) ) ;
#1209 = CARTESIAN_POINT ( 'NONE',  ( -11.66725022231030984, 16.50999999999999801, 5.016499999999999737 ) ) ;
#1210 = CIRCLE ( 'NONE', #37919, 0.3809999999999984510 ) ;
#1211 = CARTESIAN_POINT ( 'NONE',  ( -57.76865908382304582, 0.8624112519253351872, 0.3783812474402863946 ) ) ;
#1212 = CARTESIAN_POINT ( 'NONE',  ( -15.89375338022620809, 121.0219768425927214, -0.2124277663179632014 ) ) ;
#1213 = VERTEX_POINT ( 'NONE', #5340 ) ;
#1214 = CARTESIAN_POINT ( 'NONE',  ( -46.93283292234357162, 25.30718002661817323, -1.635697237164840834 ) ) ;
#1215 = CARTESIAN_POINT ( 'NONE',  ( -6.899851155630319255, 121.8351476159203770, -0.4925943478833076372 ) ) ;
#1216 = CARTESIAN_POINT ( 'NONE',  ( -47.19079517381227618, 25.11791606914807318, -2.000773461933185615 ) ) ;
#1217 = EDGE_LOOP ( 'NONE', ( #24235, #36966, #30547, #19520 ) ) ;
#1218 = LINE ( 'NONE', #17379, #11060 ) ;
#1219 = CARTESIAN_POINT ( 'NONE',  ( -15.84614414026255069, 146.9522167609303267, -0.9100203137935937159 ) ) ;
#1220 = CARTESIAN_POINT ( 'NONE',  ( 4.676120195389507295, -12.14821529611620576, 1.449936329584695649 ) ) ;
#1221 = CARTESIAN_POINT ( 'NONE',  ( -5.873718653373209975, 117.7475948868982698, 0.6546600694323945202 ) ) ;
#1222 = CYLINDRICAL_SURFACE ( 'NONE', #17916, 0.2539999999999997260 ) ;
#1223 = CARTESIAN_POINT ( 'NONE',  ( 20.69515314362131519, 152.5608647341385335, 0.4887519660486651651 ) ) ;
#1224 = EDGE_CURVE ( 'NONE', #33842, #2737, #27448, .T. ) ;
#1225 = ORIENTED_EDGE ( 'NONE', *, *, #17010, .F. ) ;
#1226 = CARTESIAN_POINT ( 'NONE',  ( 2.522041008973656240, -3.380034811851383214, 3.874746376371965617 ) ) ;
#1227 = CARTESIAN_POINT ( 'NONE',  ( -0.2932902739210894727, 116.4254261620736344, -0.01852769337193111918 ) ) ;
#1228 = CARTESIAN_POINT ( 'NONE',  ( -30.19451713491628198, 70.61549828015994024, -1.270000000000007345 ) ) ;
#1229 = CYLINDRICAL_SURFACE ( 'NONE', #37378, 0.5080000000000000071 ) ;
#1230 = EDGE_CURVE ( 'NONE', #35682, #41397, #37280, .T. ) ;
#1231 = AXIS2_PLACEMENT_3D ( 'NONE', #689, #10669, #23433 ) ;
#1232 = VERTEX_POINT ( 'NONE', #4926 ) ;
#1233 = CARTESIAN_POINT ( 'NONE',  ( 8.148461401976737406, 120.7335647551133917, 1.392322577989073773 ) ) ;
#1234 = CARTESIAN_POINT ( 'NONE',  ( 0.9983407785579379023, 1.652274601622760741, 4.518288805521794238 ) ) ;
#1235 = CARTESIAN_POINT ( 'NONE',  ( 5.842876937034568563, 117.7475948868982698, 0.8887855332765352001 ) ) ;
#1236 = CARTESIAN_POINT ( 'NONE',  ( -56.60409974985478243, 4.028981045513427617, -2.444348447022182125 ) ) ;
#1237 = APPLICATION_CONTEXT ( 'automotive_design' ) ;
#1238 = CARTESIAN_POINT ( 'NONE',  ( 14.84487292597011709, 154.6636077862465015, -1.582666667450879583 ) ) ;
#1239 = CARTESIAN_POINT ( 'NONE',  ( 1.861163356255745915, -7.643417679262992870, 4.233688895527200735 ) ) ;
#1240 = CARTESIAN_POINT ( 'NONE',  ( -10.25083424799711018, 157.8242135995235458, -1.281710951059998660 ) ) ;
#1241 = ORIENTED_EDGE ( 'NONE', *, *, #20043, .F. ) ;
#1242 = ORIENTED_EDGE ( 'NONE', *, *, #38846, .T. ) ;
#1243 = CARTESIAN_POINT ( 'NONE',  ( -2.805605324221295938, 120.9854572005495044, 0.04483369291007284485 ) ) ;
#1244 = CARTESIAN_POINT ( 'NONE',  ( 6.004855586296256931, -14.40561964533282335, 2.074926179989267094 ) ) ;
#1245 = CARTESIAN_POINT ( 'NONE',  ( -47.32981077577479567, 19.92739019301375336, 5.119713631626648720 ) ) ;
#1246 = PRESENTATION_LAYER_ASSIGNMENT (  '', '', ( #26389 ) ) ;
#1247 = CARTESIAN_POINT ( 'NONE',  ( -0.4906820272735821220, 117.9496050520764783, -1.406625124191804410 ) ) ;
#1248 = ORIENTED_EDGE ( 'NONE', *, *, #15383, .T. ) ;
#1249 = CARTESIAN_POINT ( 'NONE',  ( 3.283742410131405443, 119.1333808041459577, 0.8926212079385046350 ) ) ;
#1250 = CARTESIAN_POINT ( 'NONE',  ( 14.60500000000000043, 71.11999999999999034, -1.904999999999999583 ) ) ;
#1251 = B_SPLINE_CURVE_WITH_KNOTS ( 'NONE', 3,
 ( #37493, #15109, #11928, #28112, #40505, #34317, #24488, #37091, #14901, #34727, #41122, #30895 ),
 .UNSPECIFIED., .F., .F.,
 ( 4, 2, 2, 2, 2, 4 ),
 ( 0.6055624778641834904, 0.6081219722606592271, 0.7359737730006136180, 0.8019803297504601858, 0.8679868865003068645, 1.000000000000000000 ),
 .UNSPECIFIED. ) ;
#1252 = CARTESIAN_POINT ( 'NONE',  ( 4.756879816653102111, 117.4006788688050449, 1.206942442746047783 ) ) ;
#1253 = CARTESIAN_POINT ( 'NONE',  ( -11.23106549681889810, 119.1264784044212632, 0.5965447130870018544 ) ) ;
#1254 = CARTESIAN_POINT ( 'NONE',  ( 7.384888961195664514, 14.16877864132934839, -4.050812539764339526 ) ) ;
#1255 = CARTESIAN_POINT ( 'NONE',  ( 12.84263471596168138, 130.8243885708800747, 1.276791159582618240 ) ) ;
#1256 = DIRECTION ( 'NONE',  ( -0.6294287539883864913, -0.7770581983690970640, 0.000000000000000000 ) ) ;
#1257 = CARTESIAN_POINT ( 'NONE',  ( 15.73021646601966239, 121.2535323456646523, -0.2080526303901671648 ) ) ;
#1258 = DIRECTION ( 'NONE',  ( 5.188838149069472160E-16, -1.699382548006136559E-16, -1.000000000000000000 ) ) ;
#1259 = CARTESIAN_POINT ( 'NONE',  ( -55.96400101662930382, 4.835333878257412010, 2.481606003085900625 ) ) ;
#1260 = SURFACE_STYLE_FILL_AREA ( #17415 ) ;
#1261 = CARTESIAN_POINT ( 'NONE',  ( -57.53497731650991653, 2.247686704661286505, 1.882970859819747433 ) ) ;
#1262 = CARTESIAN_POINT ( 'NONE',  ( -57.61145207080065234, 1.897832464664358509, 1.722955516460566772 ) ) ;
#1263 = CARTESIAN_POINT ( 'NONE',  ( -4.556770483176405762, 118.1065360176216501, 0.4935596350356394879 ) ) ;
#1264 = FACE_OUTER_BOUND ( 'NONE', #33978, .T. ) ;
#1265 = VERTEX_POINT ( 'NONE', #17883 ) ;
#1266 = CARTESIAN_POINT ( 'NONE',  ( -43.49527490626578441, 22.26612824116996237, 2.150709692269567874 ) ) ;
#1267 = CARTESIAN_POINT ( 'NONE',  ( 6.165645682523538618, 119.5752110173503695, -1.007953236233805283 ) ) ;
#1268 = CARTESIAN_POINT ( 'NONE',  ( -7.499048524201011645, 123.6595150816924047, -0.1842243911843318704 ) ) ;
#1269 = CARTESIAN_POINT ( 'NONE',  ( 4.563396916661870861, 118.0729906482839340, 0.7687451279623377376 ) ) ;
#1270 = CARTESIAN_POINT ( 'NONE',  ( -9.561025033428087738, 123.8224200044116827, -0.8726585919039497874 ) ) ;
#1271 = CARTESIAN_POINT ( 'NONE',  ( -0.06880952194489776963, 115.7029491485453008, -1.763577818935210040 ) ) ;
#1272 = CARTESIAN_POINT ( 'NONE',  ( 3.403262595199820773, 117.9496052708406921, -1.151714290375731142 ) ) ;
#1273 = CARTESIAN_POINT ( 'NONE',  ( -3.290491044589036740, 30.52917213649525507, -3.264312889705288878 ) ) ;
#1274 = CARTESIAN_POINT ( 'NONE',  ( 0.02156534543286487207, 156.6359106937186709, -1.079218069903262300 ) ) ;
#1275 = FACE_OUTER_BOUND ( 'NONE', #11841, .T. ) ;
#1276 = CARTESIAN_POINT ( 'NONE',  ( -30.20416046766209917, 71.17241488000101413, 1.269999999999991580 ) ) ;
#1277 = CARTESIAN_POINT ( 'NONE',  ( 8.799660282941641043, 117.6859426315424599, 0.07877357120233691168 ) ) ;
#1278 = CARTESIAN_POINT ( 'NONE',  ( -15.72791684456901962, 146.8976217498096162, -0.1132496748128679204 ) ) ;
#1279 = CARTESIAN_POINT ( 'NONE',  ( -6.540217103314379345E-14, 82.64346620154573486, 2.383338306179204368E-29 ) ) ;
#1280 = CARTESIAN_POINT ( 'NONE',  ( 2.883180212088789052, 116.9538966677400254, 0.4754005367760563705 ) ) ;
#1281 = DIRECTION ( 'NONE',  ( 1.011795553208986377E-16, 1.000000000000000000, -0.000000000000000000 ) ) ;
#1282 = CARTESIAN_POINT ( 'NONE',  ( 3.009962208777686499, -14.98531826913061771, 3.912431539232285704 ) ) ;
#1283 = CARTESIAN_POINT ( 'NONE',  ( -18.71424449056256378, 147.4429432625130119, 1.699796950208447788 ) ) ;
#1284 = CARTESIAN_POINT ( 'NONE',  ( 0.9053751552131774627, -6.120233167431497812, -0.3594991891349857416 ) ) ;
#1285 = CARTESIAN_POINT ( 'NONE',  ( -13.21954506825633402, 156.9672759736256467, -0.8747755986887105761 ) ) ;
#1286 = CARTESIAN_POINT ( 'NONE',  ( 0.1873809172457601979, 14.59626481882237492, -0.9553521702420578743 ) ) ;
#1287 = ORIENTED_EDGE ( 'NONE', *, *, #17004, .T. ) ;
#1288 = CARTESIAN_POINT ( 'NONE',  ( -50.77948459960266092, 12.22376025917672138, 0.7375277020707294851 ) ) ;
#1289 = CARTESIAN_POINT ( 'NONE',  ( 1.370820134808094837, 106.2483430537416638, 5.168860673143087503 ) ) ;
#1290 = ITEM_DEFINED_TRANSFORMATION ( 'NONE', 'NONE', #5338,  #3275 ) ;
#1291 = CARTESIAN_POINT ( 'NONE',  ( -5.220694793870528372, 121.0999079655412203, 0.2922795305089894713 ) ) ;
#1292 = CARTESIAN_POINT ( 'NONE',  ( 4.658995561375286698, -13.35466759734559083, 3.413121997863386881 ) ) ;
#1293 = CARTESIAN_POINT ( 'NONE',  ( 3.531217591821261159, 156.5024071230465097, -1.273243333543745859 ) ) ;
#1294 = EDGE_LOOP ( 'NONE', ( #9321, #12008, #12666, #41017 ) ) ;
#1295 = CIRCLE ( 'NONE', #30513, 0.2540000000000000036 ) ;
#1296 = DIRECTION ( 'NONE',  ( 9.627370216492862708E-17, 1.000000000000000000, -0.000000000000000000 ) ) ;
#1297 = CARTESIAN_POINT ( 'NONE',  ( 2.821697343786723877, -14.64683725402170289, 4.582568527534213843 ) ) ;
#1298 = CARTESIAN_POINT ( 'NONE',  ( -4.963187677402431497, 117.4661819789754986, -0.9730286260216215455 ) ) ;
#1299 = CARTESIAN_POINT ( 'NONE',  ( 8.537819074431615363, 123.3353292868209365, 0.08920952957173446107 ) ) ;
#1300 = ORIENTED_EDGE ( 'NONE', *, *, #25394, .T. ) ;
#1301 = CARTESIAN_POINT ( 'NONE',  ( 1.195985117830443034, 118.4063602595805946, 0.6806364119286733017 ) ) ;
#1302 = CARTESIAN_POINT ( 'NONE',  ( 4.258623371604620012, 112.0483952545076818, 2.856521178696663554 ) ) ;
#1303 = CARTESIAN_POINT ( 'NONE',  ( -5.517349593794012463, 28.10803576007639037, 0.4164286583522215368 ) ) ;
#1304 = DIRECTION ( 'NONE',  ( 5.188838149069472160E-16, -1.699382548006136559E-16, -1.000000000000000000 ) ) ;
#1305 = CARTESIAN_POINT ( 'NONE',  ( 2.784667331447688632, 116.5968896900294709, -0.09290643507641017929 ) ) ;
#1306 = CIRCLE ( 'NONE', #32565, 0.5080000000000000071 ) ;
#1307 = CYLINDRICAL_SURFACE ( 'NONE', #5741, 18.32410244842765934 ) ;
#1308 = VECTOR ( 'NONE', #32914, 1000.000000000000000 ) ;
#1309 = CARTESIAN_POINT ( 'NONE',  ( 1.985468892469562485, -15.55060482525283305, 5.976321803999622873 ) ) ;
#1310 = FACE_OUTER_BOUND ( 'NONE', #18095, .T. ) ;
#1311 = CARTESIAN_POINT ( 'NONE',  ( -2.880736501481947265, 31.22451072257329585, 0.7774695130801791976 ) ) ;
#1312 = CARTESIAN_POINT ( 'NONE',  ( 4.042996894205697522, 118.2594131075661608, 0.9467780975002215715 ) ) ;
#1313 = ORIENTED_EDGE ( 'NONE', *, *, #40737, .T. ) ;
#1314 = CARTESIAN_POINT ( 'NONE',  ( 5.116497545627949783, 15.83618160547830911, 6.690270154343205711 ) ) ;
#1315 = CARTESIAN_POINT ( 'NONE',  ( -2.430891878037258813, 117.4063284849774078, -0.7237017793962934320 ) ) ;
#1316 = CARTESIAN_POINT ( 'NONE',  ( -2.258874542396802187, 118.3648483361698851, -0.8858652710056678092 ) ) ;
#1317 = CARTESIAN_POINT ( 'NONE',  ( 4.957728306477804381, 117.4049568006667670, 1.028863336443936127 ) ) ;
#1318 = CARTESIAN_POINT ( 'NONE',  ( -6.507153519498132566E-14, 76.29346620154572634, 3.067795752821199360E-29 ) ) ;
#1319 = FACE_OUTER_BOUND ( 'NONE', #3397, .T. ) ;
#1320 = CARTESIAN_POINT ( 'NONE',  ( 3.728136974946417492, 6.765255174955887796, 2.739693761753763113 ) ) ;
#1321 = CARTESIAN_POINT ( 'NONE',  ( -7.842268484490568348, 73.30875693322846587, -1.523999999999996247 ) ) ;
#1322 = CARTESIAN_POINT ( 'NONE',  ( -5.276743917130819916, 115.6909491485453003, 0.8116159901532213894 ) ) ;
#1323 = CARTESIAN_POINT ( 'NONE',  ( 3.403332384622693052, -13.60094159685824877, 2.654810364998238192 ) ) ;
#1324 = CARTESIAN_POINT ( 'NONE',  ( 1.889402974297992754, 108.8931014686503289, -4.028630146538900725 ) ) ;
#1325 = CARTESIAN_POINT ( 'NONE',  ( 0.03201377673046572336, 33.52827609515317420, 3.383309648808628278 ) ) ;
#1326 = DIRECTION ( 'NONE',  ( -0.6594218222380416883, -0.7517731442105793915, 0.000000000000000000 ) ) ;
#1327 = ORIENTED_EDGE ( 'NONE', *, *, #33725, .F. ) ;
#1328 = CARTESIAN_POINT ( 'NONE',  ( -3.857386620090222262, 105.1226137608093438, -3.700239550084083895 ) ) ;
#1329 = CARTESIAN_POINT ( 'NONE',  ( 1.959965285483297404, -15.65532139403495648, 5.519319896091174904 ) ) ;
#1330 = CARTESIAN_POINT ( 'NONE',  ( -12.41883037655689037, 155.1253022143813496, 1.737092194502518616 ) ) ;
#1331 = CARTESIAN_POINT ( 'NONE',  ( -3.178183004559932190, -7.902942162671289239, -3.366045245292264010 ) ) ;
#1332 = ORIENTED_EDGE ( 'NONE', *, *, #22941, .T. ) ;
#1333 = EDGE_LOOP ( 'NONE', ( #21722, #36591, #25860, #38452 ) ) ;
#1334 = CYLINDRICAL_SURFACE ( 'NONE', #23814, 5.588000000000006295 ) ;
#1335 = CARTESIAN_POINT ( 'NONE',  ( 0.2359694434508981808, 106.4201689084969047, 5.118158396747612748 ) ) ;
#1336 = CARTESIAN_POINT ( 'NONE',  ( -9.865641862003254658, 123.3250567171901082, 0.7964883383408416506 ) ) ;
#1337 = CARTESIAN_POINT ( 'NONE',  ( -44.94860120752490218, 21.36157935410335895, 3.600951685817770365 ) ) ;
#1338 = CIRCLE ( 'NONE', #14928, 2.857500000000000817 ) ;
#1339 = CARTESIAN_POINT ( 'NONE',  ( 11.23500844718012992, 122.9575399027323073, -1.191779604289733285 ) ) ;
#1340 = CIRCLE ( 'NONE', #32609, 1.396999999999998909 ) ;
#1341 = CARTESIAN_POINT ( 'NONE',  ( -13.31282764718934608, 122.3357896625302459, -1.791091420989350258 ) ) ;
#1342 = FACE_OUTER_BOUND ( 'NONE', #40799, .T. ) ;
#1343 = CARTESIAN_POINT ( 'NONE',  ( 4.261500844742492689, 118.2248151516817956, -0.2975339631682852870 ) ) ;
#1344 = CARTESIAN_POINT ( 'NONE',  ( 15.59522120955183055, 147.8873989650969918, -0.4103944809294444163 ) ) ;
#1345 = ORIENTED_EDGE ( 'NONE', *, *, #4341, .F. ) ;
#1346 = CARTESIAN_POINT ( 'NONE',  ( 2.994295736468014280, -14.77441112906794984, 3.968895097548184037 ) ) ;
#1347 = DIRECTION ( 'NONE',  ( -0.6294287539883844929, -0.7770581983690987293, 0.000000000000000000 ) ) ;
#1348 = CARTESIAN_POINT ( 'NONE',  ( -57.55255837555638010, 1.471581310123065700, 1.351947345340770656 ) ) ;
#1349 = CARTESIAN_POINT ( 'NONE',  ( 2.362155674307470310, -13.89060443905824371, -3.983575812745122846 ) ) ;
#1350 = CARTESIAN_POINT ( 'NONE',  ( 13.72925640114926082, 131.0408573235120571, 1.723107598632783066 ) ) ;
#1351 = CARTESIAN_POINT ( 'NONE',  ( -3.646310357438999894, 28.62608726100145873, 1.835561881698716924 ) ) ;
#1352 = CARTESIAN_POINT ( 'NONE',  ( -6.805961295028136071, 123.7298400107579255, -0.09869924339446545236 ) ) ;
#1353 = CARTESIAN_POINT ( 'NONE',  ( 3.935102970030661673, 16.48578375386999539, 2.424025302511324309 ) ) ;
#1354 = CARTESIAN_POINT ( 'NONE',  ( 5.300740673260364133, 121.3529869156830046, 0.1337733589788159816 ) ) ;
#1355 = CARTESIAN_POINT ( 'NONE',  ( -46.79259615289808494, 25.76143605979575923, 1.464524644194001635 ) ) ;
#1356 = AXIS2_PLACEMENT_3D ( 'NONE', #28783, #38173, #12177 ) ;
#1357 = AXIS2_PLACEMENT_3D ( 'NONE', #16330, #30595, #17389 ) ;
#1358 = CARTESIAN_POINT ( 'NONE',  ( -53.01551111795198068, 8.729259440421092364, -0.3204493394367286530 ) ) ;
#1359 = CARTESIAN_POINT ( 'NONE',  ( -2.174026700015069036, 116.2368718333218425, -0.1864608981796752329 ) ) ;
#1360 = CARTESIAN_POINT ( 'NONE',  ( -6.374728672999452917E-14, 124.9344662015457317, 7.707042028354222152E-17 ) ) ;
#1361 = CARTESIAN_POINT ( 'NONE',  ( -30.75918919842648336, 69.77432548395512413, 1.269999999999991358 ) ) ;
#1362 = CARTESIAN_POINT ( 'NONE',  ( -0.3831293027247411609, 105.9761014636926149, 5.290230343685635717 ) ) ;
#1363 = CARTESIAN_POINT ( 'NONE',  ( -2.958531772299361595, 44.28946620154572855, -1.329372033065076675 ) ) ;
#1364 = CARTESIAN_POINT ( 'NONE',  ( 5.007560425261973869, -3.380029175189206203, 6.774419414089246416 ) ) ;
#1365 = DIRECTION ( 'NONE',  ( -0.8745520943968250194, 0.4849315768086532863, -5.361993529360574930E-16 ) ) ;
#1366 = FACE_OUTER_BOUND ( 'NONE', #35222, .T. ) ;
#1367 = CARTESIAN_POINT ( 'NONE',  ( -58.16317756775203662, 1.603007233358586081, 1.028822313162477631 ) ) ;
#1368 = EDGE_CURVE ( 'NONE', #6241, #29982, #30885, .T. ) ;
#1369 = CARTESIAN_POINT ( 'NONE',  ( -4.973569738608247803, 117.3993868453981548, -0.9750659555622913643 ) ) ;
#1370 = CARTESIAN_POINT ( 'NONE',  ( -13.44960824739634653, 119.6710471929552000, 0.1296808650140444663 ) ) ;
#1371 = ORIENTED_EDGE ( 'NONE', *, *, #327, .F. ) ;
#1372 = CARTESIAN_POINT ( 'NONE',  ( -57.96050266256141725, 2.261623006455215634, -0.4698253072426236132 ) ) ;
#1373 = CARTESIAN_POINT ( 'NONE',  ( -5.078986093043185157, 72.99146620154573384, -0.1014902294541238092 ) ) ;
#1374 = VERTEX_POINT ( 'NONE', #11919 ) ;
#1375 = DIRECTION ( 'NONE',  ( -0.9998501190848629872, -0.01731298258490746381, -8.537024980200835623E-16 ) ) ;
#1376 = CARTESIAN_POINT ( 'NONE',  ( -6.503408402854686798, 121.7799126398724354, -0.1299535771408516782 ) ) ;
#1377 = CARTESIAN_POINT ( 'NONE',  ( 5.498554953534677381, -14.76196523188227872, 3.265392988355040327 ) ) ;
#1378 = CARTESIAN_POINT ( 'NONE',  ( -19.52548538990948757, 136.0480396440595996, 1.529100095608182830 ) ) ;
#1379 = CARTESIAN_POINT ( 'NONE',  ( 15.93800727448848065, 121.3860667298135070, 0.7466885930842024344 ) ) ;
#1380 = CARTESIAN_POINT ( 'NONE',  ( 20.36908824613697888, 132.1502320877631007, -0.7851131432546852862 ) ) ;
#1381 = CARTESIAN_POINT ( 'NONE',  ( -29.22193451008083542, 63.05474646772795921, 1.269999999999993578 ) ) ;
#1382 = CARTESIAN_POINT ( 'NONE',  ( -21.88244685892446384, 151.4414241944827495, -0.6640443303913105000 ) ) ;
#1383 = CARTESIAN_POINT ( 'NONE',  ( -50.24489010722032845, 15.90173676724104723, -4.871286304140493684 ) ) ;
#1384 = ADVANCED_FACE ( 'NONE', ( #1725 ), #14619, .F. ) ;
#1385 = CARTESIAN_POINT ( 'NONE',  ( 4.973153348176213129, 117.3993868326347183, 0.9753024067320210655 ) ) ;
#1386 = ORIENTED_EDGE ( 'NONE', *, *, #433, .F. ) ;
#1387 = CARTESIAN_POINT ( 'NONE',  ( -2.184846125065896150, 116.1979711210248780, -0.02027492182686356156 ) ) ;
#1388 = CARTESIAN_POINT ( 'NONE',  ( -3.455858276899955950, 119.9243055703230851, 0.6230356542855080004 ) ) ;
#1389 = CARTESIAN_POINT ( 'NONE',  ( -57.94428360355602337, 0.6253113912629046922, -0.9307620923768729071 ) ) ;
#1390 = CARTESIAN_POINT ( 'NONE',  ( 19.63947405400084634, 148.8045834396381508, -1.723899180582558088 ) ) ;
#1391 = CARTESIAN_POINT ( 'NONE',  ( 0.9474642044963531573, -6.343762114497205395, -0.2236011429025598352 ) ) ;
#1392 = CARTESIAN_POINT ( 'NONE',  ( -14.34163035669555164, 121.9874158357064857, -1.600522166921893863 ) ) ;
#1393 = CARTESIAN_POINT ( 'NONE',  ( -46.91604881613255174, 25.30076613767161220, -1.786867259277528985 ) ) ;
#1394 = AXIS2_PLACEMENT_3D ( 'NONE', #3654, #3026, #12796 ) ;
#1395 = CARTESIAN_POINT ( 'NONE',  ( 12.75300196040200085, 152.1353413313561305, -1.119124812251137469 ) ) ;
#1396 = CARTESIAN_POINT ( 'NONE',  ( -9.118174893680297544, 124.1671967267183589, -0.1822028344259497834 ) ) ;
#1397 = VERTEX_POINT ( 'NONE', #25016 ) ;
#1398 = CARTESIAN_POINT ( 'NONE',  ( -1.339510839693951239, 119.4570717772418220, -0.6353817622545779864 ) ) ;
#1399 = CARTESIAN_POINT ( 'NONE',  ( 4.776532240430319654, -15.60394515218366251, 2.960345780779299663 ) ) ;
#1400 = DIRECTION ( 'NONE',  ( -0.4849315768086535083, -0.8745520943968250194, -1.030032898892974695E-16 ) ) ;
#1401 = CARTESIAN_POINT ( 'NONE',  ( -4.350331169090538630, 118.1836411042714019, -0.6150010472375504467 ) ) ;
#1402 = EDGE_CURVE ( 'NONE', #5536, #5052, #39044, .T. ) ;
#1403 = CARTESIAN_POINT ( 'NONE',  ( -51.73272837791831336, 13.19950324185369794, -4.393710239503588078 ) ) ;
#1404 = DIRECTION ( 'NONE',  ( -0.000000000000000000, -0.000000000000000000, -1.000000000000000000 ) ) ;
#1405 = CARTESIAN_POINT ( 'NONE',  ( -0.02969003158484915736, 157.1787724364823760, 1.485810588193620774 ) ) ;
#1406 = CARTESIAN_POINT ( 'NONE',  ( -11.24191166894635074, 82.34025985790688651, -1.523999999999999799 ) ) ;
#1407 = ADVANCED_FACE ( 'NONE', ( #39281 ), #32891, .T. ) ;
#1408 = CARTESIAN_POINT ( 'NONE',  ( 5.772319165917887851, 116.9338547871927858, 0.1153446742911717754 ) ) ;
#1409 = EDGE_CURVE ( 'NONE', #15145, #13978, #34982, .T. ) ;
#1410 = CARTESIAN_POINT ( 'NONE',  ( 6.774419413954826830, 18.20997082500984376, -5.007560425318187569 ) ) ;
#1411 = CARTESIAN_POINT ( 'NONE',  ( 14.33905310436362690, 139.0340687859245463, 0.7442083991839667512 ) ) ;
#1412 = CARTESIAN_POINT ( 'NONE',  ( 2.940475496281206969, 117.1197906563906344, -0.4390297717439133884 ) ) ;
#1413 = CARTESIAN_POINT ( 'NONE',  ( -47.19240717248688810, 20.04893757306798108, -5.078271723505031865 ) ) ;
#1414 = AXIS2_PLACEMENT_3D ( 'NONE', #34555, #28573, #25376 ) ;
#1415 = DIRECTION ( 'NONE',  ( 0.4849315768086426282, 0.8745520943968310146, 1.030032898892908135E-16 ) ) ;
#1416 = CARTESIAN_POINT ( 'NONE',  ( -57.99953387342350908, 0.4830015814202143209, 0.7353922615980046373 ) ) ;
#1417 = CARTESIAN_POINT ( 'NONE',  ( -17.27060146982332611, 122.7565812399420651, -0.2921901055230265998 ) ) ;
#1418 = ORIENTED_EDGE ( 'NONE', *, *, #18535, .T. ) ;
#1419 = CARTESIAN_POINT ( 'NONE',  ( -46.81215924274956564, 25.79096025118141711, -0.6894041771339123326 ) ) ;
#1420 = CARTESIAN_POINT ( 'NONE',  ( -5.784570514964185506, 121.1847750061955793, -0.5060016832306288848 ) ) ;
#1421 = LINE ( 'NONE', #23334, #36691 ) ;
#1422 = VERTEX_POINT ( 'NONE', #19455 ) ;
#1423 = CARTESIAN_POINT ( 'NONE',  ( 3.987297185843972080, 118.7629491485453741, -0.9448535219813100072 ) ) ;
#1424 = CARTESIAN_POINT ( 'NONE',  ( -8.876935545690720630, 123.7004864364556909, -0.3337242414277967750 ) ) ;
#1425 = CARTESIAN_POINT ( 'NONE',  ( 2.039565395400614989, -15.13835760176744571, 5.886961163765535687 ) ) ;
#1426 = CARTESIAN_POINT ( 'NONE',  ( -19.32406529451199262, 152.1947311750261065, 1.288948053361433255 ) ) ;
#1427 = PLANE ( 'NONE',  #33605 ) ;
#1428 = CARTESIAN_POINT ( 'NONE',  ( 17.22116264704559541, 122.7389118244895769, 0.4537515290936993684 ) ) ;
#1429 = CARTESIAN_POINT ( 'NONE',  ( 15.37911286811759659, 147.8337517708649500, 0.3739466042392066147 ) ) ;
#1430 = EDGE_LOOP ( 'NONE', ( #22979, #36119, #20047, #567 ) ) ;
#1431 = CARTESIAN_POINT ( 'NONE',  ( 3.501419995798253915, -2.955197114699519734, 3.043391175950921568 ) ) ;
#1432 = CARTESIAN_POINT ( 'NONE',  ( -4.716951831472304235, 116.7562497393984415, -0.1081823505139635905 ) ) ;
#1433 = DIRECTION ( 'NONE',  ( -0.9998004120163608288, 0.000000000000000000, -0.01997839162482747608 ) ) ;
#1434 = EDGE_LOOP ( 'NONE', ( #35582, #8226, #15104, #26764, #32645, #9848, #37142, #40822, #14935, #33892, #11987, #1585, #611 ) ) ;
#1435 = CARTESIAN_POINT ( 'NONE',  ( 6.391738861559880469, 119.5489620839046410, 1.259756172207089575 ) ) ;
#1436 =( BOUNDED_CURVE ( )  B_SPLINE_CURVE ( 3, ( #33648, #13827, #33854, #14649 ),
 .UNSPECIFIED., .F., .F. ) 
 B_SPLINE_CURVE_WITH_KNOTS ( ( 4, 4 ),
 ( 0.09183118002780921163, 0.1539179638657816873 ),
 .UNSPECIFIED. ) 
 CURVE ( )  GEOMETRIC_REPRESENTATION_ITEM ( )  RATIONAL_B_SPLINE_CURVE ( ( 0.7001390048907335517, 0.6477646404348715858, 0.6056696592518493460, 0.5738540613416668323 ) ) 
 REPRESENTATION_ITEM ( '' )  );
#1437 = CARTESIAN_POINT ( 'NONE',  ( -4.626086514281606554, -10.66701884381306087, 0.02375484599842511355 ) ) ;
#1438 = CARTESIAN_POINT ( 'NONE',  ( 0.3664415811650883481, 117.3568105388816321, 0.4447864970249673089 ) ) ;
#1439 = CARTESIAN_POINT ( 'NONE',  ( -55.57144106515218596, 6.156191000079303421, -3.024401744048434537 ) ) ;
#1440 = CARTESIAN_POINT ( 'NONE',  ( 20.67621894907592051, 148.5655811199389689, -1.615315227278341315 ) ) ;
#1441 = CARTESIAN_POINT ( 'NONE',  ( -4.626086514281606554, -10.66701884381306087, 0.02375484599842511355 ) ) ;
#1442 = CARTESIAN_POINT ( 'NONE',  ( -4.843103592331963192, 117.3073154462328063, -0.6875571908837336821 ) ) ;
#1443 = AXIS2_PLACEMENT_3D ( 'NONE', #3067, #22198, #38835 ) ;
#1444 = ORIENTED_EDGE ( 'NONE', *, *, #38421, .F. ) ;
#1445 = EDGE_CURVE ( 'NONE', #38820, #27671, #9640, .T. ) ;
#1446 = CARTESIAN_POINT ( 'NONE',  ( -12.97778284513273483, 133.8854804328748571, -0.04088747601382857616 ) ) ;
#1447 = CARTESIAN_POINT ( 'NONE',  ( 4.031817627494778122, -15.29123897636591778, 5.054998095871475527 ) ) ;
#1448 = EDGE_CURVE ( 'NONE', #40423, #2340, #26112, .T. ) ;
#1449 = CIRCLE ( 'NONE', #38837, 0.6349999999999998979 ) ;
#1450 = DIRECTION ( 'NONE',  ( 0.8745520943968240202, -0.4849315768086551182, 4.268512490100404500E-16 ) ) ;
#1451 = CARTESIAN_POINT ( 'NONE',  ( -3.409246530723191171, 109.2372022974443126, -3.913087349919080804 ) ) ;
#1452 = ORIENTED_EDGE ( 'NONE', *, *, #7804, .T. ) ;
#1453 = CARTESIAN_POINT ( 'NONE',  ( 14.93497932922872629, 152.9649416503947634, 2.345758529409812887 ) ) ;
#1454 = FACE_OUTER_BOUND ( 'NONE', #20510, .T. ) ;
#1455 = DIRECTION ( 'NONE',  ( 0.8745520943968240202, -0.4849315768086553402, 6.829619984160650158E-16 ) ) ;
#1456 = CARTESIAN_POINT ( 'NONE',  ( -9.536130858166004032, 118.4542681464805298, 0.5810392422064989404 ) ) ;
#1457 = EDGE_CURVE ( 'NONE', #26787, #35651, #16578, .T. ) ;
#1458 = CARTESIAN_POINT ( 'NONE',  ( -8.331803066987694351, 8.350395779143005015, -1.420432620954584113 ) ) ;
#1459 = CARTESIAN_POINT ( 'NONE',  ( 14.07483374865158687, 150.3034377993741657, 1.364178037702376223 ) ) ;
#1460 = DIRECTION ( 'NONE',  ( -1.000000000000000000, 0.000000000000000000, 0.000000000000000000 ) ) ;
#1461 = CARTESIAN_POINT ( 'NONE',  ( 22.79600589338267369, 150.0845277111093310, -0.2694608383616128311 ) ) ;
#1462 = CARTESIAN_POINT ( 'NONE',  ( -6.318938770521974391, 64.36956080246774548, -1.523999999999994026 ) ) ;
#1463 = EDGE_CURVE ( 'NONE', #18019, #32240, #9670, .T. ) ;
#1464 = CARTESIAN_POINT ( 'NONE',  ( -57.72392508873495842, 1.101746749479270093, 1.179667423805870863 ) ) ;
#1465 =( NAMED_UNIT ( * ) SI_UNIT ( $, .STERADIAN. ) SOLID_ANGLE_UNIT ( ) );
#1466 = AXIS2_PLACEMENT_3D ( 'NONE', #18039, #21025, #19252 ) ;
#1467 = CARTESIAN_POINT ( 'NONE',  ( -57.09878488423309051, 3.216020309495956742, 2.217633722229532367 ) ) ;
#1468 = CARTESIAN_POINT ( 'NONE',  ( -58.46978370654361612, 0.04540555296617620334, 0.7440089614489153735 ) ) ;
#1469 = CARTESIAN_POINT ( 'NONE',  ( -4.164425106054416403, 118.2394406760751622, 0.2263534819914557739 ) ) ;
#1470 = CARTESIAN_POINT ( 'NONE',  ( 3.264763291910224741, 108.5668738132266071, -4.052445894262588055 ) ) ;
#1471 = ORIENTED_EDGE ( 'NONE', *, *, #3988, .T. ) ;
#1472 = CARTESIAN_POINT ( 'NONE',  ( -53.45432727069204759, 10.77832982246877691, 4.078803160923774485 ) ) ;
#1473 = CARTESIAN_POINT ( 'NONE',  ( 6.184646281355417941, 119.6155407647441962, -1.003826558285236592 ) ) ;
#1474 = CARTESIAN_POINT ( 'NONE',  ( -5.245364206137289820, 116.4655405006298849, -1.092799426751067005 ) ) ;
#1476 = CARTESIAN_POINT ( 'NONE',  ( 4.299732312588651517, 118.2124281450362133, 0.4976895454704568511 ) ) ;
#1475 = AXIS2_PLACEMENT_3D ( 'NONE', #28043, #11863, #37848 ) ;
#1477 = CARTESIAN_POINT ( 'NONE',  ( -9.839787852217179775, 124.1914461168675530, -0.8951504484210819346 ) ) ;
#1478 = CARTESIAN_POINT ( 'NONE',  ( -0.7903546951415685307, 115.7028259477297922, -1.754549543117774446 ) ) ;
#1479 = FACE_OUTER_BOUND ( 'NONE', #26209, .T. ) ;
#1480 = ORIENTED_EDGE ( 'NONE', *, *, #26494, .F. ) ;
#1481 = CARTESIAN_POINT ( 'NONE',  ( 3.592701615362551504, 108.6576027043044377, -3.989964801148524476 ) ) ;
#1482 = CARTESIAN_POINT ( 'NONE',  ( -2.639528505629704647, 120.4390018212493914, -0.4929570044210888624 ) ) ;
#1483 = CARTESIAN_POINT ( 'NONE',  ( -4.705839724742440389, 116.0444662015457595, 3.565396701626624143 ) ) ;
#1484 = CARTESIAN_POINT ( 'NONE',  ( -47.20408514806452871, 20.03888983422028502, 5.082056583517504222 ) ) ;
#1485 = DIRECTION ( 'NONE',  ( 9.627370216492862708E-17, 1.000000000000000000, -0.000000000000000000 ) ) ;
#1486 = CARTESIAN_POINT ( 'NONE',  ( -9.426429330012480179, 124.7671717571762429, -0.04963531977156410840 ) ) ;
#1487 = CARTESIAN_POINT ( 'NONE',  ( 4.349802767100347189, -10.92635770930747796, -1.576909098649299512 ) ) ;
#1488 = CARTESIAN_POINT ( 'NONE',  ( 1.924101685567825903, 116.8467566806161386, 0.3833193769953583963 ) ) ;
#1489 = CARTESIAN_POINT ( 'NONE',  ( 5.965356522962860453, 65.30181249999998272, -5.016499999999999737 ) ) ;
#1491 = CARTESIAN_POINT ( 'NONE',  ( 13.78108617287050564, 121.3979351292862816, -1.006787891297146409 ) ) ;
#1490 = CARTESIAN_POINT ( 'NONE',  ( 2.915559332840946816, -14.19431184016030301, 0.3483797586856177686 ) ) ;
#1492 = CARTESIAN_POINT ( 'NONE',  ( -2.445625216771193156, 119.3768144667271542, 0.6598031440805112169 ) ) ;
#1493 = AXIS2_PLACEMENT_3D ( 'NONE', #33530, #39926, #36719 ) ;
#1494 = CARTESIAN_POINT ( 'NONE',  ( -0.7897743334665792148, -0.9462621144725560374, 0.5691593732151654095 ) ) ;
#1495 = CARTESIAN_POINT ( 'NONE',  ( -13.27770485956329694, 119.7426348059052685, -0.8357656065649388122 ) ) ;
#1496 = CARTESIAN_POINT ( 'NONE',  ( 0.5056692551311988693, 10.92592451650425112, 0.8332994872028685052 ) ) ;
#1497 = ORIENTED_EDGE ( 'NONE', *, *, #31314, .F. ) ;
#1498 = CARTESIAN_POINT ( 'NONE',  ( -48.46138709710082537, 15.22468166490328123, 0.8008350491754776534 ) ) ;
#1499 = ITEM_DEFINED_TRANSFORMATION ( 'NONE', 'NONE', #25723,  #3275 ) ;
#1500 = CARTESIAN_POINT ( 'NONE',  ( -8.332953031246923103, 122.7091975629380585, 0.3740907431100291003 ) ) ;
#1501 = CARTESIAN_POINT ( 'NONE',  ( 3.638845723804262189, -14.60113053194242383, 5.212470003951681363 ) ) ;
#1502 = CARTESIAN_POINT ( 'NONE',  ( 0.8386157876099215036, 156.7682548876429109, -1.206618248707299834 ) ) ;
#1503 = VERTEX_POINT ( 'NONE', #6481 ) ;
#1504 = AXIS2_PLACEMENT_3D ( 'NONE', #20658, #4506, #4090 ) ;
#1505 = CARTESIAN_POINT ( 'NONE',  ( 4.553366535818831551, 104.6144662015457811, 1.608775678111619145 ) ) ;
#1506 = VECTOR ( 'NONE', #13715, 1000.000000000000227 ) ;
#1507 = CARTESIAN_POINT ( 'NONE',  ( 3.258219809910011033, -14.04213616937880005, 2.843395319141139410 ) ) ;
#1508 = CARTESIAN_POINT ( 'NONE',  ( -4.894673311264758020, 117.5446123977157100, -1.081256949576274273 ) ) ;
#1509 = AXIS2_PLACEMENT_3D ( 'NONE', #17697, #33711, #23885 ) ;
#1510 = CARTESIAN_POINT ( 'NONE',  ( 7.045353508903499318, 122.0728772437221323, 0.1110369332536843695 ) ) ;
#1511 = ORIENTED_EDGE ( 'NONE', *, *, #11811, .F. ) ;
#1512 = CARTESIAN_POINT ( 'NONE',  ( 20.12154232503847595, 149.0333503175929479, 2.470054797493932419 ) ) ;
#1513 = CARTESIAN_POINT ( 'NONE',  ( 5.084164759140180401, 114.9388725758527272, 1.737832868923124607 ) ) ;
#1514 = CARTESIAN_POINT ( 'NONE',  ( 12.21488373879589240, 17.14499999999999957, 4.381499999999999950 ) ) ;
#1515 = ADVANCED_FACE ( 'NONE', ( #108 ), #22221, .F. ) ;
#1516 = CARTESIAN_POINT ( 'NONE',  ( 0.03256023585714045571, 157.9544661776888290, -1.629447346748784220 ) ) ;
#1517 = CARTESIAN_POINT ( 'NONE',  ( 6.908764576387254941, 117.1865127098105575, 0.01035743554829997824 ) ) ;
#1518 = EDGE_CURVE ( 'NONE', #22436, #1811, #13071, .T. ) ;
#1519 = CARTESIAN_POINT ( 'NONE',  ( 9.925711944554073796, 78.55658865046544292, -5.016499999999999737 ) ) ;
#1520 = CARTESIAN_POINT ( 'NONE',  ( 1.910917866030142909, -15.65413017954154995, 5.882152347191063058 ) ) ;
#1521 = CARTESIAN_POINT ( 'NONE',  ( 4.862091962581056137, 117.4116108956684030, 1.165648838277617338 ) ) ;
#1522 = CARTESIAN_POINT ( 'NONE',  ( 1.534760489240974080, 36.16307923083526532, -0.6549077602738699877 ) ) ;
#1523 = CARTESIAN_POINT ( 'NONE',  ( -4.629600663469410904, 117.9777096712006852, 0.7347564628851412927 ) ) ;
#1524 = ORIENTED_EDGE ( 'NONE', *, *, #34009, .T. ) ;
#1525 = CARTESIAN_POINT ( 'NONE',  ( -8.041749784432907333, 11.96416136180153345, -2.598976288244244870 ) ) ;
#1526 = CARTESIAN_POINT ( 'NONE',  ( 5.875440716348254711, 118.9244925334023151, -1.017365677016041081 ) ) ;
#1527 = CARTESIAN_POINT ( 'NONE',  ( -2.364009027793917195, 119.4803856251332945, -0.6315868319338824310 ) ) ;
#1528 = CARTESIAN_POINT ( 'NONE',  ( 4.895718167919051567, 117.6590296544187737, 0.9622844256249989403 ) ) ;
#1529 = CARTESIAN_POINT ( 'NONE',  ( -11.37822013471355653, 56.06794068206369275, -5.016499999999995296 ) ) ;
#1530 = CARTESIAN_POINT ( 'NONE',  ( -0.01386859376332154337, 119.8383472832138779, 0.6940411431075991233 ) ) ;
#1531 = CIRCLE ( 'NONE', #25317, 18.13811525448111439 ) ;
#1532 = CARTESIAN_POINT ( 'NONE',  ( -3.234384296441582762, 11.31316835407710819, -3.315160845070126427 ) ) ;
#1533 = CARTESIAN_POINT ( 'NONE',  ( 1.247998466936322838E-15, 12.96302561210691806, 0.000000000000000000 ) ) ;
#1534 = CARTESIAN_POINT ( 'NONE',  ( -26.29578028364076658, 73.87584665086983193, -1.270000000000006013 ) ) ;
#1535 = CARTESIAN_POINT ( 'NONE',  ( 2.317735183313462066, -14.86924938851764999, 5.343245562499194357 ) ) ;
#1536 = CARTESIAN_POINT ( 'NONE',  ( 4.687267571633873864, 120.2198808273567892, -0.2753304537621711900 ) ) ;
#1537 = CARTESIAN_POINT ( 'NONE',  ( -0.2179416487220206811, 33.83400432488151210, 3.531833526404775103 ) ) ;
#1538 = CARTESIAN_POINT ( 'NONE',  ( -0.6554515820231663348, 115.7029491485453150, 1.735612802329033810 ) ) ;
#1539 = ORIENTED_EDGE ( 'NONE', *, *, #17162, .F. ) ;
#1540 = CARTESIAN_POINT ( 'NONE',  ( -3.197619535514014011, 105.1239064336704985, -4.271075346114246329 ) ) ;
#1541 = CARTESIAN_POINT ( 'NONE',  ( 5.270497567351643653, -15.36183412081716604, 0.7307456425073816098 ) ) ;
#1542 = CARTESIAN_POINT ( 'NONE',  ( -19.87863739466945745, 147.4002846799066333, 1.728157425434577510 ) ) ;
#1543 = CARTESIAN_POINT ( 'NONE',  ( -0.2773724154211913984, 24.90860930217742464, 0.9350043038818249830 ) ) ;
#1544 = VERTEX_POINT ( 'NONE', #29261 ) ;
#1545 = CIRCLE ( 'NONE', #9013, 3.683000000000001162 ) ;
#1546 = ORIENTED_EDGE ( 'NONE', *, *, #5800, .T. ) ;
#1547 = PLANE ( 'NONE',  #437 ) ;
#1548 = CARTESIAN_POINT ( 'NONE',  ( 2.900991945634675773, 122.3314979878274045, 0.2533474610292540952 ) ) ;
#1549 =( NAMED_UNIT ( * ) PLANE_ANGLE_UNIT ( ) SI_UNIT ( $, .RADIAN. ) );
#1550 = CARTESIAN_POINT ( 'NONE',  ( -12.65121035427621266, 128.4643691153342218, 0.9906145297030367614 ) ) ;
#1551 = CARTESIAN_POINT ( 'NONE',  ( -12.69999999999999574, 11.53894877578617262, 1.555301434917138235E-15 ) ) ;
#1552 = CARTESIAN_POINT ( 'NONE',  ( 4.562811221412711227, 118.0737936952979794, -0.6153291334979017480 ) ) ;
#1553 = CARTESIAN_POINT ( 'NONE',  ( 9.634306097685872317, 155.2307989660268959, -1.622952429610069247 ) ) ;
#1554 = CARTESIAN_POINT ( 'NONE',  ( -9.074718672963452804, 157.1510513929294177, -1.991881423077542568 ) ) ;
#1555 = DIRECTION ( 'NONE',  ( -5.188838149069471174E-16, 1.699382548006136313E-16, 1.000000000000000000 ) ) ;
#1556 = ORIENTED_EDGE ( 'NONE', *, *, #39881, .F. ) ;
#1557 = CARTESIAN_POINT ( 'NONE',  ( 4.394285435036319853, 118.1841684474106984, -0.4164588777813547638 ) ) ;
#1558 = CARTESIAN_POINT ( 'NONE',  ( 2.776805996813493049, 120.9068798055765370, -0.1259499506852532758 ) ) ;
#1559 = VERTEX_POINT ( 'NONE', #16682 ) ;
#1560 = CARTESIAN_POINT ( 'NONE',  ( 3.216763585201820153, -14.58149021785123978, 2.832987347109013676 ) ) ;
#1561 = CARTESIAN_POINT ( 'NONE',  ( 10.45722248778832508, 56.52709681235301531, -5.016500000000866599 ) ) ;
#1562 = AXIS2_PLACEMENT_3D ( 'NONE', #13972, #19565, #32574 ) ;
#1563 = B_SPLINE_CURVE_WITH_KNOTS ( 'NONE', 3,
 ( #10718, #23699, #40136, #8160, #30110, #11351, #33317, #10515, #17322, #26708 ),
 .UNSPECIFIED., .F., .F.,
 ( 4, 2, 2, 2, 4 ),
 ( -5.999999993416881897E-08, 0.0003259810225990044091, 0.0006520220451979429760, 0.0009780630677968815429, 0.001304104090395820110 ),
 .UNSPECIFIED. ) ;
#1564 = CARTESIAN_POINT ( 'NONE',  ( -58.03077483564787542, 0.4858688437074938915, 1.087158688094367331 ) ) ;
#1565 = EDGE_CURVE ( 'NONE', #17342, #3974, #14232, .T. ) ;
#1566 = CARTESIAN_POINT ( 'NONE',  ( -1.319288878716189828, -8.717950886928733212, 4.428293336331323715 ) ) ;
#1567 = CARTESIAN_POINT ( 'NONE',  ( 16.85437733762575618, 144.1809451582817587, 2.058110026898294365 ) ) ;
#1568 = CARTESIAN_POINT ( 'NONE',  ( -2.299720509168451166, 30.37513842844993306, 3.096482033432269354 ) ) ;
#1569 = CARTESIAN_POINT ( 'NONE',  ( -6.118667329350094164, 121.4157903421748301, 0.08376844782033875114 ) ) ;
#1570 = CARTESIAN_POINT ( 'NONE',  ( 4.586363120317823672, -1.655842793181455663, -0.6244342276643227718 ) ) ;
#1571 = CARTESIAN_POINT ( 'NONE',  ( 2.828086164579441952, 121.0305217392013759, 0.08274239724663745577 ) ) ;
#1572 = CARTESIAN_POINT ( 'NONE',  ( -46.89809204272969367, 25.37679221950173059, 1.718882409580913651 ) ) ;
#1573 = VECTOR ( 'NONE', #21848, 999.9999999999998863 ) ;
#1574 = CARTESIAN_POINT ( 'NONE',  ( -57.95665747882670615, 0.5159457608236717174, -0.4254811051331304217 ) ) ;
#1575 = CARTESIAN_POINT ( 'NONE',  ( 8.792662243298641656, 117.7335494595113943, -0.05956412395685332928 ) ) ;
#1576 = CARTESIAN_POINT ( 'NONE',  ( 0.006734421714204561794, 121.9236798544229003, -0.3370180007450780391 ) ) ;
#1577 = DIRECTION ( 'NONE',  ( -0.8745520943968240202, 0.4849315768086552292, -5.361993529360572958E-16 ) ) ;
#1578 = CARTESIAN_POINT ( 'NONE',  ( -2.178937547604698377, 106.5591908312060667, 4.866054723391081360 ) ) ;
#1579 = CARTESIAN_POINT ( 'NONE',  ( -30.15519950990045572, 69.97033940222175374, 1.269999999999991802 ) ) ;
#1580 = CARTESIAN_POINT ( 'NONE',  ( 8.101632580580826470, 8.064395906452419993, -2.298819013970823999 ) ) ;
#1581 = DIRECTION ( 'NONE',  ( -0.9998501190848635423, -0.01731298258487451447, -5.158639060800523934E-16 ) ) ;
#1582 = CARTESIAN_POINT ( 'NONE',  ( -58.64217253742437208, 0.4108157498741576985, 0.3978973257256460672 ) ) ;
#1583 = CARTESIAN_POINT ( 'NONE',  ( -58.83227707057486811, -0.08366279997995551554, 0.2458995907044889129 ) ) ;
#1584 = CARTESIAN_POINT ( 'NONE',  ( -0.008148259816615344500, 159.5682499516715040, 0.4077722408685187649 ) ) ;
#1585 = ORIENTED_EDGE ( 'NONE', *, *, #14881, .T. ) ;
#1586 = CARTESIAN_POINT ( 'NONE',  ( -57.38748718130355542, 3.645894598607590797, -1.236217348619478962 ) ) ;
#1587 = ORIENTED_EDGE ( 'NONE', *, *, #19393, .F. ) ;
#1588 = CARTESIAN_POINT ( 'NONE',  ( -46.82131867383202461, 20.47688106639290240, -5.000304862135876327 ) ) ;
#1589 = COLOUR_RGB ( '', 0.40784314, 0.44705882, 0.49803922) ;
#1590 = CARTESIAN_POINT ( 'NONE',  ( -13.59117098933512580, 150.2425924485890505, -0.2715839415562138481 ) ) ;
#1591 = CARTESIAN_POINT ( 'NONE',  ( 2.665431962039443992, -15.40910046105366327, 5.814861676232141008 ) ) ;
#1592 = CARTESIAN_POINT ( 'NONE',  ( -6.811759424595843271, 118.6475953829349379, 0.9158128249201543669 ) ) ;
#1593 = AXIS2_PLACEMENT_3D ( 'NONE', #22972, #442, #9584 ) ;
#1594 = CARTESIAN_POINT ( 'NONE',  ( 0.007599820978683539778, 117.2191897141855179, -0.3803261187632671625 ) ) ;
#1595 = CARTESIAN_POINT ( 'NONE',  ( -2.707926769430928804, 11.08828375386998033, -3.745406074561137721 ) ) ;
#1596 = CARTESIAN_POINT ( 'NONE',  ( -4.752142575032330285, 116.8068435238802465, -0.2604826270010437983 ) ) ;
#1597 = CARTESIAN_POINT ( 'NONE',  ( -49.86239633785145742, 16.51455008844218142, -4.953957629277327968 ) ) ;
#1598 = VERTEX_POINT ( 'NONE', #17104 ) ;
#1599 = CARTESIAN_POINT ( 'NONE',  ( 8.798071512540863282, 117.6842349196870572, 0.1758064070670784795 ) ) ;
#1600 = CARTESIAN_POINT ( 'NONE',  ( -8.228482648312640535, 121.2453320564195280, 0.9666412201339350529 ) ) ;
#1601 = CARTESIAN_POINT ( 'NONE',  ( -56.19876127534764265, 4.345455792799514327, -2.342364202820239605 ) ) ;
#1602 = ADVANCED_FACE ( 'NONE', ( #39921 ), #27543, .T. ) ;
#1603 = CARTESIAN_POINT ( 'NONE',  ( 3.289525010481779255, 118.9727644790723531, -0.7721065173366223888 ) ) ;
#1604 = CARTESIAN_POINT ( 'NONE',  ( -1.109551233970537343, 117.7697124030934077, -0.5969493375118321010 ) ) ;
#1605 = CARTESIAN_POINT ( 'NONE',  ( -42.72397600927682504, 22.83316142988638831, -1.683267422954632275 ) ) ;
#1606 = AXIS2_PLACEMENT_3D ( 'NONE', #21223, #5083, #8678 ) ;
#1607 = CARTESIAN_POINT ( 'NONE',  ( 4.453624852893700137, 120.7762672505206041, -0.3811677228292793540 ) ) ;
#1608 = ORIENTED_EDGE ( 'NONE', *, *, #24547, .F. ) ;
#1609 = CARTESIAN_POINT ( 'NONE',  ( -17.79834178490407481, 144.5560955566678558, -2.349204209454022863 ) ) ;
#1610 = CARTESIAN_POINT ( 'NONE',  ( 4.535010020878385895, -15.35856548043400238, 0.06517018677027014428 ) ) ;
#1611 = CARTESIAN_POINT ( 'NONE',  ( -4.374336409094900624, 118.1842338761308753, -0.5915268427067872370 ) ) ;
#1612 = ADVANCED_FACE ( 'NONE', ( #13711 ), #18615, .T. ) ;
#1613 = CARTESIAN_POINT ( 'NONE',  ( -56.26318288983030413, 4.268071985104968213, -2.480832006587858185 ) ) ;
#1614 = CARTESIAN_POINT ( 'NONE',  ( -4.958806897238241085, 117.4102282907815606, 0.9054230299057887121 ) ) ;
#1615 = CARTESIAN_POINT ( 'NONE',  ( 11.01279815837308895, 154.4909003399924643, 2.068435761307119147 ) ) ;
#1616 = DIRECTION ( 'NONE',  ( -1.000000000000000000, -6.353134868986659519E-16, 6.146657985744592735E-16 ) ) ;
#1617 = AXIS2_PLACEMENT_3D ( 'NONE', #36632, #26828, #1065 ) ;
#1618 = CARTESIAN_POINT ( 'NONE',  ( 10.83072783392011651, 157.9016520041087688, 0.1964268902508807535 ) ) ;
#1619 = CARTESIAN_POINT ( 'NONE',  ( -5.777836206968382626, 13.68815862607732825, 6.147148275823971275 ) ) ;
#1620 = CARTESIAN_POINT ( 'NONE',  ( 15.83982646870413191, 146.6055793175013093, 0.7699162700945606508 ) ) ;
#1621 = CARTESIAN_POINT ( 'NONE',  ( -11.56352105402813280, 78.55269139521317356, 1.524000000000000465 ) ) ;
#1622 = ADVANCED_FACE ( 'NONE', ( #20714 ), #3696, .T. ) ;
#1623 = CARTESIAN_POINT ( 'NONE',  ( -42.12253153191132782, 21.94389511927449732, -0.09363185731631336328 ) ) ;
#1624 = CARTESIAN_POINT ( 'NONE',  ( -8.016647455044246584, 121.3928899876477772, -1.222747983602104904 ) ) ;
#1625 = AXIS2_PLACEMENT_3D ( 'NONE', #5659, #18189, #2460 ) ;
#1626 = CARTESIAN_POINT ( 'NONE',  ( -58.32289719230551839, -0.2069853552843642364, 0.1059582036190176574 ) ) ;
#1627 = CARTESIAN_POINT ( 'NONE',  ( -13.64797835309731866, 119.6379125180634446, -0.1726152169769648581 ) ) ;
#1628 = ORIENTED_EDGE ( 'NONE', *, *, #19844, .T. ) ;
#1629 = CARTESIAN_POINT ( 'NONE',  ( -46.93527007713159804, 25.91000514300129254, -0.2210822239326209193 ) ) ;
#1630 = CARTESIAN_POINT ( 'NONE',  ( 6.874218592591693877, 121.5427147135433046, -0.4735844615521632717 ) ) ;
#1631 = CARTESIAN_POINT ( 'NONE',  ( -8.366466113708746377, 119.9145198431060777, 1.112176479753330227 ) ) ;
#1632 = CIRCLE ( 'NONE', #4390, 0.7620000000000015650 ) ;
#1633 = ORIENTED_EDGE ( 'NONE', *, *, #10977, .F. ) ;
#1634 = CARTESIAN_POINT ( 'NONE',  ( 0.5927366764262057552, 115.7030772134404799, -1.739505766195229564 ) ) ;
#1635 = CARTESIAN_POINT ( 'NONE',  ( -9.155891339183989786, 123.9989874199980022, -0.4132670667758963079 ) ) ;
#1636 = CARTESIAN_POINT ( 'NONE',  ( 4.246535372682106235, -13.89508586689386327, 4.277860383763752772 ) ) ;
#1637 = CARTESIAN_POINT ( 'NONE',  ( -14.33513709642007861, 121.5541609676003389, 0.9327927267376099341 ) ) ;
#1638 = LINE ( 'NONE', #34216, #5021 ) ;
#1639 = CARTESIAN_POINT ( 'NONE',  ( 22.65355654554102216, 150.6414900647796173, 0.6056372710714960084 ) ) ;
#1640 = CARTESIAN_POINT ( 'NONE',  ( 9.499210638188102962, 124.7903824246305362, 0.2360490693302050025 ) ) ;
#1641 = ORIENTED_EDGE ( 'NONE', *, *, #10958, .F. ) ;
#1642 = CARTESIAN_POINT ( 'NONE',  ( 0.7259983000635549244, 26.63096242550804860, 0.6518668477890779966 ) ) ;
#1643 = EDGE_CURVE ( 'NONE', #39553, #22515, #28148, .T. ) ;
#1644 = CARTESIAN_POINT ( 'NONE',  ( -15.19377495473410811, 156.0906695176550443, -0.3258312939631710647 ) ) ;
#1645 = CARTESIAN_POINT ( 'NONE',  ( -44.11963993135361051, 21.57970632322487958, -2.906001689204277927 ) ) ;
#1646 = DIRECTION ( 'NONE',  ( -0.9998004120163609398, -4.016384292689130894E-17, -0.01997839162482749689 ) ) ;
#1647 = ORIENTED_EDGE ( 'NONE', *, *, #28787, .T. ) ;
#1648 = CARTESIAN_POINT ( 'NONE',  ( 8.481912912939511884, 119.1148186440260588, 1.316834002904183620 ) ) ;
#1649 = CARTESIAN_POINT ( 'NONE',  ( -6.422645615570758970, 77.88548590848095898, 1.524000000000002908 ) ) ;
#1650 = CARTESIAN_POINT ( 'NONE',  ( 20.53318969041745490, 136.3738900553462372, 2.061127768630951707 ) ) ;
#1651 = CARTESIAN_POINT ( 'NONE',  ( -55.98935619762070104, 5.304184903340836144, -2.807757416349843549 ) ) ;
#1652 = CARTESIAN_POINT ( 'NONE',  ( 9.147047865982747439, 157.1510513929294177, -1.627767162235162379 ) ) ;
#1653 = CIRCLE ( 'NONE', #9766, 9.048750000000000071 ) ;
#1654 = CARTESIAN_POINT ( 'NONE',  ( -8.398906084147393258, 18.04027321918359306, -0.8732425085428288103 ) ) ;
#1655 = CARTESIAN_POINT ( 'NONE',  ( -9.442718531279867378, 118.5748184150550060, -1.042386753229704865 ) ) ;
#1656 = CARTESIAN_POINT ( 'NONE',  ( 4.935068106205077854, 117.6551405386727538, -0.7499101476925047471 ) ) ;
#1657 = ORIENTED_EDGE ( 'NONE', *, *, #41794, .F. ) ;
#1658 = CARTESIAN_POINT ( 'NONE',  ( -13.63867282259138669, 150.2122286517991085, 0.04772847129159333429 ) ) ;
#1659 = CARTESIAN_POINT ( 'NONE',  ( 3.586901592285024698, -15.56753269123677086, 5.192771612050266050 ) ) ;
#1660 = CARTESIAN_POINT ( 'NONE',  ( -6.263959367015712765, 28.84083519579221999, 0.1566845698765544637 ) ) ;
#1661 = CIRCLE ( 'NONE', #9133, 3.175000000000001155 ) ;
#1662 = CARTESIAN_POINT ( 'NONE',  ( -0.1787238347214931966, 117.9496057287605595, -1.408787723444971274 ) ) ;
#1663 = ORIENTED_EDGE ( 'NONE', *, *, #4742, .F. ) ;
#1664 = CARTESIAN_POINT ( 'NONE',  ( 7.562035183886194112, 119.9600249249614592, 1.380075063195379315 ) ) ;
#1665 = DIRECTION ( 'NONE',  ( -0.4849315768086535083, -0.8745520943968250194, -1.030032898892974695E-16 ) ) ;
#1666 = AXIS2_PLACEMENT_3D ( 'NONE', #32390, #6830, #3222 ) ;
#1667 = FACE_OUTER_BOUND ( 'NONE', #41630, .T. ) ;
#1668 = CARTESIAN_POINT ( 'NONE',  ( -1.918777129854518870, 121.7602717223048501, 0.2400857948923555418 ) ) ;
#1669 = CARTESIAN_POINT ( 'NONE',  ( 8.395564333921381461, 13.51935342844394583, -0.6424836208785561498 ) ) ;
#1670 = CARTESIAN_POINT ( 'NONE',  ( 9.559621201325379403, 153.9312916436033447, 1.179784447169990980 ) ) ;
#1671 = CARTESIAN_POINT ( 'NONE',  ( -4.782995773917860127, 118.5930653697794384, -0.9660711341386800655 ) ) ;
#1672 = ADVANCED_FACE ( 'NONE', ( #40343 ), #3935, .T. ) ;
#1673 = CARTESIAN_POINT ( 'NONE',  ( 3.228502273016993218, 159.4348965051207756, -0.3922148187338911351 ) ) ;
#1674 = CARTESIAN_POINT ( 'NONE',  ( 4.886022116125724679, 117.7561648045584519, -0.7145573245312663024 ) ) ;
#1675 = AXIS2_PLACEMENT_3D ( 'NONE', #6302, #35478, #19903 ) ;
#1676 = CARTESIAN_POINT ( 'NONE',  ( -57.32388393874000343, 1.962507715601113034, 1.551164999238653142 ) ) ;
#1677 = CARTESIAN_POINT ( 'NONE',  ( -56.40362312693983426, 4.444843175407298119, 2.562861284854979882 ) ) ;
#1678 = CARTESIAN_POINT ( 'NONE',  ( -5.078986093043186045, 85.69146620154573668, -0.1014902294541237954 ) ) ;
#1679 = CARTESIAN_POINT ( 'NONE',  ( -4.160016578962718370, 118.2392577574570112, 0.2314449875878247520 ) ) ;
#1680 = CARTESIAN_POINT ( 'NONE',  ( 4.429857153230104316, 111.0465000998802907, -3.038205857650542630 ) ) ;
#1681 = EDGE_LOOP ( 'NONE', ( #10008, #19257, #555, #25784 ) ) ;
#1682 = EDGE_CURVE ( 'NONE', #27418, #37655, #29897, .T. ) ;
#1683 = CARTESIAN_POINT ( 'NONE',  ( -50.58884987432006852, 15.93229845861179861, 5.010371253631904942 ) ) ;
#1684 =( BOUNDED_CURVE ( )  B_SPLINE_CURVE ( 3, ( #14501, #27516, #36903, #30914 ),
 .UNSPECIFIED., .F., .T. ) 
 B_SPLINE_CURVE_WITH_KNOTS ( ( 4, 4 ),
 ( 0.01144530851284876125, 0.09183118002780921163 ),
 .UNSPECIFIED. ) 
 CURVE ( )  GEOMETRIC_REPRESENTATION_ITEM ( )  RATIONAL_B_SPLINE_CURVE ( ( 0.9552667266446379646, 0.8529924504886332581, 0.7679498765706652685, 0.7001390048907338848 ) ) 
 REPRESENTATION_ITEM ( '' )  );
#1685 = CARTESIAN_POINT ( 'NONE',  ( -4.183512250370689856, 119.3195231512375898, -0.9266158876289375401 ) ) ;
#1686 = CARTESIAN_POINT ( 'NONE',  ( -5.281229466409689266, 116.7000894413872629, -1.021210189368793264 ) ) ;
#1687 = CARTESIAN_POINT ( 'NONE',  ( 4.433936586972705207, 118.1614370034927646, 0.6150725568094654871 ) ) ;
#1688 = CARTESIAN_POINT ( 'NONE',  ( -15.91132205781029008, 147.3275361421020193, -1.167720536598260805 ) ) ;
#1689 = DIRECTION ( 'NONE',  ( -1.000000000000000000, 1.011795553208986254E-16, 0.000000000000000000 ) ) ;
#1690 = VERTEX_POINT ( 'NONE', #36715 ) ;
#1691 = CARTESIAN_POINT ( 'NONE',  ( -0.8080508600641240768, 24.25718022715097888, 4.550674767031389401 ) ) ;
#1692 = CARTESIAN_POINT ( 'NONE',  ( -14.37089176232999321, 134.5679602169015254, -1.683180344383908178 ) ) ;
#1693 = DIRECTION ( 'NONE',  ( -0.8745520943968246863, 0.4849315768086538414, -5.122214988120500191E-16 ) ) ;
#1694 = CARTESIAN_POINT ( 'NONE',  ( -44.81960200544693151, 21.09415034428922908, 3.442746975522605002 ) ) ;
#1695 = CARTESIAN_POINT ( 'NONE',  ( -6.075447103849212382, 121.3874205645395961, 0.1528716657061620909 ) ) ;
#1696 = ADVANCED_FACE ( 'NONE', ( #11137 ), #26704, .T. ) ;
#1697 = DIRECTION ( 'NONE',  ( -0.8745520943968301264, 0.4849315768086440159, -5.271987356194192020E-16 ) ) ;
#1698 = CARTESIAN_POINT ( 'NONE',  ( 22.16805208646083258, 150.4821223471089411, 1.513879355785526570 ) ) ;
#1699 = DIRECTION ( 'NONE',  ( 0.1469470846586743706, 0.000000000000000000, 0.9891443546370348727 ) ) ;
#1701 = CARTESIAN_POINT ( 'NONE',  ( 10.77577921906383374, 119.6772744462923157, -0.9367561965627279053 ) ) ;
#1700 = CARTESIAN_POINT ( 'NONE',  ( 3.212496809824684441, -14.25148094350509353, 2.370051959060230473 ) ) ;
#1702 = CARTESIAN_POINT ( 'NONE',  ( -18.70798771669560523, 146.9271955717142930, 1.702497825003243648 ) ) ;
#1703 = CARTESIAN_POINT ( 'NONE',  ( 0.8685042297821888857, -7.415843212509670934, 0.4410767154842855642 ) ) ;
#1704 = CARTESIAN_POINT ( 'NONE',  ( -3.814135102937820321, 116.8938343318378088, -0.4443717020561034903 ) ) ;
#1705 = ADVANCED_FACE ( 'NONE', ( #7327 ), #7648, .T. ) ;
#1706 = CARTESIAN_POINT ( 'NONE',  ( 0.7683055643446228267, 21.07255974867073078, 0.6014680952941496850 ) ) ;
#1707 = ORIENTED_EDGE ( 'NONE', *, *, #6569, .T. ) ;
#1708 = CARTESIAN_POINT ( 'NONE',  ( -47.79679003974130325, 17.22715854250130718, 2.282645788202369186 ) ) ;
#1709 = CARTESIAN_POINT ( 'NONE',  ( -0.7006168245644571746, 156.3636429644085695, 0.4970284052464097324 ) ) ;
#1710 = CARTESIAN_POINT ( 'NONE',  ( 4.667506617707346983, -11.86120359225895093, 0.9697133514482669803 ) ) ;
#1711 = CARTESIAN_POINT ( 'NONE',  ( 10.54966536967459234, 123.3532649940754027, -0.9932924318631478622 ) ) ;
#1712 = VERTEX_POINT ( 'NONE', #36305 ) ;
#1713 = CARTESIAN_POINT ( 'NONE',  ( 0.4623142775939118598, 115.7034744490966602, 1.762871263781926601 ) ) ;
#1714 = CARTESIAN_POINT ( 'NONE',  ( 2.715444768400132158, -14.72438443971033095, 4.720152092698882029 ) ) ;
#1715 = CARTESIAN_POINT ( 'NONE',  ( -4.887146391587018357, 117.6636767201053289, -0.9828159811524803668 ) ) ;
#1716 = CARTESIAN_POINT ( 'NONE',  ( 7.047330174099000644, 122.0696255612902519, 0.06645725506650276837 ) ) ;
#1717 = EDGE_CURVE ( 'NONE', #31005, #40327, #26908, .T. ) ;
#1718 = EDGE_LOOP ( 'NONE', ( #13114, #32605, #28225, #34544 ) ) ;
#1719 = CARTESIAN_POINT ( 'NONE',  ( 17.72814975036767038, 131.6735282812448986, 2.269257323068798904 ) ) ;
#1720 = CYLINDRICAL_SURFACE ( 'NONE', #30618, 3.175000000000001155 ) ;
#1721 = CARTESIAN_POINT ( 'NONE',  ( 0.01596947694123658501, 156.4635559983122448, -0.7991779281049287142 ) ) ;
#1722 = CARTESIAN_POINT ( 'NONE',  ( 21.48671512862179611, 132.5742979909900328, 0.1330572995313749063 ) ) ;
#1723 = CARTESIAN_POINT ( 'NONE',  ( -6.654617103318593247E-14, 104.6144662015457243, 1.534725424433578570E-31 ) ) ;
#1724 = CARTESIAN_POINT ( 'NONE',  ( 1.989242623267584165, -15.37180843082167137, 6.016017301631105596 ) ) ;
#1725 = FACE_OUTER_BOUND ( 'NONE', #7264, .T. ) ;
#1726 = CARTESIAN_POINT ( 'NONE',  ( -0.7387659178326329013, 32.94979111317254450, 0.8178967711910589689 ) ) ;
#1727 = ADVANCED_FACE ( 'NONE', ( #1152 ), #40132, .T. ) ;
#1728 = CARTESIAN_POINT ( 'NONE',  ( -4.711805129293004768, 117.9616559148864781, 0.6918731007553912127 ) ) ;
#1729 = VERTEX_POINT ( 'NONE', #7748 ) ;
#1730 = EDGE_LOOP ( 'NONE', ( #36348, #16513, #29077, #41244 ) ) ;
#1731 = CARTESIAN_POINT ( 'NONE',  ( 5.274109024393328404, 115.7029491485453150, -0.8140283081321303404 ) ) ;
#1732 = CARTESIAN_POINT ( 'NONE',  ( 5.647724574261765440, 118.2795828492321704, -0.9363071186805449475 ) ) ;
#1733 = CARTESIAN_POINT ( 'NONE',  ( -2.266726881631651036, 118.5759350612125900, -0.8281820106640958024 ) ) ;
#1734 = CARTESIAN_POINT ( 'NONE',  ( 4.723834500974907868, 117.6625160859792487, 1.132072396740811060 ) ) ;
#1735 = DIRECTION ( 'NONE',  ( -1.000000000000000000, 0.000000000000000000, -6.146657985744586818E-16 ) ) ;
#1736 = CARTESIAN_POINT ( 'NONE',  ( -0.3766127027002308947, 114.7739974199301116, 2.035987775551920009 ) ) ;
#1737 = CARTESIAN_POINT ( 'NONE',  ( 1.616848224653315569, 9.589005055319924864, -4.350374724214612243 ) ) ;
#1738 = CARTESIAN_POINT ( 'NONE',  ( 4.980372089298493954, 117.4083386159582005, -0.8694277117261164367 ) ) ;
#1739 = CARTESIAN_POINT ( 'NONE',  ( -1.217761333252803224, 106.0671965372247740, -5.195771519815528094 ) ) ;
#1740 = CARTESIAN_POINT ( 'NONE',  ( 1.928300050954173450, -15.05328954375542772, 5.649432967411273765 ) ) ;
#1741 = CARTESIAN_POINT ( 'NONE',  ( 5.461839458676641001, 117.5340897209903517, -0.6076615112082688341 ) ) ;
#1742 = CARTESIAN_POINT ( 'NONE',  ( -2.296080426531199592, 33.88561480753556765, 4.023271960718671991 ) ) ;
#1743 = CARTESIAN_POINT ( 'NONE',  ( -0.5727016603203397560, 115.7031860021946557, 1.740666313404392485 ) ) ;
#1744 = CARTESIAN_POINT ( 'NONE',  ( -1.932895124392534303, 20.38400505531995321, -4.219463811995566083 ) ) ;
#1745 = VERTEX_POINT ( 'NONE', #40754 ) ;
#1746 = CARTESIAN_POINT ( 'NONE',  ( -4.843412999271194508, 105.1215046380817029, -2.263786507608671617 ) ) ;
#1747 = CARTESIAN_POINT ( 'NONE',  ( 3.827285340041869155, -15.59443631323044421, 3.224486442507772388 ) ) ;
#1748 = CARTESIAN_POINT ( 'NONE',  ( -0.4802819474809040812, 118.7114656741295988, 0.5981741851633315399 ) ) ;
#1749 = EDGE_CURVE ( 'NONE', #19747, #35348, #13067, .T. ) ;
#1750 = CARTESIAN_POINT ( 'NONE',  ( 0.5005776846888100318, 19.73258526448893591, -0.8400667230076528380 ) ) ;
#1751 = ORIENTED_EDGE ( 'NONE', *, *, #28742, .F. ) ;
#1752 = ORIENTED_EDGE ( 'NONE', *, *, #36346, .F. ) ;
#1753 = DIRECTION ( 'NONE',  ( -0.3582377630123937395, 0.9336303900108844367, -1.442042072394378310E-15 ) ) ;
#1754 = CARTESIAN_POINT ( 'NONE',  ( 4.252685754339869284, 122.9893884486272526, 0.2003490066864924701 ) ) ;
#1755 = FILL_AREA_STYLE_COLOUR ( '', #18907 ) ;
#1756 = CARTESIAN_POINT ( 'NONE',  ( -8.590326429123278373, 154.7538831414287870, 1.096848044820072143 ) ) ;
#1757 = CARTESIAN_POINT ( 'NONE',  ( -42.67774669360623108, 22.12976309729135593, 1.921043817380094332 ) ) ;
#1758 = CARTESIAN_POINT ( 'NONE',  ( 4.705771658150993630, 117.9790676909462661, -0.6572654973250883215 ) ) ;
#1759 = CARTESIAN_POINT ( 'NONE',  ( 5.624295920984120123, 156.7050554705274408, -1.628980406729419128 ) ) ;
#1760 = CARTESIAN_POINT ( 'NONE',  ( -14.15513794057049779, 123.4894365733723447, -1.873888081047781595 ) ) ;
#1761 = DIRECTION ( 'NONE',  ( -0.6294287539884059202, -0.7770581983690814099, -1.945484789722797322E-16 ) ) ;
#1762 = ORIENTED_EDGE ( 'NONE', *, *, #691, .F. ) ;
#1763 = CARTESIAN_POINT ( 'NONE',  ( 4.171966789054940783, 118.2392508536157862, -0.2176385797143781942 ) ) ;
#1764 = CARTESIAN_POINT ( 'NONE',  ( 8.223969002016808361, 122.7966848691156514, -0.2142357769474920459 ) ) ;
#1765 = ORIENTED_EDGE ( 'NONE', *, *, #33196, .F. ) ;
#1766 = CARTESIAN_POINT ( 'NONE',  ( 3.178324225997528618, -14.33742748831649827, 1.935164598152447679 ) ) ;
#1767 = CARTESIAN_POINT ( 'NONE',  ( 4.972946268020358218, 117.3993836135847033, 0.9764272678749694734 ) ) ;
#1768 = CARTESIAN_POINT ( 'NONE',  ( -58.07568876781240164, 0.3868594689447146795, 1.028118745743028084 ) ) ;
#1769 = AXIS2_PLACEMENT_3D ( 'NONE', #10155, #36381, #23767 ) ;
#1770 = CARTESIAN_POINT ( 'NONE',  ( 3.951836011467571907, -5.044640503713330837, -2.394960105287299523 ) ) ;
#1771 = CARTESIAN_POINT ( 'NONE',  ( 17.23725050067783471, 146.8699245690979751, 2.055247338431126725 ) ) ;
#1772 = CARTESIAN_POINT ( 'NONE',  ( -3.055152424816264478, 29.15171311842127011, 2.103066797612082262 ) ) ;
#1773 = CARTESIAN_POINT ( 'NONE',  ( -4.073291749555337127, 117.6466181296975151, 0.7504383534773491071 ) ) ;
#1774 = CARTESIAN_POINT ( 'NONE',  ( -4.637963820743935983, -6.603494994175692412, 0.1710436084038768345 ) ) ;
#1775 = CARTESIAN_POINT ( 'NONE',  ( 4.232597188052644732, 155.8470599587123502, 0.1762653075193724439 ) ) ;
#1776 = CARTESIAN_POINT ( 'NONE',  ( 8.344183819546742598, 4.025392264050483782, -1.191670311180863528 ) ) ;
#1777 = CARTESIAN_POINT ( 'NONE',  ( -57.24575050778504703, 1.871741192705528301, -0.5496743666259116257 ) ) ;
#1778 = CARTESIAN_POINT ( 'NONE',  ( -2.140641356428172770, 116.4937786673416866, -0.3810182028649428676 ) ) ;
#1779 =( REPRESENTATION_RELATIONSHIP ('NONE','NONE', #30767, #19076 ) REPRESENTATION_RELATIONSHIP_WITH_TRANSFORMATION ( #17242 )SHAPE_REPRESENTATION_RELATIONSHIP( ) );
#1780 = DIRECTION ( 'NONE',  ( 0.9807655518882886225, -0.1951894777626621558, 5.420735302995426205E-16 ) ) ;
#1781 = DIRECTION ( 'NONE',  ( 5.188838149069472160E-16, -1.699382548006136559E-16, -1.000000000000000000 ) ) ;
#1782 = CARTESIAN_POINT ( 'NONE',  ( -7.994219716368544226, 68.36415334912796027, 1.270000000000003570 ) ) ;
#1783 = DIRECTION ( 'NONE',  ( -0.8745520943968241312, 0.4849315768086548406, -5.691349986800536046E-16 ) ) ;
#1784 = CARTESIAN_POINT ( 'NONE',  ( 7.466160517099046601, -1.205741384250370363, -3.973931221679563919 ) ) ;
#1785 = CARTESIAN_POINT ( 'NONE',  ( 3.314101028046484210, 118.1588881422629242, 0.7891393284369173644 ) ) ;
#1786 = CARTESIAN_POINT ( 'NONE',  ( -7.868930244179279221, 69.75330307926518003, 1.270000000000003348 ) ) ;
#1787 = CARTESIAN_POINT ( 'NONE',  ( 4.792324638223571576, 56.51998046905274009, -4.972049999999996750 ) ) ;
#1788 = CARTESIAN_POINT ( 'NONE',  ( 0.1041500444719085511, 106.1822392402443143, -5.212094112990285133 ) ) ;
#1789 = CARTESIAN_POINT ( 'NONE',  ( -10.70371904046275979, 157.9381250348597234, 0.2505172755855811784 ) ) ;
#1790 = VERTEX_POINT ( 'NONE', #28383 ) ;
#1791 = CARTESIAN_POINT ( 'NONE',  ( -58.55612285180487930, 0.6590214021355705887, -0.05016670522519821318 ) ) ;
#1792 = ORIENTED_EDGE ( 'NONE', *, *, #37372, .F. ) ;
#1793 = CARTESIAN_POINT ( 'NONE',  ( -44.83891394770831340, 21.39113109692858217, -3.507332325250104965 ) ) ;
#1794 = CARTESIAN_POINT ( 'NONE',  ( -1.624513285529166184, 120.9965111687125159, 0.001083860100774148216 ) ) ;
#1795 = CARTESIAN_POINT ( 'NONE',  ( 5.341109902925343711, -14.98078892696824660, 3.412803344283087181 ) ) ;
#1796 = CARTESIAN_POINT ( 'NONE',  ( -0.01081828485867829433, 118.1092738308834669, 0.5413912121690740431 ) ) ;
#1797 = CARTESIAN_POINT ( 'NONE',  ( 4.883164212476692967, 117.4312795728108227, -0.5545796311387335420 ) ) ;
#1798 = CARTESIAN_POINT ( 'NONE',  ( 4.419457123578296454, 17.78516144714274105, -1.360477052881604143 ) ) ;
#1799 = CARTESIAN_POINT ( 'NONE',  ( -16.90643861817993354, 122.6916909566506320, -0.7822879649369940402 ) ) ;
#1800 = CARTESIAN_POINT ( 'NONE',  ( -51.28922332432183140, 14.16478490540409219, -4.617129769900083502 ) ) ;
#1801 = ORIENTED_EDGE ( 'NONE', *, *, #16774, .F. ) ;
#1802 = AXIS2_PLACEMENT_3D ( 'NONE', #31412, #41438, #15845 ) ;
#1803 = CARTESIAN_POINT ( 'NONE',  ( -5.563982112966385785, 116.7029361893387431, -0.03558650952807581452 ) ) ;
#1804 = DIRECTION ( 'NONE',  ( 0.9998501190848635423, 0.01731298258487451447, 5.158639060800523934E-16 ) ) ;
#1805 = CARTESIAN_POINT ( 'NONE',  ( -9.157854976475398701, 121.7740273863187923, 1.020316602444926835 ) ) ;
#1806 = CARTESIAN_POINT ( 'NONE',  ( -49.36007427823454918, 17.22477551487747149, -4.982732351148011496 ) ) ;
#1807 = CARTESIAN_POINT ( 'NONE',  ( 12.53898343483645483, 122.9501582372872406, -1.331292802868025316 ) ) ;
#1808 = CARTESIAN_POINT ( 'NONE',  ( -4.913347341789825684, 118.0342071775839941, -0.9606804153092147747 ) ) ;
#1809 = CARTESIAN_POINT ( 'NONE',  ( -48.56815661899837977, 19.24492339269602681, -5.224590812749990931 ) ) ;
#1810 = CARTESIAN_POINT ( 'NONE',  ( 0.7306116569919257620, 156.4221767039705071, -0.6844267650493706112 ) ) ;
#1811 = VERTEX_POINT ( 'NONE', #24333 ) ;
#1812 = CARTESIAN_POINT ( 'NONE',  ( -16.01586142131302637, 150.9843922791743296, -2.313278988710850470 ) ) ;
#1813 = CARTESIAN_POINT ( 'NONE',  ( 3.179180861052679052, -15.64967171142420099, 4.365151252316144870 ) ) ;
#1814 = CARTESIAN_POINT ( 'NONE',  ( -4.340471936078397874, 118.1815412487432866, -0.6239179087215906971 ) ) ;
#1815 = CARTESIAN_POINT ( 'NONE',  ( -57.29531047346088712, 2.067549486662559222, -1.749273462387503031 ) ) ;
#1816 = LINE ( 'NONE', #30764, #8889 ) ;
#1817 = CARTESIAN_POINT ( 'NONE',  ( 11.24613893767475581, 123.2561760277034324, 1.620791190024705175 ) ) ;
#1818 = CARTESIAN_POINT ( 'NONE',  ( -5.924740142096584172, 65.21691166894066782, -1.269999999999994023 ) ) ;
#1819 = CARTESIAN_POINT ( 'NONE',  ( -5.224212249200172131, -8.128124378088662283, -6.605211778952579493 ) ) ;
#1820 = CARTESIAN_POINT ( 'NONE',  ( 15.89661694251502233, 145.9828583539951126, 0.9138632209041560595 ) ) ;
#1821 = CARTESIAN_POINT ( 'NONE',  ( -57.52317756609133426, 3.014644041894651405, -1.981665235817958948 ) ) ;
#1822 = AXIS2_PLACEMENT_3D ( 'NONE', #36149, #6534, #19301 ) ;
#1824 = VERTEX_POINT ( 'NONE', #11551 ) ;
#1823 = CARTESIAN_POINT ( 'NONE',  ( -44.02811856515548783, 21.20684991433588351, -2.650346054289419495 ) ) ;
#1825 = CARTESIAN_POINT ( 'NONE',  ( -2.017383181376497969, 117.3993839202099849, 1.370540161117654421 ) ) ;
#1826 = FACE_OUTER_BOUND ( 'NONE', #41958, .T. ) ;
#1827 = CARTESIAN_POINT ( 'NONE',  ( -58.37241122568488549, -0.2962816677227891882, -1.036115889661433750E-14 ) ) ;
#1828 = CARTESIAN_POINT ( 'NONE',  ( -51.10637697011796377, 21.44594517096482633, -9.676659029908143380E-15 ) ) ;
#1829 = CARTESIAN_POINT ( 'NONE',  ( -4.745947329130700609, 116.7839080817633430, 0.02307940527355903035 ) ) ;
#1830 = ORIENTED_EDGE ( 'NONE', *, *, #17540, .F. ) ;
#1831 = CARTESIAN_POINT ( 'NONE',  ( -47.66286930719411430, 20.62480072838431155, -5.054501799269508489 ) ) ;
#1832 = CARTESIAN_POINT ( 'NONE',  ( -7.899188505988096409, 121.9926928506463355, -0.9456170989852971109 ) ) ;
#1833 = DIRECTION ( 'NONE',  ( -0.000000000000000000, -0.000000000000000000, -1.000000000000000000 ) ) ;
#1834 = ORIENTED_EDGE ( 'NONE', *, *, #16784, .F. ) ;
#1835 = CARTESIAN_POINT ( 'NONE',  ( 4.758501140356155901, 118.7629491485453741, -0.8044719740567526367 ) ) ;
#1836 = CARTESIAN_POINT ( 'NONE',  ( -11.87576104716911907, 151.9737369308441544, -0.5463127210923325316 ) ) ;
#1837 = CARTESIAN_POINT ( 'NONE',  ( 2.069070256058832324, -15.20480250118845511, 5.930115229603830862 ) ) ;
#1838 = CARTESIAN_POINT ( 'NONE',  ( -3.003295232750944344, 159.1263692740743068, 1.093010787580665832 ) ) ;
#1839 = AXIS2_PLACEMENT_3D ( 'NONE', #27524, #17706, #30706 ) ;
#1840 = DIRECTION ( 'NONE',  ( -0.9998004120163608288, 0.000000000000000000, -0.01997839162482749342 ) ) ;
#1841 = CARTESIAN_POINT ( 'NONE',  ( 13.64397932274287584, 119.6379125180634446, 0.3727430486357818928 ) ) ;
#1842 = CARTESIAN_POINT ( 'NONE',  ( 8.025551358755512510, 122.8503416937399351, 0.2015751188716342623 ) ) ;
#1843 = CARTESIAN_POINT ( 'NONE',  ( -5.005799711115156647, 117.5941877228957537, 0.5449465340951143988 ) ) ;
#1844 = CARTESIAN_POINT ( 'NONE',  ( -0.2409191691226134635, 30.52881386638012629, -0.9476172785465332149 ) ) ;
#1845 = CARTESIAN_POINT ( 'NONE',  ( -8.213135470206685440, 117.5064756823292385, -0.2531991783344218483 ) ) ;
#1846 = DIRECTION ( 'NONE',  ( -4.017660918040594346E-17, 1.000000000000000000, 2.376309959284834438E-19 ) ) ;
#1847 = ORIENTED_EDGE ( 'NONE', *, *, #4341, .T. ) ;
#1848 = DIRECTION ( 'NONE',  ( -1.000000000000000000, -5.463695987328526437E-16, 0.000000000000000000 ) ) ;
#1849 = EDGE_LOOP ( 'NONE', ( #16707, #10753, #3320, #6175 ) ) ;
#1850 = CARTESIAN_POINT ( 'NONE',  ( -5.969389315549677555, 118.6093026330748614, 0.9569931481840777687 ) ) ;
#1851 = DIRECTION ( 'NONE',  ( -5.188838149069472160E-16, 1.699382548006136559E-16, 1.000000000000000000 ) ) ;
#1852 = CARTESIAN_POINT ( 'NONE',  ( 3.006067730437935293, 117.5448765310053005, 0.7098943453401750370 ) ) ;
#1853 = CARTESIAN_POINT ( 'NONE',  ( -58.63691926683795685, -0.7730888055834101991, -0.03927874230347657564 ) ) ;
#1854 = AXIS2_PLACEMENT_3D ( 'NONE', #40634, #8669, #34449 ) ;
#1855 = CARTESIAN_POINT ( 'NONE',  ( 18.89434961005710534, 135.8679125664981484, -1.636908753694952257 ) ) ;
#1856 = CARTESIAN_POINT ( 'NONE',  ( -8.392384909494198908, 27.87760190725155951, 0.4359655409547527616 ) ) ;
#1857 = CARTESIAN_POINT ( 'NONE',  ( -1.008854969157164216, 117.0751458430253393, -0.4193480094219990129 ) ) ;
#1858 = CARTESIAN_POINT ( 'NONE',  ( 4.919889287388610200, 117.6395836675350353, -0.8280294640748854240 ) ) ;
#1859 = VERTEX_POINT ( 'NONE', #31361 ) ;
#1860 = CIRCLE ( 'NONE', #30417, 0.2540000000000013358 ) ;
#1861 = CARTESIAN_POINT ( 'NONE',  ( -9.105893302116724541, 123.9936668703698075, -0.02250835519154683814 ) ) ;
#1862 = CARTESIAN_POINT ( 'NONE',  ( -12.39214084994788756, 122.8403290575659526, -1.822206477283890624 ) ) ;
#1863 = CARTESIAN_POINT ( 'NONE',  ( 6.169188725349925129, -14.24425063093240418, 1.535968726618487379 ) ) ;
#1864 = DIRECTION ( 'NONE',  ( 0.9998004120163608288, 0.000000000000000000, 0.01997839162482749342 ) ) ;
#1865 = CARTESIAN_POINT ( 'NONE',  ( -1.567216851204632500, 117.9496054947997692, -1.374611063050779514 ) ) ;
#1866 = EDGE_LOOP ( 'NONE', ( #30676, #16869 ) ) ;
#1867 = CARTESIAN_POINT ( 'NONE',  ( 19.09005709338556400, 148.2829752965438956, 2.500029303593213736 ) ) ;
#1868 = DIRECTION ( 'NONE',  ( 0.9454731675810352787, -0.3256999990547799206, 8.013021739297562628E-15 ) ) ;
#1869 = CARTESIAN_POINT ( 'NONE',  ( 18.00660244842765323, 1.647546923381499288E-15, 2.205172805198582110E-15 ) ) ;
#1870 = CIRCLE ( 'NONE', #37222, 1.905000000000007354 ) ;
#1871 = CARTESIAN_POINT ( 'NONE',  ( -2.328636301501583628, 124.8000875644994068, -0.03907356579384855394 ) ) ;
#1872 = CARTESIAN_POINT ( 'NONE',  ( -6.911983299595774177, -11.51556667111630894, -4.837919318831837678 ) ) ;
#1873 = CARTESIAN_POINT ( 'NONE',  ( 11.86571527151339822, 128.3619849303985632, 1.073981288313974991 ) ) ;
#1874 = DIRECTION ( 'NONE',  ( -0.000000000000000000, -0.000000000000000000, -1.000000000000000000 ) ) ;
#1875 = CARTESIAN_POINT ( 'NONE',  ( 20.43054131464308298, 152.5480347002736607, -0.4178791510274245113 ) ) ;
#1876 = CARTESIAN_POINT ( 'NONE',  ( 6.059261036834405978, 56.51500000000000057, -5.016500000000000625 ) ) ;
#1877 = CARTESIAN_POINT ( 'NONE',  ( -58.30132030250355513, -0.1468297825097129305, 0.3337338984326744251 ) ) ;
#1878 = PRESENTATION_STYLE_ASSIGNMENT (( #30622 ) ) ;
#1879 = CARTESIAN_POINT ( 'NONE',  ( 1.824656174747253168, -15.25388738520313225, 5.420764384989097628 ) ) ;
#1880 = CARTESIAN_POINT ( 'NONE',  ( -4.117142285576561811, 118.2429491485453354, 0.1876306250578462509 ) ) ;
#1881 = CARTESIAN_POINT ( 'NONE',  ( -11.74288454345109756, 118.7273140689154616, -0.2346507796901759202 ) ) ;
#1882 = AXIS2_PLACEMENT_3D ( 'NONE', #15387, #11358, #24546 ) ;
#1883 = VERTEX_POINT ( 'NONE', #18570 ) ;
#1884 = CARTESIAN_POINT ( 'NONE',  ( -52.26939619200407350, 13.58078015197115818, 4.476849201000069556 ) ) ;
#1885 = CARTESIAN_POINT ( 'NONE',  ( -6.174373104427945513, 119.6968065231476857, -1.242162679386602520 ) ) ;
#1886 = FACE_OUTER_BOUND ( 'NONE', #34234, .T. ) ;
#1887 = CARTESIAN_POINT ( 'NONE',  ( 4.224925902082478757, 118.2240476267590736, 0.4891913066779954300 ) ) ;
#1888 = CARTESIAN_POINT ( 'NONE',  ( -12.10601879509736634, 151.9817061558079274, -1.041216838735509187 ) ) ;
#1889 = DIRECTION ( 'NONE',  ( -0.3582377630123937950, 0.9336303900108844367, -3.445432962228676930E-16 ) ) ;
#1890 = CARTESIAN_POINT ( 'NONE',  ( 18.86374853661768825, 125.3403196291361610, 0.3769425889880999581 ) ) ;
#1891 = EDGE_CURVE ( 'NONE', #17493, #17052, #5614, .T. ) ;
#1892 = ORIENTED_EDGE ( 'NONE', *, *, #31827, .F. ) ;
#1893 = CARTESIAN_POINT ( 'NONE',  ( -4.247245584637960647, 22.75789413176893206, 1.861891798430825862 ) ) ;
#1894 = CARTESIAN_POINT ( 'NONE',  ( -3.522522545432727359, 120.3814187630814132, -0.6186928868410387361 ) ) ;
#1895 = CARTESIAN_POINT ( 'NONE',  ( 3.174366308151882254, 69.94346620154573202, 0.06343139340882769650 ) ) ;
#1896 = DIRECTION ( 'NONE',  ( 0.3582377630123966261, -0.9336303900108832154, 0.000000000000000000 ) ) ;
#1897 = DIRECTION ( 'NONE',  ( -5.188838149069471174E-16, 1.699382548006136313E-16, 1.000000000000000000 ) ) ;
#1898 = CARTESIAN_POINT ( 'NONE',  ( -6.991872955157565350, 121.9342904866002186, -0.005970709178320789817 ) ) ;
#1899 = DIRECTION ( 'NONE',  ( -0.7770581983690837413, 0.6294287539884032556, -5.101669463485834765E-16 ) ) ;
#1900 = CARTESIAN_POINT ( 'NONE',  ( 22.03992273305654237, 150.6352520364973486, 1.509874617927603024 ) ) ;
#1901 = CARTESIAN_POINT ( 'NONE',  ( 4.130807148828959718, 104.6144662015457385, -2.502011538036419402 ) ) ;
#1903 = CARTESIAN_POINT ( 'NONE',  ( 21.42146139051182985, 149.1985357531029308, -1.383244442692061149 ) ) ;
#1902 = CARTESIAN_POINT ( 'NONE',  ( 3.028202472743143581, -14.11696900735987015, 1.123381337427139526 ) ) ;
#1904 = CARTESIAN_POINT ( 'NONE',  ( -0.01081828683970047049, 119.3136608367422866, 0.5413913113077200023 ) ) ;
#1905 = CARTESIAN_POINT ( 'NONE',  ( 1.653223041919489544, 21.06826514481450729, 4.324967054831568625 ) ) ;
#1906 = CARTESIAN_POINT ( 'NONE',  ( -14.40286820143220936, 120.3907653763288579, -0.8772178161575924227 ) ) ;
#1907 = VECTOR ( 'NONE', #2855, 1000.000000000000000 ) ;
#1908 = CARTESIAN_POINT ( 'NONE',  ( -0.1559983344249278314, 9.848737885527594216, 0.9609112391775298523 ) ) ;
#1909 = EDGE_LOOP ( 'NONE', ( #42053, #40651, #8623, #21459 ) ) ;
#1910 = ADVANCED_FACE ( 'NONE', ( #37755 ), #18355, .F. ) ;
#1911 = CARTESIAN_POINT ( 'NONE',  ( -50.02669608763528686, 12.78473261814649931, -8.015744983012485712E-15 ) ) ;
#1912 = CARTESIAN_POINT ( 'NONE',  ( -9.756861847786568731, 124.2227999206177032, 0.4199055954619892450 ) ) ;
#1913 = CARTESIAN_POINT ( 'NONE',  ( 5.228661469329079381, -12.87456325985388084, 2.426867231591100182 ) ) ;
#1914 = CARTESIAN_POINT ( 'NONE',  ( 2.563812760316453332, 119.9929590031203901, -0.5332384965226230067 ) ) ;
#1915 = ORIENTED_EDGE ( 'NONE', *, *, #26964, .T. ) ;
#1916 = CARTESIAN_POINT ( 'NONE',  ( 1.123125151977883318, 115.7029491485453718, 1.744272880635622247 ) ) ;
#1917 = ORIENTED_EDGE ( 'NONE', *, *, #29167, .T. ) ;
#1918 = CARTESIAN_POINT ( 'NONE',  ( 3.334874478900925254, -13.11215654211414439, 1.739483084651320066 ) ) ;
#1919 = CARTESIAN_POINT ( 'NONE',  ( -4.780916927273618278, 117.8747006157190214, -0.8582680989615314449 ) ) ;
#1920 = CARTESIAN_POINT ( 'NONE',  ( 9.145901261935787119, 124.1724329610943300, 0.1484858654357239516 ) ) ;
#1921 = ORIENTED_EDGE ( 'NONE', *, *, #7173, .T. ) ;
#1922 = CARTESIAN_POINT ( 'NONE',  ( 10.11172965818656166, 120.4647147465577461, 1.576227610178518201 ) ) ;
#1923 = DIRECTION ( 'NONE',  ( -1.000000000000000000, 0.000000000000000000, 0.000000000000000000 ) ) ;
#1924 = DIRECTION ( 'NONE',  ( 4.017660918040594346E-17, -1.000000000000000000, -2.376309959284834438E-19 ) ) ;
#1925 = EDGE_CURVE ( 'NONE', #11774, #22436, #31578, .T. ) ;
#1926 = CARTESIAN_POINT ( 'NONE',  ( -4.800085724567965784, 115.7029491485459545, -1.472342921364490298 ) ) ;
#1927 = CARTESIAN_POINT ( 'NONE',  ( 23.32536756748174867, 149.0517038676186417, 0.2354165988066211079 ) ) ;
#1928 = EDGE_CURVE ( 'NONE', #37721, #4510, #36907, .T. ) ;
#1929 =( BOUNDED_SURFACE ( )  B_SPLINE_SURFACE ( 3, 2, ( 
 ( #33401, #8037, #14410 ),
 ( #17193, #40014, #10806 ),
 ( #34033, #1662, #11018 ),
 ( #23788, #23998, #17402 ),
 ( #36809, #4445, #14616 ),
 ( #37019, #1247, #17608 ),
 ( #27417, #27620, #21418 ),
 ( #8666, #2290, #25054 ),
 ( #37636, #12281, #25487 ),
 ( #9092, #18441, #41475 ),
 ( #34444, #14827, #24845 ),
 ( #41685, #1865, #31447 ),
 ( #5907, #31874, #18868 ),
 ( #27832, #31023, #12067 ),
 ( #25270, #40838, #18658 ),
 ( #21839, #31231, #2715 ),
 ( #5277, #11641, #28675 ),
 ( #35085, #24626, #8460 ),
 ( #31663, #18229, #11858 ),
 ( #8241, #38274, #12492 ) ),
 .UNSPECIFIED., .F., .F., .T. ) 
 B_SPLINE_SURFACE_WITH_KNOTS ( ( 4, 2, 2, 2, 2, 2, 2, 2, 2, 4 ),
 ( 3, 3 ),
 ( -1.951563910473907981E-17, 0.0002906966660415815436, 0.0004360449990623821003, 0.0005813933320831826028, 0.0008720899981247837163, 0.001162786664166384721, 0.002325573328332788958, 0.002906966660415991402, 0.003488359992499193412, 0.004651146656665597866 ),
 ( 0.000000000000000000, 0.7115408901999051849 ),
 .UNSPECIFIED. ) 
 GEOMETRIC_REPRESENTATION_ITEM ( )  RATIONAL_B_SPLINE_SURFACE ( (
 ( 1.000000000000000000, 0.8295190474764645439, 0.9016464323943773618),
 ( 1.000000000000000000, 0.8295190474764645439, 0.9016464323943773618),
 ( 1.000000000000000000, 0.8295191844949277860, 0.9016465114428253713),
 ( 1.000000000000000000, 0.8295189621554358572, 0.9016463831711215571),
 ( 1.000000000000000000, 0.8295186834253872599, 0.9016462223666781295),
 ( 1.000000000000000000, 0.8295188167253252365, 0.9016462992698410783),
 ( 1.000000000000000000, 0.8295190048409176731, 0.9016464077971535485),
 ( 1.000000000000000000, 0.8295192071976853487, 0.9016465245404596818),
 ( 1.000000000000000000, 0.8295190396943252775, 0.9016464279047196051),
 ( 1.000000000000000000, 0.8295190584192864147, 0.9016464387074907272),
 ( 1.000000000000000000, 0.8295190452658104396, 0.9016464311190108827),
 ( 1.000000000000000000, 0.8295190572912768401, 0.9016464380567215109),
 ( 1.000000000000000000, 0.8295191187437633840, 0.9016464735097805550),
 ( 1.000000000000000000, 0.8295190147136782821, 0.9016464134929291774),
 ( 1.000000000000000000, 0.8295185759670760106, 0.9016461603720204998),
 ( 1.000000000000000000, 0.8295184858515097792, 0.9016461083827084222),
 ( 1.000000000000000000, 0.8295190237822920309, 0.9016464187247776874),
 ( 1.000000000000000000, 0.8295190933398598476, 0.9016464588538057878),
 ( 1.000000000000000000, 0.8295190474770748335, 0.9016464323947295245),
 ( 1.000000000000000000, 0.8295190474770748335, 0.9016464323947295245) ) ) 
 REPRESENTATION_ITEM ( '' )  SURFACE ( )  );
#1930 = CARTESIAN_POINT ( 'NONE',  ( -5.177913976931281859, 56.51500000000002899, -5.372099999999998765 ) ) ;
#1931 = COLOUR_RGB ( '', 0.31764706, 0.68627451, 0.89019608) ;
#1932 = EDGE_CURVE ( 'NONE', #25709, #5098, #38932, .T. ) ;
#1933 = CARTESIAN_POINT ( 'NONE',  ( 1.986764264153795478, -15.15368377650233533, 5.911265622359163530 ) ) ;
#1934 = DIRECTION ( 'NONE',  ( 5.188838149069471174E-16, -1.699382548006136313E-16, -1.000000000000000000 ) ) ;
#1935 = CYLINDRICAL_SURFACE ( 'NONE', #12373, 2.539999999999999591 ) ;
#1936 = CARTESIAN_POINT ( 'NONE',  ( -4.735645682745369456, 117.8440288062297441, 0.8352900991755182192 ) ) ;
#1937 = ORIENTED_EDGE ( 'NONE', *, *, #8400, .F. ) ;
#1938 = CYLINDRICAL_SURFACE ( 'NONE', #11847, 0.5080000000000000071 ) ;
#1939 = CARTESIAN_POINT ( 'NONE',  ( 8.527773727094952960, 119.1143268667826476, -0.9731819787258109145 ) ) ;
#1940 = CARTESIAN_POINT ( 'NONE',  ( -3.998531074477553293, 117.0582680968029905, -1.101271957883942942 ) ) ;
#1941 = CARTESIAN_POINT ( 'NONE',  ( 4.962772945303370875, 117.4661736183843317, 0.9732638675253090232 ) ) ;
#1942 = CARTESIAN_POINT ( 'NONE',  ( -11.66725022231030628, 55.24499999999998323, -5.016500000000000625 ) ) ;
#1943 = CARTESIAN_POINT ( 'NONE',  ( -0.07831152689304127223, 109.4728569552520838, 3.919029035233798641 ) ) ;
#1944 = CARTESIAN_POINT ( 'NONE',  ( -10.73808814597608574, 77.14487411131504757, -1.523999999999998467 ) ) ;
#1945 = FACE_OUTER_BOUND ( 'NONE', #41913, .T. ) ;
#1946 = DIRECTION ( 'NONE',  ( -0.8745520943968243532, 0.4849315768086547296, -6.829619984160642269E-16 ) ) ;
#1947 = CARTESIAN_POINT ( 'NONE',  ( 1.990724735134854262, -15.09768785095407040, 5.370787383207776600 ) ) ;
#1948 = CARTESIAN_POINT ( 'NONE',  ( 5.187812668267121730, 115.4810986995850755, -1.301936727496811441 ) ) ;
#1949 = CARTESIAN_POINT ( 'NONE',  ( 0.9515549220119206009, 38.57169665032974848, 1.406172627325484203 ) ) ;
#1950 = CARTESIAN_POINT ( 'NONE',  ( -0.4316363188167808840, 115.7034387397185213, 1.748257578123638245 ) ) ;
#1951 = CARTESIAN_POINT ( 'NONE',  ( 4.326043401919948295, 8.289558097378858292, -1.648119079657388353 ) ) ;
#1952 = EDGE_LOOP ( 'NONE', ( #3276, #12265, #13796, #35170 ) ) ;
#1953 = CARTESIAN_POINT ( 'NONE',  ( -2.761919320456341698, 105.1243152825708620, -4.564426355482043896 ) ) ;
#1954 = CARTESIAN_POINT ( 'NONE',  ( 4.220783105811589664, -15.35787857112312693, 0.3368293509108917783 ) ) ;
#1955 = CARTESIAN_POINT ( 'NONE',  ( -15.53591925045088651, 153.1703808545849483, 1.736877461573578030 ) ) ;
#1956 = CARTESIAN_POINT ( 'NONE',  ( 0.9071407760921452734, 21.51634675185595924, 0.3571511405359465430 ) ) ;
#1957 = CARTESIAN_POINT ( 'NONE',  ( -0.9163883642843115851, 13.89126970375589032, 0.3362141533434955809 ) ) ;
#1958 = ORIENTED_EDGE ( 'NONE', *, *, #31551, .T. ) ;
#1959 = ORIENTED_EDGE ( 'NONE', *, *, #28804, .T. ) ;
#1960 = DIRECTION ( 'NONE',  ( -0.4849315768086426282, -0.8745520943968310146, -1.030032898892908135E-16 ) ) ;
#1961 = CARTESIAN_POINT ( 'NONE',  ( 2.642867612521250908, 121.0686911241271702, 0.3905210903889254070 ) ) ;
#1962 = SURFACE_SIDE_STYLE ('',( #8555 ) ) ;
#1963 = CARTESIAN_POINT ( 'NONE',  ( -9.666892607209499388, 123.4354624054469980, 0.6853163995640745298 ) ) ;
#1964 = DIRECTION ( 'NONE',  ( 1.000000000000000000, 0.000000000000000000, 1.224646799147353207E-16 ) ) ;
#1965 = CARTESIAN_POINT ( 'NONE',  ( 3.325379330704291814, -12.45968715000887705, 0.9553361148970926919 ) ) ;
#1966 = CARTESIAN_POINT ( 'NONE',  ( 2.217461812776179819, 157.2504501563031738, -1.545323669738358552 ) ) ;
#1967 = CARTESIAN_POINT ( 'NONE',  ( -19.82367009662587520, 149.5711785761137662, -2.459487706365388604 ) ) ;
#1968 = DIRECTION ( 'NONE',  ( -6.353134868986659519E-16, 1.000000000000000000, 0.000000000000000000 ) ) ;
#1969 = CARTESIAN_POINT ( 'NONE',  ( 4.074910602682932925, 118.2429491485453497, -0.1454311599470141936 ) ) ;
#1970 = CARTESIAN_POINT ( 'NONE',  ( 6.492529462933093853, 121.6679077367135591, -0.1901135952749836711 ) ) ;
#1971 = ADVANCED_FACE ( 'NONE', ( #38187 ), #8579, .F. ) ;
#1972 = ORIENTED_EDGE ( 'NONE', *, *, #22219, .T. ) ;
#1973 = CARTESIAN_POINT ( 'NONE',  ( 3.046489168745748266, -14.83993489217504091, 3.784491786591300588 ) ) ;
#1974 = CIRCLE ( 'NONE', #6741, 0.7620000000000015650 ) ;
#1975 = VECTOR ( 'NONE', #16197, 1000.000000000000000 ) ;
#1976 = FACE_OUTER_BOUND ( 'NONE', #17302, .T. ) ;
#1977 = CARTESIAN_POINT ( 'NONE',  ( -58.42460811326324688, -0.3780437665152627247, 0.3615838660048876774 ) ) ;
#1978 = CARTESIAN_POINT ( 'NONE',  ( 2.099109474952898236, -4.195072059908932616, -4.137704358558784712 ) ) ;
#1979 = CARTESIAN_POINT ( 'NONE',  ( 1.456364663599907905, 120.2326517397585377, 0.4672470943647334396 ) ) ;
#1980 = CARTESIAN_POINT ( 'NONE',  ( -3.216045294022573664, 29.79186273158684983, 3.430717191674401700 ) ) ;
#1981 = CARTESIAN_POINT ( 'NONE',  ( -2.055333930833691092, 107.8038693663528278, 4.443139710053165103 ) ) ;
#1982 = EDGE_CURVE ( 'NONE', #17903, #12743, #14742, .T. ) ;
#1983 = CARTESIAN_POINT ( 'NONE',  ( 3.501419995798253915, -2.955197114699519734, 3.043391175950921568 ) ) ;
#1984 = CARTESIAN_POINT ( 'NONE',  ( -0.5321123018419734452, 37.22158963861809156, -0.7300149017649124605 ) ) ;
#1985 = EDGE_CURVE ( 'NONE', #25154, #18870, #41173, .T. ) ;
#1986 = CARTESIAN_POINT ( 'NONE',  ( -4.386519595447357922, 0.5779702600499575516, 7.231359419481246498 ) ) ;
#1987 = CARTESIAN_POINT ( 'NONE',  ( -57.48728866487982714, 1.341405240446180702, -0.2210608495301590037 ) ) ;
#1988 = CARTESIAN_POINT ( 'NONE',  ( 2.158285020023808176, 116.4043711044980540, -0.2448377587554940171 ) ) ;
#1989 = CYLINDRICAL_SURFACE ( 'NONE', #14889, 0.2539999999999996705 ) ;
#1990 = CARTESIAN_POINT ( 'NONE',  ( -14.53564353655538177, 79.78436006922240153, 1.269999999999997353 ) ) ;
#1991 = CARTESIAN_POINT ( 'NONE',  ( -6.442297258278467886, 29.65178619621697464, 0.8020365093557799696 ) ) ;
#1992 = CARTESIAN_POINT ( 'NONE',  ( 0.6763034141103227981, -4.228338640871131204, 8.424193199533098309 ) ) ;
#1993 = CARTESIAN_POINT ( 'NONE',  ( 0.3349063509247137138, 117.3993832491035363, 1.495621030033295940 ) ) ;
#1994 = DIRECTION ( 'NONE',  ( -0.9998004120163608288, 1.039227405372657318E-20, -0.01997839162482760098 ) ) ;
#1995 = CARTESIAN_POINT ( 'NONE',  ( 0.3785707606481875653, 120.7331730230137623, -0.5164240810526171677 ) ) ;
#1996 = CARTESIAN_POINT ( 'NONE',  ( -21.78567168733534842, 151.4242408681541008, 0.1492089687398850950 ) ) ;
#1997 = EDGE_LOOP ( 'NONE', ( #2346, #1937, #13889, #16961 ) ) ;
#1998 = CARTESIAN_POINT ( 'NONE',  ( -58.50860430493788300, 0.7049166599848583070, -0.9756837515128594651 ) ) ;
#1999 = AXIS2_PLACEMENT_3D ( 'NONE', #32311, #42126, #2936 ) ;
#2000 = CIRCLE ( 'NONE', #24436, 12.69999999999999751 ) ;
#2001 = VERTEX_POINT ( 'NONE', #41389 ) ;
#2002 = CARTESIAN_POINT ( 'NONE',  ( -47.72307967018490871, 19.52623448395591765, -5.191226814325721861 ) ) ;
#2003 = CARTESIAN_POINT ( 'NONE',  ( -15.72550100231863368, 145.6881679641610674, -0.3142329346387550681 ) ) ;
#2004 = CARTESIAN_POINT ( 'NONE',  ( 2.285161673027230389, -15.58026522864758334, 5.856586201423784388 ) ) ;
#2005 = CARTESIAN_POINT ( 'NONE',  ( -7.864631202759968964, 118.9574329095587757, 0.9664042006415775043 ) ) ;
#2006 = CARTESIAN_POINT ( 'NONE',  ( 19.81309253913735802, 152.3633698111425758, -1.013446639353942968 ) ) ;
#2007 = CARTESIAN_POINT ( 'NONE',  ( -1.287880193524239658, 20.15907059199006923, -4.440276399826991849 ) ) ;
#2008 = CARTESIAN_POINT ( 'NONE',  ( -18.54376275836462185, 154.1690995007799927, -0.7937872377295739357 ) ) ;
#2009 = CARTESIAN_POINT ( 'NONE',  ( -49.81232696645592029, 16.59374381583211999, -4.964399749387115257 ) ) ;
#2010 = VERTEX_POINT ( 'NONE', #21971 ) ;
#2011 = CARTESIAN_POINT ( 'NONE',  ( 2.182859927827073498, 116.1873359508715566, 0.04703207412767947126 ) ) ;
#2012 = DIRECTION ( 'NONE',  ( 0.9849462604886048966, -0.000000000000000000, 0.1728608224830406881 ) ) ;
#2013 = CARTESIAN_POINT ( 'NONE',  ( -6.588241325444357699, 120.6599796251122427, 0.8186057014055782011 ) ) ;
#2014 = CARTESIAN_POINT ( 'NONE',  ( -56.75031417288079183, 3.184683474932036518, -1.986967496122973520 ) ) ;
#2015 = CARTESIAN_POINT ( 'NONE',  ( 18.49981012119508605, 140.7300538122508726, -1.765484999878022654 ) ) ;
#2016 = CARTESIAN_POINT ( 'NONE',  ( -16.06052414861355970, 125.3625853296581312, -1.884096674228965540 ) ) ;
#2017 = CARTESIAN_POINT ( 'NONE',  ( -49.19743978460682143, 17.65503563884207594, -5.190924102448302158 ) ) ;
#2018 = CARTESIAN_POINT ( 'NONE',  ( 0.01596947694123658501, 156.4635559983122448, -0.7991779281049287142 ) ) ;
#2019 = ORIENTED_EDGE ( 'NONE', *, *, #35051, .F. ) ;
#2020 = CARTESIAN_POINT ( 'NONE',  ( -4.261081698622679603, 119.8084884740358547, -0.9035344350157260562 ) ) ;
#2021 = CARTESIAN_POINT ( 'NONE',  ( 4.136722333222721204, -15.50381924862055705, 2.038268645697551396 ) ) ;
#2022 = CARTESIAN_POINT ( 'NONE',  ( -4.441848593430714587, 118.1590354598291270, -0.6062622877682531941 ) ) ;
#2023 = CARTESIAN_POINT ( 'NONE',  ( -58.10099831372669854, 0.3475205698689753930, -0.9728495803591354907 ) ) ;
#2024 = CIRCLE ( 'NONE', #10859, 0.2540000000000017799 ) ;
#2025 = CARTESIAN_POINT ( 'NONE',  ( -5.007446857918051109, 117.4001727933947450, 0.7824604973016788811 ) ) ;
#2026 = CARTESIAN_POINT ( 'NONE',  ( 17.73735868213781330, 147.0764175921665640, 2.241444305069557164 ) ) ;
#2027 = DIRECTION ( 'NONE',  ( -5.206863593109713661E-17, 1.000000000000000000, -1.077750396879097183E-30 ) ) ;
#2028 = ADVANCED_FACE ( 'NONE', ( #12194 ), #33502, .T. ) ;
#2029 = TOROIDAL_SURFACE ( 'NONE', #21730, 0.3810000000000014486, 0.2540000000000000036 ) ;
#2030 = ADVANCED_FACE ( 'NONE', ( #40961 ), #17939, .T. ) ;
#2031 = CARTESIAN_POINT ( 'NONE',  ( -4.212901951478492890, -8.356617434558033963, -7.328762184035659821 ) ) ;
#2032 = CARTESIAN_POINT ( 'NONE',  ( 15.49830880841120795, 147.8629129908177049, 0.8994996151558262154 ) ) ;
#2033 = CARTESIAN_POINT ( 'NONE',  ( -13.46199999999999442, 13.84300000000000530, 0.000000000000000000 ) ) ;
#2035 = ORIENTED_EDGE ( 'NONE', *, *, #39593, .F. ) ;
#2034 = CARTESIAN_POINT ( 'NONE',  ( -44.40685758373553682, 19.43703734468912714, -0.2085933842879179878 ) ) ;
#2036 = DIRECTION ( 'NONE',  ( 0.9336303900108808840, 0.3582377630124026768, -4.808225039248730429E-15 ) ) ;
#2037 = CARTESIAN_POINT ( 'NONE',  ( -57.47393550255000605, 1.325481720219651161, 0.09114234605507165465 ) ) ;
#2038 = CARTESIAN_POINT ( 'NONE',  ( -52.43464216547582879, 18.97776253636583732, -1.004568992552039040E-14 ) ) ;
#2039 = CARTESIAN_POINT ( 'NONE',  ( -15.61624682818917265, 120.8175431576145940, -0.1535658744814573373 ) ) ;
#2040 = ORIENTED_EDGE ( 'NONE', *, *, #27411, .T. ) ;
#2041 = CARTESIAN_POINT ( 'NONE',  ( -49.70354115100154502, 23.42381831551578486, -0.3024929150989502658 ) ) ;
#2042 = CARTESIAN_POINT ( 'NONE',  ( 7.903461424171575267, 122.1176562113792983, -0.5506078847746120886 ) ) ;
#2043 = CARTESIAN_POINT ( 'NONE',  ( -8.019189887688819240, 121.5801876769127432, 0.8265596201061200521 ) ) ;
#2044 = ORIENTED_EDGE ( 'NONE', *, *, #9457, .T. ) ;
#2045 = CARTESIAN_POINT ( 'NONE',  ( -5.078986093043185157, 72.48346620154573827, -0.1014902294541238092 ) ) ;
#2046 = CARTESIAN_POINT ( 'NONE',  ( 0.001786757842161811136, 120.9379535345006076, -0.08941666878750617609 ) ) ;
#2047 = CARTESIAN_POINT ( 'NONE',  ( 3.754230566796173285, -14.80532124960526374, 5.272564796848507207 ) ) ;
#2048 = CARTESIAN_POINT ( 'NONE',  ( -17.30645727728363426, 153.8449085212272678, 1.293747054194649637 ) ) ;
#2049 = CARTESIAN_POINT ( 'NONE',  ( 5.230039278750658660, 78.94094791484917550, -5.321858878493932465 ) ) ;
#2050 = CARTESIAN_POINT ( 'NONE',  ( 23.37772998923890100, 142.7868430859564626, 0.6200176421473860833 ) ) ;
#2051 = CARTESIAN_POINT ( 'NONE',  ( 9.014329603292043913, 124.0612904411588318, 0.2246157754502237647 ) ) ;
#2052 = LINE ( 'NONE', #35065, #8782 ) ;
#2053 = CARTESIAN_POINT ( 'NONE',  ( -0.9703616065139187841, 22.75662690174698355, -0.1248384507273650884 ) ) ;
#2054 = CARTESIAN_POINT ( 'NONE',  ( -18.81533481972616428, 125.3161215262879580, -0.4318114027375014041 ) ) ;
#2055 = DIRECTION ( 'NONE',  ( -0.9998004120163608288, 0.000000000000000000, -0.01997839162482749342 ) ) ;
#2056 = CIRCLE ( 'NONE', #1394, 5.334000000000001407 ) ;
#2057 = CARTESIAN_POINT ( 'NONE',  ( -5.817775060672866871, 56.51499999999999346, -4.384522920466269014 ) ) ;
#2058 = ORIENTED_EDGE ( 'NONE', *, *, #8373, .F. ) ;
#2059 = CARTESIAN_POINT ( 'NONE',  ( -5.866213452989303079, 118.3783053522630979, 0.9224362309636404689 ) ) ;
#2060 = CARTESIAN_POINT ( 'NONE',  ( 2.913282581332740762, -14.11548038430587937, -3.586046950971230274 ) ) ;
#2061 = CARTESIAN_POINT ( 'NONE',  ( 14.13476661394972211, 155.9232964860746620, 1.730687652093988671 ) ) ;
#2062 = CARTESIAN_POINT ( 'NONE',  ( -55.76611385812176280, 5.250064693407995975, -2.603441191291675949 ) ) ;
#2063 = CARTESIAN_POINT ( 'NONE',  ( 20.34707623724158054, 149.4216517587604756, -1.615871423115795125 ) ) ;
#2064 = CARTESIAN_POINT ( 'NONE',  ( -3.436282163690115077, 26.04026231355703658, -7.687665148811276161 ) ) ;
#2065 = CARTESIAN_POINT ( 'NONE',  ( -22.07432572979854157, 148.5290936231802448, -2.031061984987305280 ) ) ;
#2066 = CARTESIAN_POINT ( 'NONE',  ( 4.869185350499654952, 117.6445503307796798, -0.8938492170851732865 ) ) ;
#2067 = CARTESIAN_POINT ( 'NONE',  ( 1.973215784349658497, 106.6933082031156772, 4.964841027628618342 ) ) ;
#2068 = EDGE_LOOP ( 'NONE', ( #28107, #7520, #34020, #14291 ) ) ;
#2069 = CARTESIAN_POINT ( 'NONE',  ( -15.40211203110487759, 147.8297367799732456, -0.07919316026241125794 ) ) ;
#2070 = CARTESIAN_POINT ( 'NONE',  ( -19.51070465195341797, 147.4874203640471535, -2.520207112597399934 ) ) ;
#2071 = CARTESIAN_POINT ( 'NONE',  ( 2.090134903116885656, -15.63197564439436427, 5.828951795168951122 ) ) ;
#2072 = DIRECTION ( 'NONE',  ( 5.188838149069472160E-16, -1.699382548006136559E-16, -1.000000000000000000 ) ) ;
#2073 = CARTESIAN_POINT ( 'NONE',  ( -8.480639930781094904, 68.51064353654967931, -1.269999999999995799 ) ) ;
#2074 = ORIENTED_EDGE ( 'NONE', *, *, #375, .F. ) ;
#2075 = CARTESIAN_POINT ( 'NONE',  ( 9.618126185770233150, 121.1143850344477215, 1.566364589618396419 ) ) ;
#2076 = DIRECTION ( 'NONE',  ( -0.9998501190848638753, -0.01731298258485278532, -8.537024980200814916E-16 ) ) ;
#2077 = TOROIDAL_SURFACE ( 'NONE', #9541, 0.3809999999999990616, 0.2540000000000000036 ) ;
#2078 = FACE_OUTER_BOUND ( 'NONE', #34790, .T. ) ;
#2079 = CARTESIAN_POINT ( 'NONE',  ( -0.4023205627561269870, 108.3383513567250986, 4.340400160729728896 ) ) ;
#2080 = CARTESIAN_POINT ( 'NONE',  ( 2.927854471352651533, -7.645316342317141967, 7.903470162911977681 ) ) ;
#2081 = CARTESIAN_POINT ( 'NONE',  ( 12.31319552751066659, 152.0262389575480881, 1.296791798139147023 ) ) ;
#2082 = CARTESIAN_POINT ( 'NONE',  ( -4.787717183442803837, 118.5930653697794384, -0.9403843580293530513 ) ) ;
#2083 = EDGE_CURVE ( 'NONE', #14687, #5970, #12181, .T. ) ;
#2084 = CARTESIAN_POINT ( 'NONE',  ( 18.36446446646845487, 154.1536317137893661, -0.4323159980074336994 ) ) ;
#2085 = CARTESIAN_POINT ( 'NONE',  ( 5.115576404397946142, 56.51499999999996504, -4.603576161448420301 ) ) ;
#2086 = CARTESIAN_POINT ( 'NONE',  ( -58.36801712489022975, -0.2878572300611665358, 0.05073317217019857051 ) ) ;
#2087 = FACE_OUTER_BOUND ( 'NONE', #40476, .T. ) ;
#2088 = VECTOR ( 'NONE', #7580, 1000.000000000000227 ) ;
#2089 = CYLINDRICAL_SURFACE ( 'NONE', #4237, 0.2539999999999942859 ) ;
#2090 = CARTESIAN_POINT ( 'NONE',  ( -4.287468807849243113, 118.2136502785617154, 0.3571622525904151746 ) ) ;
#2091 = CARTESIAN_POINT ( 'NONE',  ( -21.68875320759065062, 132.7412702629105468, -0.4333929054516005852 ) ) ;
#2092 = EDGE_LOOP ( 'NONE', ( #21526, #19689, #30798, #12030 ) ) ;
#2093 = CARTESIAN_POINT ( 'NONE',  ( -54.34142964503966056, 9.837102586603037935, 3.694930414371496052 ) ) ;
#2094 = CARTESIAN_POINT ( 'NONE',  ( -4.013207239964067696, 119.1603065593399720, -0.9237844164917737855 ) ) ;
#2095 = CARTESIAN_POINT ( 'NONE',  ( -1.381059818124894312, 106.2379067940291293, -5.172899357470507553 ) ) ;
#2096 = CARTESIAN_POINT ( 'NONE',  ( 4.350168497188355410, 118.1836287563303358, 0.6150604927752495454 ) ) ;
#2097 = CARTESIAN_POINT ( 'NONE',  ( -14.64564643111563846, 139.2174805014774392, -1.155614491733865989 ) ) ;
#2098 = DIRECTION ( 'NONE',  ( -1.000000000000000000, 0.000000000000000000, 0.000000000000000000 ) ) ;
#2099 = VECTOR ( 'NONE', #41623, 1000.000000000000000 ) ;
#2100 = DIRECTION ( 'NONE',  ( -1.011795553208986377E-16, -1.000000000000000000, 0.000000000000000000 ) ) ;
#2101 = ORIENTED_EDGE ( 'NONE', *, *, #26310, .T. ) ;
#2102 = CARTESIAN_POINT ( 'NONE',  ( 3.400481176189167343, 25.78150505744974552, 3.158589348000393482 ) ) ;
#2103 = CARTESIAN_POINT ( 'NONE',  ( -32.35039025330549123, 51.35812770460057664, 1.523999999999994248 ) ) ;
#2104 = CARTESIAN_POINT ( 'NONE',  ( -10.39456080247343905, 81.94606122948148652, -1.269999999999998908 ) ) ;
#2105 = DIRECTION ( 'NONE',  ( 0.8745520943968249084, -0.4849315768086533418, 5.271987356194193006E-16 ) ) ;
#2106 = CARTESIAN_POINT ( 'NONE',  ( -3.682264917456324227, 94.83546620154572793, -0.07358041635423923088 ) ) ;
#2107 = CARTESIAN_POINT ( 'NONE',  ( -7.810501765866526114, 122.5295832722994191, 0.1257769165047209758 ) ) ;
#2108 = DIRECTION ( 'NONE',  ( 0.8138664877804110409, 0.5810519254489896479, -5.002558946445370251E-16 ) ) ;
#2109 = CARTESIAN_POINT ( 'NONE',  ( 5.495761340641351467, 159.0395019988757781, 0.8742782617121154232 ) ) ;
#2110 = LINE ( 'NONE', #34903, #737 ) ;
#2112 = CARTESIAN_POINT ( 'NONE',  ( 16.31190729917912563, 125.3309463260932830, -1.192360770973151851 ) ) ;
#2111 = CARTESIAN_POINT ( 'NONE',  ( 1.852819980464847305, -15.24972552306870455, 5.408883774200016425 ) ) ;
#2113 = AXIS2_PLACEMENT_3D ( 'NONE', #41531, #15095, #8516 ) ;
#2114 = CARTESIAN_POINT ( 'NONE',  ( -11.41525058642626256, 122.8492764348241337, 1.228842657910306002 ) ) ;
#2115 = CARTESIAN_POINT ( 'NONE',  ( 0.7725963012898818816, -15.30024676335969325, -0.5870848125168374176 ) ) ;
#2116 = CARTESIAN_POINT ( 'NONE',  ( -4.821777392514813521, 117.1414559920645644, -0.5894805283384125794 ) ) ;
#2117 = CARTESIAN_POINT ( 'NONE',  ( 0.8451309169872193161, 21.29487494764119759, 0.4837088869917456346 ) ) ;
#2118 = ORIENTED_EDGE ( 'NONE', *, *, #37313, .T. ) ;
#2119 = CARTESIAN_POINT ( 'NONE',  ( -57.38720131040756200, 1.641502911523470942, 0.7119259365333153733 ) ) ;
#2120 = CARTESIAN_POINT ( 'NONE',  ( -0.6220149250935740337, 120.7813932625355307, 0.1825499261673581841 ) ) ;
#2121 = ADVANCED_FACE ( 'NONE', ( #27744 ), #4254, .T. ) ;
#2122 = CARTESIAN_POINT ( 'NONE',  ( 2.821817058828279823, -15.16010343277639194, 5.768636546787819341 ) ) ;
#2123 = CARTESIAN_POINT ( 'NONE',  ( 17.27955699683393576, 146.3482411845097886, -1.367784599882192254 ) ) ;
#2124 = EDGE_LOOP ( 'NONE', ( #28766, #34062, #4168, #38468 ) ) ;
#2125 = CARTESIAN_POINT ( 'NONE',  ( 1.943291158100776572, 115.7022449525728263, 1.718216098553282833 ) ) ;
#2126 = CARTESIAN_POINT ( 'NONE',  ( -4.724190901440335821, 117.9428858324453984, -0.8166581812100317528 ) ) ;
#2127 = EDGE_CURVE ( 'NONE', #34427, #9964, #34360, .T. ) ;
#2128 = CARTESIAN_POINT ( 'NONE',  ( 6.497458072406196550, 121.7745328324513139, 0.05723077286956951282 ) ) ;
#2129 = VERTEX_POINT ( 'NONE', #1990 ) ;
#2130 = CARTESIAN_POINT ( 'NONE',  ( 11.20355582914602266, 156.1341193432522800, 2.130866455309296192 ) ) ;
#2131 = DIRECTION ( 'NONE',  ( -0.8745520943968253524, 0.4849315768086530087, -8.537024980200771528E-16 ) ) ;
#2132 = FACE_OUTER_BOUND ( 'NONE', #16740, .T. ) ;
#2133 = CIRCLE ( 'NONE', #17762, 18.00660244842765323 ) ;
#2134 = EDGE_CURVE ( 'NONE', #25560, #18746, #14952, .T. ) ;
#2135 = CARTESIAN_POINT ( 'NONE',  ( -3.174366308152011928, 65.62546620154573418, -0.06343139340882732180 ) ) ;
#2136 = CARTESIAN_POINT ( 'NONE',  ( 18.59469708476128602, 154.1615476314759974, 0.06268175667117116545 ) ) ;
#2137 = CARTESIAN_POINT ( 'NONE',  ( 0.07831152689291247249, 109.4728569552520838, -3.919029035233798641 ) ) ;
#2138 = CIRCLE ( 'NONE', #30043, 12.69999999999999751 ) ;
#2139 = CARTESIAN_POINT ( 'NONE',  ( 1.887010163324958523, -15.42916175108831389, 5.374230824943217577 ) ) ;
#2140 = DIRECTION ( 'NONE',  ( -0.01997839162482749342, -1.040247600000944484E-18, 0.9998004120163608288 ) ) ;
#2141 = CARTESIAN_POINT ( 'NONE',  ( -14.73199999999999399, 12.96302561210691984, 0.000000000000000000 ) ) ;
#2142 = EDGE_CURVE ( 'NONE', #11267, #28559, #22172, .T. ) ;
#2143 = CARTESIAN_POINT ( 'NONE',  ( -4.846938226398710192, 117.8246799134837914, 0.6898159354236798047 ) ) ;
#2144 = ORIENTED_EDGE ( 'NONE', *, *, #14403, .F. ) ;
#2145 = ORIENTED_EDGE ( 'NONE', *, *, #40646, .F. ) ;
#2146 = DIRECTION ( 'NONE',  ( -1.000000000000000000, 0.000000000000000000, 0.000000000000000000 ) ) ;
#2147 = CARTESIAN_POINT ( 'NONE',  ( 8.513471249619389170, 119.1860349514362838, -0.9933054490459751751 ) ) ;
#2148 = CARTESIAN_POINT ( 'NONE',  ( -6.475519728870542835, 122.5560431351108974, -0.2403424393823894445 ) ) ;
#2149 = CARTESIAN_POINT ( 'NONE',  ( 4.716832267211478857, 117.7257293850826585, 1.100839505850291999 ) ) ;
#2150 = DIRECTION ( 'NONE',  ( 0.000000000000000000, 0.000000000000000000, -1.000000000000000000 ) ) ;
#2151 = CARTESIAN_POINT ( 'NONE',  ( -0.3351388899281586009, 111.5577547982948801, 3.138814863473581962 ) ) ;
#2152 = CARTESIAN_POINT ( 'NONE',  ( 3.895047602890354010, -2.730319773039217690, 2.488009491782988469 ) ) ;
#2153 = LINE ( 'NONE', #15113, #21689 ) ;
#2154 = LINE ( 'NONE', #41343, #29394 ) ;
#2155 = CARTESIAN_POINT ( 'NONE',  ( 3.383663933261424006, -14.10150345098371005, 4.318103191797684204 ) ) ;
#2156 = CARTESIAN_POINT ( 'NONE',  ( 5.259129974998846713, 118.7524313932052991, -0.4270625282899581099 ) ) ;
#2157 = CARTESIAN_POINT ( 'NONE',  ( -14.38208595515612664, 131.1674235819977241, -1.945708262771122854 ) ) ;
#2158 = CARTESIAN_POINT ( 'NONE',  ( -6.997652642833405601, 121.9526520506185676, -0.1398297539000763479 ) ) ;
#2159 = CARTESIAN_POINT ( 'NONE',  ( -4.945311175443938723, 30.81497459379012227, 3.823255950980341655 ) ) ;
#2160 = EDGE_CURVE ( 'NONE', #15671, #35981, #41599, .T. ) ;
#2161 = CARTESIAN_POINT ( 'NONE',  ( -1.039409186399214535, 115.7029401452854671, 1.708810721072470784 ) ) ;
#2162 = CARTESIAN_POINT ( 'NONE',  ( -0.5093740622119584671, 14.76157059199007016, 4.595130897425484306 ) ) ;
#2164 = EDGE_LOOP ( 'NONE', ( #13314, #38087, #29660, #7685 ) ) ;
#2163 = CARTESIAN_POINT ( 'NONE',  ( 13.28278499026787784, 156.9705208988102640, 0.7618315876160811628 ) ) ;
#2165 = CARTESIAN_POINT ( 'NONE',  ( 0.2403197276938094373, 104.6144662015456674, -5.339994071284486665 ) ) ;
#2166 = CARTESIAN_POINT ( 'NONE',  ( 4.466571682983457414, -15.50692525667736454, 1.643437993322231838 ) ) ;
#2167 = CARTESIAN_POINT ( 'NONE',  ( -8.634969826329047748, 120.3810071108087243, 1.137220218559220841 ) ) ;
#2168 = CARTESIAN_POINT ( 'NONE',  ( -0.6564745402265276253, 25.61689014148909393, -0.7196881648562951650 ) ) ;
#2169 = AXIS2_PLACEMENT_3D ( 'NONE', #13076, #6484, #533 ) ;
#2170 = CARTESIAN_POINT ( 'NONE',  ( -0.8868740923517060004, 23.60745955286466824, 0.4068859645678858938 ) ) ;
#2171 = ADVANCED_FACE ( 'NONE', ( #9830 ), #42101, .T. ) ;
#2172 = VERTEX_POINT ( 'NONE', #22589 ) ;
#2173 = ORIENTED_EDGE ( 'NONE', *, *, #33952, .F. ) ;
#2174 = DIRECTION ( 'NONE',  ( -0.9998004120163609398, -4.016384292689130894E-17, -0.01997839162482749689 ) ) ;
#2175 = CARTESIAN_POINT ( 'NONE',  ( 1.232226514448922616, 109.2701902778323557, 3.967559291276892885 ) ) ;
#2176 = CARTESIAN_POINT ( 'NONE',  ( -10.18692116311738438, 123.6566696788710686, 0.8138387218406053503 ) ) ;
#2177 = DIRECTION ( 'NONE',  ( -0.9849462604886047856, 0.000000000000000000, -0.1728608224830407714 ) ) ;
#2178 = CARTESIAN_POINT ( 'NONE',  ( 2.022490532284443088, -15.01207906941262671, 5.472131392975311925 ) ) ;
#2179 = CARTESIAN_POINT ( 'NONE',  ( 12.49185498700837016, 153.6617311634574037, -1.629683330142263076 ) ) ;
#2180 = AXIS2_PLACEMENT_3D ( 'NONE', #28788, #35189, #38591 ) ;
#2181 = CARTESIAN_POINT ( 'NONE',  ( -12.79701950029137691, 155.3440856034525837, -2.194532851538729012 ) ) ;
#2182 = CARTESIAN_POINT ( 'NONE',  ( -5.580495364573205386, 77.10007210032874525, -1.269999999999995799 ) ) ;
#2183 = EDGE_CURVE ( 'NONE', #2010, #24767, #25067, .T. ) ;
#2184 = CARTESIAN_POINT ( 'NONE',  ( -8.935197197525255319, 123.9063447689825779, -0.1785465045940570206 ) ) ;
#2185 = CARTESIAN_POINT ( 'NONE',  ( -0.7326219338007132764, 37.28220708697721619, 2.048504824603448959 ) ) ;
#2186 = CARTESIAN_POINT ( 'NONE',  ( 15.92039698932583569, 146.6311637152522565, -0.2762755564230129912 ) ) ;
#2187 = VERTEX_POINT ( 'NONE', #12611 ) ;
#2188 = CARTESIAN_POINT ( 'NONE',  ( 3.186936940905604754, -14.67134942876716153, 3.163583609075255598 ) ) ;
#2189 = FACE_OUTER_BOUND ( 'NONE', #17505, .T. ) ;
#2190 =( BOUNDED_CURVE ( )  B_SPLINE_CURVE ( 3, ( #1660, #40630, #31021, #41257 ),
 .UNSPECIFIED., .F., .T. ) 
 B_SPLINE_CURVE_WITH_KNOTS ( ( 4, 4 ),
 ( 0.6881516260757224446, 0.7252176650374851929 ),
 .UNSPECIFIED. ) 
 CURVE ( )  GEOMETRIC_REPRESENTATION_ITEM ( )  RATIONAL_B_SPLINE_CURVE ( ( 0.5306017708566714841, 0.5183752415894662402, 0.5098124223071008876, 0.5049133130095754263 ) ) 
 REPRESENTATION_ITEM ( '' )  );
#2191 = CARTESIAN_POINT ( 'NONE',  ( 2.383981540283352629, 36.81846344528510429, 1.803752045214196853 ) ) ;
#2192 = CARTESIAN_POINT ( 'NONE',  ( -52.02227077088271301, 12.92666902008283358, 4.429676403336999968 ) ) ;
#2193 = CARTESIAN_POINT ( 'NONE',  ( -1.997604609866625580, -12.39122764300357105, -4.168859717980781809 ) ) ;
#2194 = CARTESIAN_POINT ( 'NONE',  ( 4.379744549753488592, 120.5100497556178567, 0.6885478749808132681 ) ) ;
#2195 = CARTESIAN_POINT ( 'NONE',  ( -3.110005066758847025, 28.42684073856939619, 0.3580217987620312736 ) ) ;
#2196 = CARTESIAN_POINT ( 'NONE',  ( -5.907561988889506566, 118.9932487913337411, 0.3492918592308485448 ) ) ;
#2197 = TOROIDAL_SURFACE ( 'NONE', #25981, 0.7620000000000000107, 0.2540000000000000036 ) ;
#2198 = CARTESIAN_POINT ( 'NONE',  ( 2.522041008973656240, -3.380034811851383214, 3.874746376371965617 ) ) ;
#2199 = CARTESIAN_POINT ( 'NONE',  ( 2.836071964827284297, 121.0300505300837415, 0.05667146733340969189 ) ) ;
#2200 = CARTESIAN_POINT ( 'NONE',  ( 8.265420891810833837, -5.467761657695628053, -1.740095136296691214 ) ) ;
#2201 = CARTESIAN_POINT ( 'NONE',  ( -57.94149553976682654, 0.5275954726333825784, -0.3053296928521576636 ) ) ;
#2202 = CARTESIAN_POINT ( 'NONE',  ( 5.525492539046071627, 117.0090066130893547, -0.4571800171334148843 ) ) ;
#2203 = CARTESIAN_POINT ( 'NONE',  ( -0.9036232957556743495, 122.5862318000603182, -0.2430700419085213837 ) ) ;
#2204 = DIRECTION ( 'NONE',  ( -1.000000000000000000, 0.000000000000000000, 0.000000000000000000 ) ) ;
#2205 = CARTESIAN_POINT ( 'NONE',  ( -3.456281358658260583, 50.63946620154572997, -1.847419665314800508 ) ) ;
#2206 = CARTESIAN_POINT ( 'NONE',  ( -2.033853377119958061, -8.777475726645231902, -8.175041553700232555 ) ) ;
#2207 = CARTESIAN_POINT ( 'NONE',  ( 0.7927169096838266871, 117.9394488418538174, 1.400391285740484104 ) ) ;
#2208 = CARTESIAN_POINT ( 'NONE',  ( -23.43300365160792964, 82.12916405548841681, -1.270000000000006013 ) ) ;
#2209 = CARTESIAN_POINT ( 'NONE',  ( 5.177913976931212581, 57.15000000000004832, -5.372100000000001430 ) ) ;
#2210 = CARTESIAN_POINT ( 'NONE',  ( 0.4698238578430272705, 109.1907409294041429, -4.006476130220050891 ) ) ;
#2211 = CARTESIAN_POINT ( 'NONE',  ( -23.15061725546907212, 148.7607265879045144, 0.2678260907677696978 ) ) ;
#2212 = EDGE_CURVE ( 'NONE', #18094, #36577, #5178, .T. ) ;
#2213 = ORIENTED_EDGE ( 'NONE', *, *, #18348, .T. ) ;
#2214 = CARTESIAN_POINT ( 'NONE',  ( -58.83227707057485389, -0.08366279997994163775, -5.798466560119647675E-15 ) ) ;
#2215 = AXIS2_PLACEMENT_3D ( 'NONE', #11347, #15162, #11767 ) ;
#2216 = ORIENTED_EDGE ( 'NONE', *, *, #20706, .T. ) ;
#2217 = DIRECTION ( 'NONE',  ( 4.017660918040594346E-17, -1.000000000000000000, -2.376309959284832031E-19 ) ) ;
#2218 = CARTESIAN_POINT ( 'NONE',  ( -11.82813386268903955, 130.3161362890850512, -0.2363542639706542603 ) ) ;
#2219 = CARTESIAN_POINT ( 'NONE',  ( 5.861737433447875567, -14.68024823731529871, 2.247769314782747774 ) ) ;
#2220 = CARTESIAN_POINT ( 'NONE',  ( -20.59592450876364111, 149.8464234248869786, 1.516103928358539354 ) ) ;
#2221 = CARTESIAN_POINT ( 'NONE',  ( 22.12956052442012833, 150.1365687424457178, -0.8564216397177741857 ) ) ;
#2222 = CARTESIAN_POINT ( 'NONE',  ( -4.319812470756069445, 11.96289413176387129, -1.686699837767231536 ) ) ;
#2223 = CARTESIAN_POINT ( 'NONE',  ( -21.82265835376372820, 151.4369626909183637, -0.8820245880042205666 ) ) ;
#2224 = CARTESIAN_POINT ( 'NONE',  ( -52.46109226273545545, 12.10756162195068875, -4.274556252865695072 ) ) ;
#2225 = EDGE_LOOP ( 'NONE', ( #11497, #24620, #32981, #34647 ) ) ;
#2226 = CARTESIAN_POINT ( 'NONE',  ( -8.798540845223380202, 117.6856535658803864, -0.1377603156279901264 ) ) ;
#2227 = DIRECTION ( 'NONE',  ( 4.017660918040594346E-17, -1.000000000000000000, -2.376309959284834438E-19 ) ) ;
#2228 = CARTESIAN_POINT ( 'NONE',  ( -0.5414988153860592623, 119.6443647996702566, 0.5124704023889978810 ) ) ;
#2229 = CARTESIAN_POINT ( 'NONE',  ( -53.71463501147313480, 9.386209292303481888, -3.577838831676722009 ) ) ;
#2230 = EDGE_CURVE ( 'NONE', #40395, #23452, #12158, .T. ) ;
#2231 = CARTESIAN_POINT ( 'NONE',  ( 18.33246729151843724, 150.1405190176936344, -1.740612831648467695 ) ) ;
#2232 = CARTESIAN_POINT ( 'NONE',  ( -13.53750608930591959, 121.6867650304669013, -1.656372850109685047 ) ) ;
#2233 = CARTESIAN_POINT ( 'NONE',  ( -55.41603145274652320, 6.826612083464994818, -3.210495615568592420 ) ) ;
#2234 = AXIS2_PLACEMENT_3D ( 'NONE', #11988, #28602, #8590 ) ;
#2235 = EDGE_CURVE ( 'NONE', #1712, #17404, #41159, .T. ) ;
#2236 = CARTESIAN_POINT ( 'NONE',  ( 7.748985956666678554, 122.1869765257964673, -0.4223483383238798017 ) ) ;
#2237 = EDGE_LOOP ( 'NONE', ( #5526, #41184 ) ) ;
#2238 = CARTESIAN_POINT ( 'NONE',  ( -12.92173176740960550, 125.9520529675768898, -1.821380522590920314 ) ) ;
#2239 = CARTESIAN_POINT ( 'NONE',  ( 2.004873297308811253, -15.47002699807756265, 5.272742632645636363 ) ) ;
#2240 = CARTESIAN_POINT ( 'NONE',  ( -4.156053678908833149, 118.2394346424153753, -0.3882629985390713134 ) ) ;
#2241 = CARTESIAN_POINT ( 'NONE',  ( -58.73801720703743001, -0.4998429216807459552, -0.2437502737749605297 ) ) ;
#2242 = TOROIDAL_SURFACE ( 'NONE', #20571, 5.080000000000005400, 0.5080000000000000071 ) ;
#2243 = CARTESIAN_POINT ( 'NONE',  ( -33.42971872652992005, 49.93539301574497102, -1.270000000000005569 ) ) ;
#2244 = CARTESIAN_POINT ( 'NONE',  ( 3.403275764582821772, 119.7942873563901713, 0.7909988017435812813 ) ) ;
#2245 = FACE_OUTER_BOUND ( 'NONE', #28960, .T. ) ;
#2246 = CARTESIAN_POINT ( 'NONE',  ( 1.765626013768924807, -4.031643488171090972, 8.243228240708695864 ) ) ;
#2247 = CARTESIAN_POINT ( 'NONE',  ( 15.80138807371428378, 145.9351319680867221, 0.6472794460535243877 ) ) ;
#2248 = CARTESIAN_POINT ( 'NONE',  ( -6.985000000000036735, 57.14999999999998437, 0.000000000000000000 ) ) ;
#2249 = CARTESIAN_POINT ( 'NONE',  ( -36.43259636504752308, 28.15155085495446485, 1.269999999999995799 ) ) ;
#2250 = CARTESIAN_POINT ( 'NONE',  ( -0.3944222225486587186, 117.3993832485554094, 1.481046348585886241 ) ) ;
#2251 = CARTESIAN_POINT ( 'NONE',  ( -57.92346726745822849, 0.7446056814934959300, 1.206286704679851107 ) ) ;
#2252 = LINE ( 'NONE', #11602, #31088 ) ;
#2253 = VECTOR ( 'NONE', #36473, 1000.000000000000114 ) ;
#2254 = DIRECTION ( 'NONE',  ( -0.8745520943968243532, 0.4849315768086547296, -6.829619984160642269E-16 ) ) ;
#2255 = CARTESIAN_POINT ( 'NONE',  ( -51.10637696787394191, 21.44594517334857287, 0.3731469903906310948 ) ) ;
#2256 = CARTESIAN_POINT ( 'NONE',  ( -1.829002187088467624, 116.5125207362610951, 0.06620492630546143120 ) ) ;
#2257 = ORIENTED_EDGE ( 'NONE', *, *, #13992, .T. ) ;
#2258 = CARTESIAN_POINT ( 'NONE',  ( -48.45250714818473625, 19.88962760504932348, -4.734234960886007926 ) ) ;
#2259 = CARTESIAN_POINT ( 'NONE',  ( 7.829869863957400256, 122.4471846315678079, -0.2494498989964459290 ) ) ;
#2260 = FACE_OUTER_BOUND ( 'NONE', #37704, .T. ) ;
#2261 = ORIENTED_EDGE ( 'NONE', *, *, #21856, .F. ) ;
#2262 = CARTESIAN_POINT ( 'NONE',  ( 2.065091541609473058, 115.7028726122111948, -1.634879014494797334 ) ) ;
#2263 = CARTESIAN_POINT ( 'NONE',  ( -9.301463764468643092, 124.2035065715909496, -0.4191708393134263577 ) ) ;
#2264 = CARTESIAN_POINT ( 'NONE',  ( 5.365742231761132963, -12.30384844886438245, 1.459887348375163096 ) ) ;
#2265 = CARTESIAN_POINT ( 'NONE',  ( -21.81117068996452701, 146.0876064316611860, 1.285479812297503965 ) ) ;
#2266 = DIRECTION ( 'NONE',  ( 1.000000000000000000, -1.162840169671635117E-16, 0.000000000000000000 ) ) ;
#2267 = AXIS2_PLACEMENT_3D ( 'NONE', #13762, #23962, #39769 ) ;
#2268 = CARTESIAN_POINT ( 'NONE',  ( 13.61156529719771768, 119.6358206793323404, 0.4233406866235921995 ) ) ;
#2269 = CARTESIAN_POINT ( 'NONE',  ( 5.952364314655516075, 121.5461442270676287, 0.1560439712719428051 ) ) ;
#2270 = FACE_OUTER_BOUND ( 'NONE', #16307, .T. ) ;
#2271 = CARTESIAN_POINT ( 'NONE',  ( -0.7497900579835341528, 31.49133049583988608, -0.6186479539722394838 ) ) ;
#2272 = CARTESIAN_POINT ( 'NONE',  ( -14.87533653215399099, 120.3210621052586475, -0.3471466443384769174 ) ) ;
#2273 = CARTESIAN_POINT ( 'NONE',  ( -41.09676540851935300, 23.04694042099051998, -1.524000000000031996 ) ) ;
#2274 = CARTESIAN_POINT ( 'NONE',  ( 5.177913976931196594, 78.94499979771845233, -5.372100000000001430 ) ) ;
#2275 = VERTEX_POINT ( 'NONE', #2833 ) ;
#2276 = CARTESIAN_POINT ( 'NONE',  ( 8.299051278477378446, 119.9935803421679026, 1.450008147901515221 ) ) ;
#2277 = DIRECTION ( 'NONE',  ( 5.188838149069472160E-16, -1.699382548006136559E-16, -1.000000000000000000 ) ) ;
#2278 = CARTESIAN_POINT ( 'NONE',  ( 21.50396862640721807, 149.5883454796168621, 2.135274339423805401 ) ) ;
#2279 = CARTESIAN_POINT ( 'NONE',  ( 20.18403667007061841, 149.6821479856479300, -1.616815787834455787 ) ) ;
#2280 = CARTESIAN_POINT ( 'NONE',  ( 3.417104117279694098, -14.34023910220586906, -3.129441506049576383 ) ) ;
#2281 = CARTESIAN_POINT ( 'NONE',  ( -0.3664415811652171340, 117.3568105388816321, -0.4447864970249671979 ) ) ;
#2282 = CARTESIAN_POINT ( 'NONE',  ( 4.981436116827920202, 117.5302645918864073, -0.7678635597125215151 ) ) ;
#2283 = ADVANCED_FACE ( 'NONE', ( #16420 ), #6435, .T. ) ;
#2284 = CARTESIAN_POINT ( 'NONE',  ( 3.916844122728723843, 109.8065891650451249, 3.681372831196203066 ) ) ;
#2285 = CARTESIAN_POINT ( 'NONE',  ( -4.254723467274468263, 155.8413357349917021, 0.07908073517333538693 ) ) ;
#2286 = CARTESIAN_POINT ( 'NONE',  ( -10.36135117696322538, 155.6679353847891321, -2.160796112024522486 ) ) ;
#2287 = CARTESIAN_POINT ( 'NONE',  ( 5.089472049306802859, -15.08631191614791334, 3.825519591672899455 ) ) ;
#2288 = CIRCLE ( 'NONE', #26061, 0.3810000000000000053 ) ;
#2289 = CARTESIAN_POINT ( 'NONE',  ( -7.994219716368544226, 68.36415334912796027, -1.523999999999995580 ) ) ;
#2290 = CARTESIAN_POINT ( 'NONE',  ( -0.6939310137895168262, 117.9496057704760972, -1.401774709011093245 ) ) ;
#2291 = CIRCLE ( 'NONE', #254, 3.683000000000001162 ) ;
#2292 = ORIENTED_EDGE ( 'NONE', *, *, #26205, .F. ) ;
#2293 = CARTESIAN_POINT ( 'NONE',  ( 17.74096168611281144, 140.4837523222294351, 2.437162785362842587 ) ) ;
#2294 = CARTESIAN_POINT ( 'NONE',  ( -13.99440778436217592, 79.95103047660883533, 1.523999999999998023 ) ) ;
#2295 = CARTESIAN_POINT ( 'NONE',  ( -3.072892473034376959, 118.0774402770256444, -0.9619640826930374589 ) ) ;
#2296 = VECTOR ( 'NONE', #9251, 1000.000000000000000 ) ;
#2297 = CARTESIAN_POINT ( 'NONE',  ( -0.4698238578431560564, 109.1907409294041429, 4.006476130220050891 ) ) ;
#2298 = CARTESIAN_POINT ( 'NONE',  ( -7.485859564062662841, -11.32103332335322499, -3.896386919873200405 ) ) ;
#2299 = CARTESIAN_POINT ( 'NONE',  ( -0.01133107913651179230, 156.3792106723807649, 0.5670535347366658652 ) ) ;
#2300 = CARTESIAN_POINT ( 'NONE',  ( -41.97746338594183868, 23.60773098774231826, -1.524000000000005794 ) ) ;
#2301 = CARTESIAN_POINT ( 'NONE',  ( 22.83860824214428575, 149.7823008822066697, -0.3949144739309157770 ) ) ;
#2302 = CARTESIAN_POINT ( 'NONE',  ( 5.860205464978446521, 56.51500000000089585, -5.019550312247728741 ) ) ;
#2303 = CARTESIAN_POINT ( 'NONE',  ( -58.12591287054759448, 0.2317919070111071345, 0.6797015115164672938 ) ) ;
#2304 = CARTESIAN_POINT ( 'NONE',  ( -8.793872193760559952, 117.6946653426936962, -0.2789185993360862037 ) ) ;
#2305 = DIRECTION ( 'NONE',  ( 0.9876665170007968841, -0.1565721916417945614, 5.390917751951445902E-16 ) ) ;
#2306 = CARTESIAN_POINT ( 'NONE',  ( -4.319384318635175468, 118.2117244580575601, 0.3218571067570579758 ) ) ;
#2307 = CARTESIAN_POINT ( 'NONE',  ( -15.56076557482332490, 120.7233670659379214, -0.3109411287488703657 ) ) ;
#2308 = EDGE_LOOP ( 'NONE', ( #25105, #6406, #17355, #34621 ) ) ;
#2309 = CARTESIAN_POINT ( 'NONE',  ( -52.50198181065980663, 11.96455506022023307, 4.263607785004571937 ) ) ;
#2310 = CARTESIAN_POINT ( 'NONE',  ( -8.219350291155233634, 120.3834793910760510, -1.437375401876854308 ) ) ;
#2311 = CARTESIAN_POINT ( 'NONE',  ( 0.09347673290359038989, 104.6144662015457385, -6.110098594576430564 ) ) ;
#2312 = VECTOR ( 'NONE', #35901, 1000.000000000000000 ) ;
#2313 = CARTESIAN_POINT ( 'NONE',  ( -2.711066548582671931, 120.7183352303693340, -0.3631387678457470014 ) ) ;
#2314 = CARTESIAN_POINT ( 'NONE',  ( -17.68910244842765778, 8.844871939465427602, 2.166290269325653984E-15 ) ) ;
#2315 = FACE_OUTER_BOUND ( 'NONE', #3086, .T. ) ;
#2316 = VERTEX_POINT ( 'NONE', #3043 ) ;
#2317 = CARTESIAN_POINT ( 'NONE',  ( 4.037907715354051241, 27.70556447992504445, -2.267523456217593214 ) ) ;
#2318 = CARTESIAN_POINT ( 'NONE',  ( -29.61277755908112042, 68.29894143245043381, 1.523999999991891618 ) ) ;
#2319 = DIRECTION ( 'NONE',  ( 0.9998004120163610509, 4.016384292689131511E-17, 0.01997839162482749689 ) ) ;
#2320 = CARTESIAN_POINT ( 'NONE',  ( -8.313969523394650452, 67.96940778435646280, -1.269999999999995355 ) ) ;
#2321 = AXIS2_PLACEMENT_3D ( 'NONE', #12658, #26490, #15841 ) ;
#2322 = CARTESIAN_POINT ( 'NONE',  ( -41.06680163122278060, 23.07855206975584395, 1.270000052244668831 ) ) ;
#2323 = CARTESIAN_POINT ( 'NONE',  ( 7.785296811173602727, 122.6196569424365066, 0.2112341757090067940 ) ) ;
#2324 = CARTESIAN_POINT ( 'NONE',  ( 4.466176584706416541, 22.48015689762229030, 1.290832665783417488 ) ) ;
#2325 = CARTESIAN_POINT ( 'NONE',  ( 14.11323155926160666, 120.5239346615589540, 1.094216903015625242 ) ) ;
#2326 = CARTESIAN_POINT ( 'NONE',  ( -2.496980690863166430, 104.6144662015454543, -4.139511689303219555 ) ) ;
#2328 = CARTESIAN_POINT ( 'NONE',  ( 13.73828690980672995, 121.6032371815301900, -1.070726600328922418 ) ) ;
#2327 = CARTESIAN_POINT ( 'NONE',  ( 2.769760999665409340, -14.92388480464812872, 4.423285184949336646 ) ) ;
#2329 = CARTESIAN_POINT ( 'NONE',  ( -13.41341228195548574, 125.8771108566470502, 1.381187796596252459 ) ) ;
#2330 = CARTESIAN_POINT ( 'NONE',  ( -3.182929088426432074, 26.46582164074821009, -3.363547984189534379 ) ) ;
#2331 = CARTESIAN_POINT ( 'NONE',  ( -8.117713882137797654, 117.8329967196738153, -0.7633534655056999352 ) ) ;
#2332 = AXIS2_PLACEMENT_3D ( 'NONE', #33270, #26866, #7494 ) ;
#2333 = CARTESIAN_POINT ( 'NONE',  ( -0.4659799999662124215, -3.540968264561009882, -0.8578381542037093466 ) ) ;
#2334 = VERTEX_POINT ( 'NONE', #19409 ) ;
#2335 = CARTESIAN_POINT ( 'NONE',  ( -57.28860081656939229, 2.041040056096066202, 1.590330371070447946 ) ) ;
#2336 = CARTESIAN_POINT ( 'NONE',  ( -15.41453346427796944, 143.5427300040290106, 0.2938895485367989946 ) ) ;
#2337 = CARTESIAN_POINT ( 'NONE',  ( 4.239944546232853106, -14.55591092887127758, 4.867068800921800609 ) ) ;
#2338 = CARTESIAN_POINT ( 'NONE',  ( 10.60975745311338692, 123.7931190674884050, -0.9249770984159892961 ) ) ;
#2339 = AXIS2_PLACEMENT_3D ( 'NONE', #14743, #20499, #27118 ) ;
#2340 = VERTEX_POINT ( 'NONE', #25401 ) ;
#2341 = VECTOR ( 'NONE', #1296, 1000.000000000000000 ) ;
#2342 = CARTESIAN_POINT ( 'NONE',  ( 1.847932960219115017, 115.7026903297836355, 1.721340370546041720 ) ) ;
#2343 = EDGE_LOOP ( 'NONE', ( #20259, #24315, #40824, #35579 ) ) ;
#2344 = CARTESIAN_POINT ( 'NONE',  ( -4.734376237147363220, 117.7615504634655252, -1.071976335040407902 ) ) ;
#2345 = CARTESIAN_POINT ( 'NONE',  ( 9.163388821854780986, 124.2347608867413413, 0.1831063163140474459 ) ) ;
#2346 = ORIENTED_EDGE ( 'NONE', *, *, #13172, .T. ) ;
#2347 = CARTESIAN_POINT ( 'NONE',  ( 19.42145995676300529, 149.0830822498907082, 2.502058577541587781 ) ) ;
#2348 = CARTESIAN_POINT ( 'NONE',  ( -6.431420355030265265E-14, 156.3034662015457172, 9.897580308537652682E-17 ) ) ;
#2349 = AXIS2_PLACEMENT_3D ( 'NONE', #22246, #26089, #344 ) ;
#2350 = PLANE ( 'NONE',  #8239 ) ;
#2351 = CARTESIAN_POINT ( 'NONE',  ( -17.14500000000466784, 71.11999999999886768, -1.524000000000000909 ) ) ;
#2352 = CARTESIAN_POINT ( 'NONE',  ( 15.92845220574645992, 121.2232988859741027, -0.005268350931750691128 ) ) ;
#2353 = CARTESIAN_POINT ( 'NONE',  ( -3.682264917456324671, 101.6934662015457320, -0.07358041635423923088 ) ) ;
#2354 = CARTESIAN_POINT ( 'NONE',  ( -12.16475753114683656, 55.74362973025081658, 5.016499999999999737 ) ) ;
#2355 = CARTESIAN_POINT ( 'NONE',  ( 1.871273403468687091, -15.33072671635390982, 5.367422375955600344 ) ) ;
#2356 = CARTESIAN_POINT ( 'NONE',  ( -16.46263872254443683, 83.91929436251373886, -1.524000000000002464 ) ) ;
#2357 = DIRECTION ( 'NONE',  ( -1.000000000000000000, -9.933992704233682996E-16, 0.000000000000000000 ) ) ;
#2358 = CARTESIAN_POINT ( 'NONE',  ( -4.892936701456676474, 117.7439554820887224, 0.7242864044084754704 ) ) ;
#2359 = ORIENTED_EDGE ( 'NONE', *, *, #37833, .F. ) ;
#2360 = CARTESIAN_POINT ( 'NONE',  ( -0.8085694520786111950, 118.7629491485454025, 1.239635759033087314 ) ) ;
#2361 = CARTESIAN_POINT ( 'NONE',  ( -5.604943360455993506, 118.2794056816863986, -1.161089605505309041 ) ) ;
#2362 = CARTESIAN_POINT ( 'NONE',  ( -4.076169972524864349, 117.8719421043398370, -0.8561738758874234412 ) ) ;
#2363 = CARTESIAN_POINT ( 'NONE',  ( 4.907969887652551932, 117.6281236953606566, 0.9703093435619695173 ) ) ;
#2364 = CARTESIAN_POINT ( 'NONE',  ( 3.187143392547471255, -14.52651900126690876, 3.212499789951002604 ) ) ;
#2365 = CARTESIAN_POINT ( 'NONE',  ( -0.8039382690413905408, 120.8419495465347069, 0.4447074479469317887 ) ) ;
#2366 = B_SPLINE_CURVE_WITH_KNOTS ( 'NONE', 3,
 ( #29855, #23016, #20041, #32421, #3675, #13026, #16639, #39027 ),
 .UNSPECIFIED., .F., .F.,
 ( 4, 2, 2, 4 ),
 ( -5.999999999990650338E-08, 0.002398869872785528400, 0.003598334809178291988, 0.004797799745571056443 ),
 .UNSPECIFIED. ) ;
#2367 = CARTESIAN_POINT ( 'NONE',  ( -4.595132424582489605, -6.828429371805166959, -0.5093739664528403877 ) ) ;
#2368 = CARTESIAN_POINT ( 'NONE',  ( -58.07447437077728125, 1.735896131820596766, 1.499107834811089557 ) ) ;
#2369 = DIRECTION ( 'NONE',  ( -1.224646799147353207E-16, 1.179012811983454535E-32, 1.000000000000000000 ) ) ;
#2370 = CARTESIAN_POINT ( 'NONE',  ( 3.449548791184131602, -12.83738641323306595, 1.613555780903996206 ) ) ;
#2371 = CARTESIAN_POINT ( 'NONE',  ( 7.070147686296559542, 122.4340714744230496, 0.03157745743911253428 ) ) ;
#2372 = CARTESIAN_POINT ( 'NONE',  ( -6.550279792842376381, 120.6599796251122427, -1.081144621291421082 ) ) ;
#2373 = CARTESIAN_POINT ( 'NONE',  ( 5.150502540934155604, 116.8624420608055630, -0.04745483869977647207 ) ) ;
#2374 = CARTESIAN_POINT ( 'NONE',  ( 0.1736941791105798827, 37.94092622093888423, 1.710797978410913300 ) ) ;
#2375 = CARTESIAN_POINT ( 'NONE',  ( -1.232253463169212360, 115.7029489552889601, 1.695155158364408665 ) ) ;
#2376 = CARTESIAN_POINT ( 'NONE',  ( -4.603678009535974169, 12.38766144714272066, -0.4343361176327051321 ) ) ;
#2378 = ORIENTED_EDGE ( 'NONE', *, *, #677, .T. ) ;
#2377 = CARTESIAN_POINT ( 'NONE',  ( 23.13755856728662508, 142.6111785389246336, 1.063510652947477153 ) ) ;
#2379 = CARTESIAN_POINT ( 'NONE',  ( 1.773199387803063853, 105.1239297914698625, -5.032115150572375128 ) ) ;
#2380 = CARTESIAN_POINT ( 'NONE',  ( 4.393930847168488363, -15.54918382657802312, 2.099248807845041309 ) ) ;
#2381 = CARTESIAN_POINT ( 'NONE',  ( -8.434619947227433912, 156.6436466068687423, 1.738452918000226610 ) ) ;
#2382 = CARTESIAN_POINT ( 'NONE',  ( 0.8148283262528154269, -11.57344599616632763, 0.5628321559398594687 ) ) ;
#2383 = CARTESIAN_POINT ( 'NONE',  ( -0.4102451260098727293, 24.68626973166569982, 0.8857237506759965129 ) ) ;
#2384 = EDGE_CURVE ( 'NONE', #36071, #117, #19612, .T. ) ;
#2385 = EDGE_CURVE ( 'NONE', #24894, #11397, #1295, .T. ) ;
#2386 = ORIENTED_EDGE ( 'NONE', *, *, #21078, .T. ) ;
#2387 = ORIENTED_EDGE ( 'NONE', *, *, #38483, .F. ) ;
#2388 = DIRECTION ( 'NONE',  ( -0.9876665170007968841, 0.1565721916417935344, -5.390917751951443929E-16 ) ) ;
#2389 = CARTESIAN_POINT ( 'NONE',  ( 3.997939770797755532, 117.2022048034790487, 1.046317678458332567 ) ) ;
#2390 = CARTESIAN_POINT ( 'NONE',  ( -16.36402192804845512, 147.4903123243063590, 0.9458667783343727153 ) ) ;
#2391 = DIRECTION ( 'NONE',  ( 6.353134868986659519E-16, -1.000000000000000000, 0.000000000000000000 ) ) ;
#2392 = CARTESIAN_POINT ( 'NONE',  ( 3.771727509258866906, -13.52648377956064429, 3.452274064300702605 ) ) ;
#2393 = CARTESIAN_POINT ( 'NONE',  ( 17.96630583390848912, 147.4621342421176848, -1.576657649719084064 ) ) ;
#2394 = CARTESIAN_POINT ( 'NONE',  ( -4.596153127770238100, 158.0471523224993859, -1.806220157282541150 ) ) ;
#2395 = DIRECTION ( 'NONE',  ( -5.206863593109713661E-17, 1.000000000000000000, -1.077750396879097183E-30 ) ) ;
#2396 = CARTESIAN_POINT ( 'NONE',  ( 2.994295736468014280, -14.77441112906794984, 3.968895097548184037 ) ) ;
#2397 = CARTESIAN_POINT ( 'NONE',  ( -0.008457519121241168295, 39.20946620154573026, 0.4232488410869258977 ) ) ;
#2398 = CARTESIAN_POINT ( 'NONE',  ( 0.6274479277950415490, 120.8480686026657196, -0.1451731132019951631 ) ) ;
#2399 = ORIENTED_EDGE ( 'NONE', *, *, #29542, .F. ) ;
#2400 = FACE_OUTER_BOUND ( 'NONE', #27885, .T. ) ;
#2401 = DIRECTION ( 'NONE',  ( -0.6559537821943223213, 0.7548010569845299278, -8.537024980200762654E-16 ) ) ;
#2402 = CARTESIAN_POINT ( 'NONE',  ( 1.733480476724572172, 35.69352191795299944, 2.306000102516378991 ) ) ;
#2403 = CARTESIAN_POINT ( 'NONE',  ( -58.30061145522722654, -0.1075020354536087575, 0.6732717543611356215 ) ) ;
#2404 = CARTESIAN_POINT ( 'NONE',  ( -2.276242205911199523, 25.81146128161704567, -8.137376054096339573 ) ) ;
#2405 = CARTESIAN_POINT ( 'NONE',  ( 12.69811389000554236, 152.1353413313561305, 1.627698677231679492 ) ) ;
#2406 = FACE_OUTER_BOUND ( 'NONE', #31534, .T. ) ;
#2407 = CARTESIAN_POINT ( 'NONE',  ( 5.755666581048775043, 159.1151184437813981, 0.09834937626042362935 ) ) ;
#2408 = CARTESIAN_POINT ( 'NONE',  ( -3.556334529073039707, 108.6891572770382624, 3.980722479600266706 ) ) ;
#2409 = CARTESIAN_POINT ( 'NONE',  ( 4.219463811995017188, -1.205994944679912306, -1.932895124392335573 ) ) ;
#2410 = CARTESIAN_POINT ( 'NONE',  ( 9.118174893680169646, 124.1671967267183589, 0.1822028344259500054 ) ) ;
#2411 = EDGE_CURVE ( 'NONE', #7919, #11738, #39022, .T. ) ;
#2412 = STYLED_ITEM ( 'NONE', ( #26181 ), #38952 ) ;
#2413 = CARTESIAN_POINT ( 'NONE',  ( 6.464508713081113633, 4.871470569706378484, -5.424950676754816570 ) ) ;
#2414 = CARTESIAN_POINT ( 'NONE',  ( -56.89020484191215132, 2.444072280526621288, -0.3054065742134425832 ) ) ;
#2415 = CARTESIAN_POINT ( 'NONE',  ( 5.543381447479352353, 116.8569150493630673, -0.3072380764452348201 ) ) ;
#2416 = CARTESIAN_POINT ( 'NONE',  ( -0.8524833535544004137, 121.9014879524050343, -0.3240522193994317401 ) ) ;
#2417 = DIRECTION ( 'NONE',  ( 0.9998004120163609398, 0.000000000000000000, 0.01997839162482749689 ) ) ;
#2418 = DIRECTION ( 'NONE',  ( 5.188838149069472160E-16, -1.699382548006136559E-16, -1.000000000000000000 ) ) ;
#2419 = CARTESIAN_POINT ( 'NONE',  ( 6.518667233416390872, -10.50300228728784901, -5.332001816399940530 ) ) ;
#2420 = CARTESIAN_POINT ( 'NONE',  ( 0.5321472206583588438, 118.1588881331645524, 0.9064177333157917849 ) ) ;
#2421 = CARTESIAN_POINT ( 'NONE',  ( 10.92199999999999704, 16.51000000000000156, 5.016499999999999737 ) ) ;
#2422 = CARTESIAN_POINT ( 'NONE',  ( -28.60507221318228943, 76.72702915747851193, 1.523999999999991806 ) ) ;
#2423 = CARTESIAN_POINT ( 'NONE',  ( 0.7818436192037604426, 120.2878791493615296, -0.5419007644741467011 ) ) ;
#2424 = CARTESIAN_POINT ( 'NONE',  ( -14.99898601413122812, 156.1447123740162226, 0.3355057415613001970 ) ) ;
#2425 = ORIENTED_EDGE ( 'NONE', *, *, #35443, .F. ) ;
#2426 = CARTESIAN_POINT ( 'NONE',  ( -58.75091225067960465, 0.1325880516401256592, -0.03773457465075338857 ) ) ;
#2427 = ORIENTED_EDGE ( 'NONE', *, *, #7427, .T. ) ;
#2428 = CARTESIAN_POINT ( 'NONE',  ( -41.28107547821695533, 23.22158991241120063, -1.524000000000005794 ) ) ;
#2429 = CARTESIAN_POINT ( 'NONE',  ( -0.6511158059023082201, 120.9972571290847156, 0.05313384682098968442 ) ) ;
#2430 = CARTESIAN_POINT ( 'NONE',  ( 4.717164877559400615, -15.39354034361711854, 4.072675418279473547 ) ) ;
#2431 = CARTESIAN_POINT ( 'NONE',  ( -19.23923079580238493, 135.9655892003723636, 1.583918808943347800 ) ) ;
#2432 = CARTESIAN_POINT ( 'NONE',  ( 14.20701772348842340, 121.1589565784038456, -0.8306491748466005021 ) ) ;
#2433 = CARTESIAN_POINT ( 'NONE',  ( -4.247245584637960647, 22.75789413176893206, 1.861891798430825862 ) ) ;
#2434 = EDGE_CURVE ( 'NONE', #33959, #31070, #23011, .T. ) ;
#2435 = CARTESIAN_POINT ( 'NONE',  ( -15.93800727448861210, 121.3860667298135070, -0.7466885930842023233 ) ) ;
#2436 = CARTESIAN_POINT ( 'NONE',  ( -55.85087417899054429, 5.582623226463158339, -2.873287190156892379 ) ) ;
#2437 = ORIENTED_EDGE ( 'NONE', *, *, #31655, .F. ) ;
#2438 = CARTESIAN_POINT ( 'NONE',  ( -0.005880675324201318707, 122.2435587914035295, 0.2942930402744693419 ) ) ;
#2439 = CARTESIAN_POINT ( 'NONE',  ( -4.466782427718574588, 71.06098887363195615, 1.270000000000004903 ) ) ;
#2440 = B_SPLINE_SURFACE_WITH_KNOTS ( 'NONE', 3, 1, ( 
 ( #6364, #2966 ),
 ( #22726, #38531 ),
 ( #26158, #13168 ),
 ( #15929, #28725 ) ),
 .UNSPECIFIED., .F., .F., .F.,
 ( 4, 4 ),
 ( 2, 2 ),
 ( 0.000000000000000000, 0.6118630412642164229 ),
 ( 0.000000000000000000, 1.000000000000000000 ),
 .UNSPECIFIED. ) ;
#2441 = CARTESIAN_POINT ( 'NONE',  ( -3.484775907859313904, 120.0787590019544098, 0.5801956493991066166 ) ) ;
#2442 = CARTESIAN_POINT ( 'NONE',  ( -53.77126677436539381, 9.275061619689314085, -3.554206636766655159 ) ) ;
#2443 = CARTESIAN_POINT ( 'NONE',  ( 18.94125265848531825, 149.4003703399637288, -1.737001818219200411 ) ) ;
#2444 = CARTESIAN_POINT ( 'NONE',  ( -3.077448401760676244, 117.9340107969418341, -0.8067720256249977240 ) ) ;
#2445 = CARTESIAN_POINT ( 'NONE',  ( -53.65759266121656879, 11.01975743955735432, -4.003319250743225588 ) ) ;
#2446 = EDGE_CURVE ( 'NONE', #33959, #30709, #40062, .T. ) ;
#2447 = CARTESIAN_POINT ( 'NONE',  ( 9.503290916780938957, 123.5188755717998816, -0.5781397488420938480 ) ) ;
#2448 = ORIENTED_EDGE ( 'NONE', *, *, #21122, .T. ) ;
#2449 = CARTESIAN_POINT ( 'NONE',  ( -7.499533598998470829, 156.0351187175861867, -1.911400249181836042 ) ) ;
#2450 = CARTESIAN_POINT ( 'NONE',  ( 4.161657294200716173, -15.28457189793756754, -0.5145498944859950852 ) ) ;
#2451 = CARTESIAN_POINT ( 'NONE',  ( -4.253023843880794352, 118.2240548184727089, -0.4605302936478082865 ) ) ;
#2452 = CARTESIAN_POINT ( 'NONE',  ( -58.43690671596436914, -0.4125963578781866037, -0.2423173958219211055 ) ) ;
#2453 = CARTESIAN_POINT ( 'NONE',  ( -4.854232772743657165, 117.4081466956269395, 0.9971777887500445914 ) ) ;
#2454 = CARTESIAN_POINT ( 'NONE',  ( 13.78929608597934831, 128.5353789189983900, 1.909663635655581615 ) ) ;
#2455 = CARTESIAN_POINT ( 'NONE',  ( -47.16908398257314872, 25.15707121737544938, 1.640988021989188805 ) ) ;
#2456 = CARTESIAN_POINT ( 'NONE',  ( -5.746845633966660039, 1.589972373264088246, -6.161128625535090109 ) ) ;
#2457 = CARTESIAN_POINT ( 'NONE',  ( 5.263358945736606564, 121.3020066425206807, 0.2711714534586360248 ) ) ;
#2458 = CARTESIAN_POINT ( 'NONE',  ( -58.83227707057486811, -0.08366279997995551554, -0.2458995907045101459 ) ) ;
#2459 = EDGE_CURVE ( 'NONE', #35057, #21265, #38404, .T. ) ;
#2461 = VERTEX_POINT ( 'NONE', #15793 ) ;
#2460 = DIRECTION ( 'NONE',  ( 0.8572391118119481179, 0.5149185422762151410, 0.000000000000000000 ) ) ;
#2462 = CARTESIAN_POINT ( 'NONE',  ( -0.4467517591321596981, 117.3993820567716142, 1.478547820748352448 ) ) ;
#2463 = CARTESIAN_POINT ( 'NONE',  ( -58.11258158571958177, 1.603013069906233934, 1.501710181103012465 ) ) ;
#2464 = CARTESIAN_POINT ( 'NONE',  ( -48.96082574602279180, 17.89581470837939747, 5.125304694085289547 ) ) ;
#2465 = CARTESIAN_POINT ( 'NONE',  ( -7.971903862541391383, 121.6201495393203800, -1.129789807432725279 ) ) ;
#2466 = EDGE_CURVE ( 'NONE', #35912, #359, #33547, .T. ) ;
#2467 = CARTESIAN_POINT ( 'NONE',  ( -5.965356522962950159, 77.01756249999996840, -5.016499999999999737 ) ) ;
#2468 = CARTESIAN_POINT ( 'NONE',  ( -51.41777536269126614, 18.15702087101736595, 2.173118852594992045 ) ) ;
#2469 = CARTESIAN_POINT ( 'NONE',  ( -8.048392397359151573, 158.6767594643193604, 0.003330354478299033406 ) ) ;
#2470 = VECTOR ( 'NONE', #25773, 999.9999999999998863 ) ;
#2471 = VERTEX_POINT ( 'NONE', #33268 ) ;
#2472 = CARTESIAN_POINT ( 'NONE',  ( -50.64083583777225073, 22.17031204481727258, -0.3653657693499831605 ) ) ;
#2473 = CARTESIAN_POINT ( 'NONE',  ( -6.036974320247253445, 121.4378217842577783, -0.1460419162834154239 ) ) ;
#2474 = DIRECTION ( 'NONE',  ( -1.000000000000000000, 9.627370216492862708E-17, 0.000000000000000000 ) ) ;
#2475 = EDGE_LOOP ( 'NONE', ( #14245, #27709 ) ) ;
#2476 = CARTESIAN_POINT ( 'NONE',  ( 2.411409958355576588, 115.7029272791032781, -1.607700095068150592 ) ) ;
#2477 = CARTESIAN_POINT ( 'NONE',  ( -1.577167647222679436, 156.2580631240469415, -0.1709568888171391354 ) ) ;
#2478 = CARTESIAN_POINT ( 'NONE',  ( 3.928490385995774936, -14.72231570353084429, 5.141255514400237203 ) ) ;
#2479 = CARTESIAN_POINT ( 'NONE',  ( -13.78108617287063353, 121.3979351292862816, 1.006787891297146409 ) ) ;
#2480 = DIRECTION ( 'NONE',  ( 0.000000000000000000, 0.000000000000000000, -1.000000000000000000 ) ) ;
#2481 = CARTESIAN_POINT ( 'NONE',  ( 15.16003043525265248, 156.1230782244120121, 0.5028385762316639473 ) ) ;
#2482 = CARTESIAN_POINT ( 'NONE',  ( 1.555436498865683026, 156.2615671560531609, 0.1081568999835344491 ) ) ;
#2483 = DIRECTION ( 'NONE',  ( -0.8745520943968250194, 0.4849315768086534528, -5.361993529360573944E-16 ) ) ;
#2484 = CARTESIAN_POINT ( 'NONE',  ( -0.9658880162092680077, 3.969362202269336226, 0.1338930134723784471 ) ) ;
#2485 = CARTESIAN_POINT ( 'NONE',  ( -3.714261611334668700, 116.6275173757784813, -0.1151834636560011560 ) ) ;
#2486 = CARTESIAN_POINT ( 'NONE',  ( -24.16603736854983708, 76.82831944025377879, 1.269999999999993801 ) ) ;
#2487 = PLANE ( 'NONE',  #4772 ) ;
#2488 = EDGE_CURVE ( 'NONE', #18952, #41795, #38005, .T. ) ;
#2489 = ORIENTED_EDGE ( 'NONE', *, *, #26047, .F. ) ;
#2490 = CARTESIAN_POINT ( 'NONE',  ( 8.375419374246291682, 119.6241210904774874, 1.419676489699448929 ) ) ;
#2491 = CARTESIAN_POINT ( 'NONE',  ( 4.409325496788552456, -14.99073161069602911, -1.440227693534741782 ) ) ;
#2492 = CARTESIAN_POINT ( 'NONE',  ( 13.41577631804572412, 120.9245410081625209, 1.450210030139598594 ) ) ;
#2493 = CARTESIAN_POINT ( 'NONE',  ( 6.603547431282811964, 157.6773268839678508, -1.653176294384505418 ) ) ;
#2494 = CARTESIAN_POINT ( 'NONE',  ( 1.818839793882075728, -13.69063247836898611, -4.255424433905749204 ) ) ;
#2495 = CARTESIAN_POINT ( 'NONE',  ( -18.89746971955500854, 128.6554162386474047, -1.621015360058189358 ) ) ;
#2496 = CARTESIAN_POINT ( 'NONE',  ( 4.772809636307222547, 117.7613819223621334, -0.8822393946220054017 ) ) ;
#2497 = CARTESIAN_POINT ( 'NONE',  ( 5.451337559846638037, 117.5214873295501405, 0.8265904065678292278 ) ) ;
#2498 = CARTESIAN_POINT ( 'NONE',  ( -15.74722489594621777, 146.9052959264698757, -0.08484200870240315995 ) ) ;
#2499 = CARTESIAN_POINT ( 'NONE',  ( -9.618126185770362824, 121.1143850344477215, -1.566364589618396197 ) ) ;
#2500 = CARTESIAN_POINT ( 'NONE',  ( 3.779930934242227369, -15.54964480308611208, 5.049599803682278676 ) ) ;
#2501 = CARTESIAN_POINT ( 'NONE',  ( 4.732128828421237721, 118.5931160184169073, 1.019631307593062974 ) ) ;
#2502 = AXIS2_PLACEMENT_3D ( 'NONE', #22755, #650, #20408 ) ;
#2503 = CARTESIAN_POINT ( 'NONE',  ( -36.43259636504752308, 28.15155085495446485, -1.524000000000003352 ) ) ;
#2504 = EDGE_CURVE ( 'NONE', #35500, #30610, #27110, .T. ) ;
#2506 = ORIENTED_EDGE ( 'NONE', *, *, #18795, .T. ) ;
#2505 = VECTOR ( 'NONE', #1415, 1000.000000000000114 ) ;
#2507 = CARTESIAN_POINT ( 'NONE',  ( 0.4867666382966649441, 119.1670848682014281, 0.5956043695837971441 ) ) ;
#2508 = SURFACE_STYLE_USAGE ( .BOTH. , #31667 ) ;
#2509 = CARTESIAN_POINT ( 'NONE',  ( 4.701335245683265995, 117.7901595215496258, 1.087246424278794477 ) ) ;
#2510 = CARTESIAN_POINT ( 'NONE',  ( -2.738288815229088069, 121.4869043954268903, 0.2316524989510643784 ) ) ;
#2511 = CARTESIAN_POINT ( 'NONE',  ( 8.265420891810833837, -5.467761657695628053, -1.740095136296691214 ) ) ;
#2512 = CARTESIAN_POINT ( 'NONE',  ( 12.19070665030413281, 151.9982576965888654, 1.154562729007634792 ) ) ;
#2513 = CARTESIAN_POINT ( 'NONE',  ( -41.18107378286554621, 22.95619949144852967, -1.523999999999998023 ) ) ;
#2514 = CARTESIAN_POINT ( 'NONE',  ( 22.99243123797615951, 146.5883926500602001, -0.5216133500896583675 ) ) ;
#2515 = DIRECTION ( 'NONE',  ( -5.188838149069472160E-16, 1.699382548006136559E-16, 1.000000000000000000 ) ) ;
#2516 = CARTESIAN_POINT ( 'NONE',  ( -58.13732371667832410, 0.2071221698984457016, 0.6618190132251328128 ) ) ;
#2517 = CARTESIAN_POINT ( 'NONE',  ( 5.652760403059779115, 78.90762248850970195, 4.881857480398483773 ) ) ;
#2518 = EDGE_CURVE ( 'NONE', #38485, #22696, #17475, .T. ) ;
#2519 = DIRECTION ( 'NONE',  ( -0.8745520943968243532, 0.4849315768086547296, -6.829619984160642269E-16 ) ) ;
#2520 = CARTESIAN_POINT ( 'NONE',  ( 5.149530563680449369, 114.9388725758769709, -1.533339281550282207 ) ) ;
#2521 = EDGE_CURVE ( 'NONE', #19034, #29525, #10668, .T. ) ;
#2522 = ORIENTED_EDGE ( 'NONE', *, *, #33625, .T. ) ;
#2523 = CARTESIAN_POINT ( 'NONE',  ( -58.50860430493789721, 0.7049166599848305514, 0.9756837515128383709 ) ) ;
#2524 = CARTESIAN_POINT ( 'NONE',  ( 4.622740841563977021, 119.7018045729082587, -0.7338303597469464368 ) ) ;
#2525 = CARTESIAN_POINT ( 'NONE',  ( -0.6715300310780568660, 105.9424719104300436, -5.313162126831953103 ) ) ;
#2526 = CIRCLE ( 'NONE', #26406, 0.2540000000000013913 ) ;
#2527 = CARTESIAN_POINT ( 'NONE',  ( -7.694217360203188250, 122.2455405838764335, -0.6631844599531893092 ) ) ;
#2528 = CARTESIAN_POINT ( 'NONE',  ( -7.917360960270791281, 70.00264313970245666, 1.270000000000003348 ) ) ;
#2529 = CARTESIAN_POINT ( 'NONE',  ( 23.44919332464148454, 146.8469795362756258, 0.4944523877934686173 ) ) ;
#2530 = ORIENTED_EDGE ( 'NONE', *, *, #33905, .T. ) ;
#2531 = CARTESIAN_POINT ( 'NONE',  ( 1.325333094648095011, 19.28447512809159292, -4.440015753949128730 ) ) ;
#2532 = CARTESIAN_POINT ( 'NONE',  ( -29.35321563035234149, 61.36487289460320227, 1.269999999999993801 ) ) ;
#2533 = CARTESIAN_POINT ( 'NONE',  ( -5.008697454415233175, 117.3984623471881292, 0.7756180019310896512 ) ) ;
#2534 = LINE ( 'NONE', #37667, #7479 ) ;
#2535 = CIRCLE ( 'NONE', #502, 0.7620000000000015650 ) ;
#2536 = CARTESIAN_POINT ( 'NONE',  ( -28.76494711669534610, 76.52965637509277030, -1.524000000000007793 ) ) ;
#2537 = CARTESIAN_POINT ( 'NONE',  ( -6.991991784399644416, 121.9291801892613734, 0.01265143332250801347 ) ) ;
#2538 = CARTESIAN_POINT ( 'NONE',  ( -4.295268622494708310, 18.69437521248495671, 1.722957355393906598 ) ) ;
#2539 = CARTESIAN_POINT ( 'NONE',  ( 3.132853369507592411, 159.3671203531505114, 0.7742396785067985343 ) ) ;
#2540 = CARTESIAN_POINT ( 'NONE',  ( -26.42106975583004314, 72.48669692073261217, 1.269999999999993356 ) ) ;
#2542 = CARTESIAN_POINT ( 'NONE',  ( 12.10120965742738441, 156.5645100661158153, -1.400626166162074693 ) ) ;
#2541 = CARTESIAN_POINT ( 'NONE',  ( 2.969447359227861405, -13.80100253337253946, 0.9847735008004718793 ) ) ;
#2543 = CARTESIAN_POINT ( 'NONE',  ( -15.45240368193238290, 131.3329289045130679, 1.560586129702050684 ) ) ;
#2544 = CARTESIAN_POINT ( 'NONE',  ( 1.027636191897724816, 24.96647085856908532, -4.506105791511280323 ) ) ;
#2545 = CARTESIAN_POINT ( 'NONE',  ( -20.30524341716979464, 152.5255278361454145, -1.346157490925044220 ) ) ;
#2546 = CARTESIAN_POINT ( 'NONE',  ( -0.9748693424575083366, -1.807339741155509660, 0.05984739681150109264 ) ) ;
#2547 = ORIENTED_EDGE ( 'NONE', *, *, #22871, .F. ) ;
#2548 = CARTESIAN_POINT ( 'NONE',  ( -56.42052199906244425, 3.302738315264078128, 0.3606658556335657906 ) ) ;
#2549 = CARTESIAN_POINT ( 'NONE',  ( -5.244198393876603248, 121.2166884500396833, 0.1799464770355448662 ) ) ;
#2550 = CARTESIAN_POINT ( 'NONE',  ( 3.373230072307711325, -14.96631539557509427, 5.513067843180951222 ) ) ;
#2551 = CARTESIAN_POINT ( 'NONE',  ( 16.86000824444443325, 147.6865045845431723, -1.246329746872388622 ) ) ;
#2552 = ORIENTED_EDGE ( 'NONE', *, *, #20644, .F. ) ;
#2553 = CARTESIAN_POINT ( 'NONE',  ( 0.8518381835474642116, 115.7029491485453150, 1.752614281141236852 ) ) ;
#2554 = VECTOR ( 'NONE', #26088, 1000.000000000000000 ) ;
#2555 = CARTESIAN_POINT ( 'NONE',  ( -4.745317454387270040, 117.7319129980786840, -1.087429732257703119 ) ) ;
#2556 = CARTESIAN_POINT ( 'NONE',  ( 8.041889123127029748, 122.8518031662551948, 0.1606960833125207211 ) ) ;
#2557 = ORIENTED_EDGE ( 'NONE', *, *, #17066, .T. ) ;
#2558 = CARTESIAN_POINT ( 'NONE',  ( 2.271387047178972995, 118.5910164976458532, 0.7981300483413861224 ) ) ;
#2559 = CARTESIAN_POINT ( 'NONE',  ( 1.650612623617701454E-15, 17.14499999999999957, 0.000000000000000000 ) ) ;
#2560 = AXIS2_PLACEMENT_3D ( 'NONE', #26322, #10762, #36974 ) ;
#2561 = DIRECTION ( 'NONE',  ( 0.000000000000000000, -0.000000000000000000, -1.000000000000000000 ) ) ;
#2562 = CARTESIAN_POINT ( 'NONE',  ( 0.004910621514677531059, 156.3161161488371533, -0.2457475809811480449 ) ) ;
#2563 = VECTOR ( 'NONE', #17486, 1000.000000000000114 ) ;
#2564 = CARTESIAN_POINT ( 'NONE',  ( 15.71820687823851159, 121.0099257824619627, -0.007297392930742286829 ) ) ;
#2565 = DIRECTION ( 'NONE',  ( -0.8745520943968235761, 0.4849315768086558398, -5.691349986800547879E-16 ) ) ;
#2566 = CARTESIAN_POINT ( 'NONE',  ( -46.93533292561973269, 25.16125026830412281, 1.870414060841448567 ) ) ;
#2567 = CARTESIAN_POINT ( 'NONE',  ( 5.237865101059586692, 78.94033958618257429, 5.314315937239232568 ) ) ;
#2569 = EDGE_CURVE ( 'NONE', #18840, #37319, #31325, .T. ) ;
#2568 = CARTESIAN_POINT ( 'NONE',  ( 1.999402950501548482, -15.06364915300781249, 5.759057916224358920 ) ) ;
#2570 = CARTESIAN_POINT ( 'NONE',  ( -42.79661761208809168, 21.81806929429799879, 2.089873509012810882 ) ) ;
#2571 = CARTESIAN_POINT ( 'NONE',  ( -20.79116009376201291, 79.67004825550966984, -1.524000000000004018 ) ) ;
#2572 = CARTESIAN_POINT ( 'NONE',  ( -4.623643573307993471, 118.0606194745544997, 0.5411930361001372480 ) ) ;
#2573 = ORIENTED_EDGE ( 'NONE', *, *, #27983, .T. ) ;
#2574 = CARTESIAN_POINT ( 'NONE',  ( -1.110165644321341460, 118.7629491485454025, 1.217933052008355554 ) ) ;
#2575 = CARTESIAN_POINT ( 'NONE',  ( 6.006868049574960899, 119.2300460209637407, -1.027315805567093898 ) ) ;
#2576 = CARTESIAN_POINT ( 'NONE',  ( -1.786380800136868618, 106.8720524443079967, -4.898415999051429992 ) ) ;
#2577 = CARTESIAN_POINT ( 'NONE',  ( 4.760004222690300324, 117.7660308155148385, 1.056159522374921167 ) ) ;
#2578 = DIRECTION ( 'NONE',  ( -5.188838149069472160E-16, 1.699382548006136559E-16, 1.000000000000000000 ) ) ;
#2579 = CARTESIAN_POINT ( 'NONE',  ( -0.3799753109755704683, 121.9236798544226730, 0.3295597595137201297 ) ) ;
#2580 = AXIS2_PLACEMENT_3D ( 'NONE', #3590, #3800, #33186 ) ;
#2581 = CARTESIAN_POINT ( 'NONE',  ( 3.745621265272091716, -10.50169880513956322, -2.708184146228840294 ) ) ;
#2582 = CARTESIAN_POINT ( 'NONE',  ( 4.853781638280933564, 117.4081357529187528, -0.9972794204146671060 ) ) ;
#2583 = DIRECTION ( 'NONE',  ( -0.000000000000000000, -0.000000000000000000, -1.000000000000000000 ) ) ;
#2584 = CARTESIAN_POINT ( 'NONE',  ( 2.741226102065047687, 109.4146836159258669, -3.767795064178312892 ) ) ;
#2585 = CARTESIAN_POINT ( 'NONE',  ( -17.50754485026813256, 146.9817191466759141, -2.164442782320840308 ) ) ;
#2586 = CARTESIAN_POINT ( 'NONE',  ( 6.075452776647331632, 121.4405985945170130, 0.1207385346877154486 ) ) ;
#2587 = CARTESIAN_POINT ( 'NONE',  ( -1.386537629721184883, 36.36735770096321829, 2.585368322340788172 ) ) ;
#2588 = CARTESIAN_POINT ( 'NONE',  ( -3.567118561776222219, 115.7029539238351816, 1.489719890727359441 ) ) ;
#2589 = CARTESIAN_POINT ( 'NONE',  ( -3.609430071560130848, 3.966570591990036032, 2.889066364458971137 ) ) ;
#2591 = VERTEX_POINT ( 'NONE', #36671 ) ;
#2590 = CARTESIAN_POINT ( 'NONE',  ( 14.49621620279156708, 120.3567457872619997, 0.7930654045677066888 ) ) ;
#2592 = CARTESIAN_POINT ( 'NONE',  ( 1.151853689421055149, 104.6144662015457811, -4.696227499264772121 ) ) ;
#2593 = CARTESIAN_POINT ( 'NONE',  ( 3.754758974503722868, -15.60599068302642678, 3.401513958955031836 ) ) ;
#2594 = CARTESIAN_POINT ( 'NONE',  ( -12.19007131875819283, 155.0146010091537221, 1.747022140133383417 ) ) ;
#2595 = CARTESIAN_POINT ( 'NONE',  ( -0.8611515851325071136, 16.54815110656625166, -0.4551624184793268135 ) ) ;
#2596 = CARTESIAN_POINT ( 'NONE',  ( 0.7643174330569572072, 9.588751494893990923, -0.6113830025413525826 ) ) ;
#2597 = ORIENTED_EDGE ( 'NONE', *, *, #13418, .F. ) ;
#2598 = EDGE_LOOP ( 'NONE', ( #15570, #5040, #12685, #2552 ) ) ;
#2599 = DIRECTION ( 'NONE',  ( -0.01997839162482749342, -1.040247600000944484E-18, 0.9998004120163608288 ) ) ;
#2600 = CARTESIAN_POINT ( 'NONE',  ( 2.588518934355891865, 109.4146836159258669, 3.874296054094246600 ) ) ;
#2601 = SURFACE_STYLE_FILL_AREA ( #38160 ) ;
#2602 = CARTESIAN_POINT ( 'NONE',  ( -4.675694769581217436, 155.9604050671876792, 0.8934998238159543860 ) ) ;
#2603 = DIRECTION ( 'NONE',  ( 0.9998004120163610509, 5.205824365704083805E-17, 0.01997839162482760444 ) ) ;
#2604 = CARTESIAN_POINT ( 'NONE',  ( 3.213330078112610177, -12.77372567451348573, 1.108568753689092690 ) ) ;
#2605 = CARTESIAN_POINT ( 'NONE',  ( 16.98580377952195875, 140.1729163700083518, -1.602912605581681582 ) ) ;
#2606 = CARTESIAN_POINT ( 'NONE',  ( -18.80649797369244425, 150.3568762430427910, -2.459390564378663768 ) ) ;
#2607 = LINE ( 'NONE', #15566, #39955 ) ;
#2608 = CARTESIAN_POINT ( 'NONE',  ( 7.971934240893917334, 121.6199950850121496, 1.129854539203151154 ) ) ;
#2609 = CARTESIAN_POINT ( 'NONE',  ( 4.074910602682932925, 118.2429491485453354, -0.1454311599470142491 ) ) ;
#2610 = CARTESIAN_POINT ( 'NONE',  ( 15.77919907218838702, 145.7191243368997675, -0.01646358168407709502 ) ) ;
#2611 = ORIENTED_EDGE ( 'NONE', *, *, #26308, .F. ) ;
#2612 = CARTESIAN_POINT ( 'NONE',  ( 2.768561164044480272, -13.57843041371762460, 0.3119852368007841603 ) ) ;
#2613 = FACE_BOUND ( 'NONE', #9801, .T. ) ;
#2614 = DIRECTION ( 'NONE',  ( 0.8745520943968240202, -0.4849315768086551182, 4.268512490100404500E-16 ) ) ;
#2615 = CARTESIAN_POINT ( 'NONE',  ( -58.66375602224792374, -0.3143320623662654301, 0.3221285174457437228 ) ) ;
#2616 = CARTESIAN_POINT ( 'NONE',  ( -6.895871986696200828, 19.14539577913392066, 4.887076909655228896 ) ) ;
#2617 = CARTESIAN_POINT ( 'NONE',  ( 11.45052794940109742, 153.2879862121713757, 1.711174725579351685 ) ) ;
#2618 = CARTESIAN_POINT ( 'NONE',  ( -13.79703500197642896, 79.79115557309579287, -1.524000000000000687 ) ) ;
#2619 = CARTESIAN_POINT ( 'NONE',  ( 23.40703704692311504, 142.8142681763856388, 0.3922439843285879801 ) ) ;
#2620 = CARTESIAN_POINT ( 'NONE',  ( -4.828659834973932696, 112.7831754354443348, 2.372633244901563465 ) ) ;
#2621 = CIRCLE ( 'NONE', #15417, 0.2539999999999967839 ) ;
#2622 = DIRECTION ( 'NONE',  ( 0.000000000000000000, 0.000000000000000000, -1.000000000000000000 ) ) ;
#2623 = CARTESIAN_POINT ( 'NONE',  ( 15.52687642492882070, 147.5330934759543879, 0.3102639428822866474 ) ) ;
#2624 = CARTESIAN_POINT ( 'NONE',  ( 5.057098040335121780, -7.207523253290371024, 6.778223571298113370 ) ) ;
#2625 = CARTESIAN_POINT ( 'NONE',  ( 8.758500698815293362, 117.9284149219992912, -0.3497163369972981495 ) ) ;
#2626 = CARTESIAN_POINT ( 'NONE',  ( 0.07831152689639594988, 109.4728569552520838, -3.919029035233729363 ) ) ;
#2627 = DIRECTION ( 'NONE',  ( -0.6825627711659453256, -0.7308269722843194760, -2.299753143848296480E-16 ) ) ;
#2628 = CARTESIAN_POINT ( 'NONE',  ( -5.266289895157169814E-14, 83.56599999999998829, 1.904999999999999805 ) ) ;
#2629 = CARTESIAN_POINT ( 'NONE',  ( 8.408789229792210662, -11.58028725773715628, 0.1531400924992341317 ) ) ;
#2630 = CARTESIAN_POINT ( 'NONE',  ( 0.1815206473440567347, 118.1588882195315477, 0.9095569039822347657 ) ) ;
#2631 = PLANE ( 'NONE',  #39625 ) ;
#2632 = CARTESIAN_POINT ( 'NONE',  ( 3.205266406700632675, -14.32095172213143641, 3.103221849221895035 ) ) ;
#2633 = CARTESIAN_POINT ( 'NONE',  ( 0.3786798576916004522, 121.5961256765096152, -0.3764709079149203830 ) ) ;
#2634 = CARTESIAN_POINT ( 'NONE',  ( -13.17783411699405605, 156.9583929045107595, 0.4564371790988702715 ) ) ;
#2635 = ORIENTED_EDGE ( 'NONE', *, *, #39644, .T. ) ;
#2636 = CARTESIAN_POINT ( 'NONE',  ( -17.14500000000466784, 71.11999999999886768, -1.270000000000000684 ) ) ;
#2637 = ORIENTED_EDGE ( 'NONE', *, *, #17533, .T. ) ;
#2638 = FACE_BOUND ( 'NONE', #27144, .T. ) ;
#2639 = CARTESIAN_POINT ( 'NONE',  ( -5.961919564881704936, 121.5457840906684908, -0.04491390701585241951 ) ) ;
#2640 = CARTESIAN_POINT ( 'NONE',  ( 2.074264724554232053, -15.58053249244904848, 5.900626476732238501 ) ) ;
#2641 = CARTESIAN_POINT ( 'NONE',  ( -11.80709641148050437, 120.8928578745602209, 1.148978701482600062 ) ) ;
#2642 = CARTESIAN_POINT ( 'NONE',  ( 14.55736095115755724, 121.4416029531759591, -0.8377414905974124304 ) ) ;
#2643 = CARTESIAN_POINT ( 'NONE',  ( -1.544744425833544099, 4.816215111148435923, 4.377641278133862279 ) ) ;
#2644 = CARTESIAN_POINT ( 'NONE',  ( -53.83244890055875231, 9.568295475555508744, -3.789950525193721109 ) ) ;
#2645 = ORIENTED_EDGE ( 'NONE', *, *, #24067, .T. ) ;
#2646 = DIRECTION ( 'NONE',  ( -1.000000000000000000, 1.044409991968847425E-16, 0.000000000000000000 ) ) ;
#2647 = CARTESIAN_POINT ( 'NONE',  ( -5.517349593794012463, 28.10803576007639037, 0.4164286583522215368 ) ) ;
#2648 = CARTESIAN_POINT ( 'NONE',  ( -9.755129750886823103, 122.6450757329969434, 0.9482731561257335962 ) ) ;
#2649 = DIRECTION ( 'NONE',  ( -0.08582482245076952787, -4.468781434041244531E-18, -0.9963102427714443099 ) ) ;
#2650 = VECTOR ( 'NONE', #16472, 1000.000000000000000 ) ;
#2651 = CARTESIAN_POINT ( 'NONE',  ( 18.65843730539381085, 148.7425187291823363, -1.723213218779726441 ) ) ;
#2652 = VECTOR ( 'NONE', #2483, 1000.000000000000227 ) ;
#2653 = CARTESIAN_POINT ( 'NONE',  ( -4.923251988582253880, 158.4862278396301178, -1.623903838676621358 ) ) ;
#2654 = CARTESIAN_POINT ( 'NONE',  ( -53.75224695799815322, 9.373383622779334345, -3.688627211158436392 ) ) ;
#2655 = CARTESIAN_POINT ( 'NONE',  ( 8.332953031246793429, 122.7091975629380585, -0.3740907431100289893 ) ) ;
#2656 = ORIENTED_EDGE ( 'NONE', *, *, #19285, .F. ) ;
#2657 = CARTESIAN_POINT ( 'NONE',  ( -18.11030164959035815, 147.2296321676236062, -2.344458923443068166 ) ) ;
#2658 = CARTESIAN_POINT ( 'NONE',  ( 3.256234316240316229, -15.49904601598017706, 3.966862439782909533 ) ) ;
#2659 = CARTESIAN_POINT ( 'NONE',  ( -4.065972646788793554, 118.2429491485453070, -0.3080848862740693250 ) ) ;
#2660 = CARTESIAN_POINT ( 'NONE',  ( -58.11144429832075531, 0.1746852717545294142, -1.017628075538466478E-14 ) ) ;
#2661 = CARTESIAN_POINT ( 'NONE',  ( -4.866475353371516377, 117.6758284370217211, 0.8741549091480164124 ) ) ;
#2662 = CARTESIAN_POINT ( 'NONE',  ( 17.54535662205662305, 147.9903219242534078, 2.232389162988360987 ) ) ;
#2663 = CARTESIAN_POINT ( 'NONE',  ( 1.122158211225882551, 34.81801111161350804, -0.09678150280622697943 ) ) ;
#2664 = ADVANCED_FACE ( 'NONE', ( #20872 ), #29642, .T. ) ;
#2665 = CARTESIAN_POINT ( 'NONE',  ( -2.029258473809828711, 23.83235028914373288, 4.157303687431403993 ) ) ;
#2666 = CARTESIAN_POINT ( 'NONE',  ( 13.62587875280878613, 150.2122286517991085, 0.5925390977946543014 ) ) ;
#2667 = CYLINDRICAL_SURFACE ( 'NONE', #3162, 0.2540000000000046665 ) ;
#2668 = AXIS2_PLACEMENT_3D ( 'NONE', #38146, #31316, #11937 ) ;
#2670 = VERTEX_POINT ( 'NONE', #11091 ) ;
#2669 = CARTESIAN_POINT ( 'NONE',  ( -47.44699234454018466, 15.94620872345373108, -7.864955498886620583E-15 ) ) ;
#2671 = CARTESIAN_POINT ( 'NONE',  ( -1.049266738966821100, 117.3993836600691338, 1.438942573323084062 ) ) ;
#2672 = CLOSED_SHELL ( 'NONE', ( #32343, #838, #24751, #2283, #1696, #39917, #26378, #30390 ) ) ;
#2673 = CARTESIAN_POINT ( 'NONE',  ( -58.10099831372669854, 0.3475205698689753930, 0.9728495803591148405 ) ) ;
#2674 = CARTESIAN_POINT ( 'NONE',  ( -54.68081972647571831, 7.927468599487359491, 3.439372298942311446 ) ) ;
#2675 = CARTESIAN_POINT ( 'NONE',  ( -30.15519950990045572, 69.97033940222175374, -1.270000000000007123 ) ) ;
#2676 = DIRECTION ( 'NONE',  ( -5.188838149069472160E-16, 1.699382548006136559E-16, 1.000000000000000000 ) ) ;
#2677 = CARTESIAN_POINT ( 'NONE',  ( -50.15972161391663064, 17.13814111569222121, 4.955022299345066550 ) ) ;
#2678 = ADVANCED_FACE ( 'NONE', ( #33479 ), #7528, .F. ) ;
#2679 = CARTESIAN_POINT ( 'NONE',  ( -21.89150648822684175, 151.4414241944827495, -0.2106634337039129667 ) ) ;
#2680 = ORIENTED_EDGE ( 'NONE', *, *, #14971, .F. ) ;
#2681 = CARTESIAN_POINT ( 'NONE',  ( -47.97936104919185851, 23.38005451144316993, -1.568716696360817675 ) ) ;
#2682 = CARTESIAN_POINT ( 'NONE',  ( 6.944753498707676442, 121.9193963520664568, -0.07675506838304683999 ) ) ;
#2683 = CARTESIAN_POINT ( 'NONE',  ( -23.09297118196009890, 77.93920196072180318, 1.269999999999994023 ) ) ;
#2684 = ORIENTED_EDGE ( 'NONE', *, *, #3283, .T. ) ;
#2685 = CARTESIAN_POINT ( 'NONE',  ( 1.944750467032260843, 115.7029431225055447, -1.643889904354718601 ) ) ;
#2686 = CARTESIAN_POINT ( 'NONE',  ( -11.96249418807715337, 130.4318746828361100, -0.4433914376541253088 ) ) ;
#2687 = CARTESIAN_POINT ( 'NONE',  ( 5.272318886577700425, -12.73938755324596706, 2.198237985477529577 ) ) ;
#2688 = CARTESIAN_POINT ( 'NONE',  ( -4.947803190686721919, 118.0342071775839941, 0.7636311594363676125 ) ) ;
#2689 = FACE_OUTER_BOUND ( 'NONE', #1162, .T. ) ;
#2690 = CARTESIAN_POINT ( 'NONE',  ( 15.38042280020263597, 120.6961994932685798, 0.5371754898667550071 ) ) ;
#2691 = CARTESIAN_POINT ( 'NONE',  ( 15.52499971488611052, 147.5364857366073750, 0.4437653257291759856 ) ) ;
#2692 = CARTESIAN_POINT ( 'NONE',  ( -4.886900518740532995, 117.7626867099871930, 0.6841186648097229428 ) ) ;
#2693 = CARTESIAN_POINT ( 'NONE',  ( -0.9549105556349912760, 13.03813504644791976, -0.2014467441264284064 ) ) ;
#2694 = CARTESIAN_POINT ( 'NONE',  ( -23.10830587629928701, 149.8995197111492814, -0.5387578213853484455 ) ) ;
#2695 = CARTESIAN_POINT ( 'NONE',  ( 12.21488373879589240, 71.11999999999999034, 5.016499999999999737 ) ) ;
#2696 = CARTESIAN_POINT ( 'NONE',  ( 5.177913976931201923, 71.67999986514567468, -5.372100000000002318 ) ) ;
#2697 = ORIENTED_EDGE ( 'NONE', *, *, #29178, .F. ) ;
#2698 = CARTESIAN_POINT ( 'NONE',  ( -5.639246004011813973, 117.7088169978700165, 0.7550884821962456916 ) ) ;
#2699 = ADVANCED_FACE ( 'NONE', ( #3885 ), #22115, .T. ) ;
#2700 = CARTESIAN_POINT ( 'NONE',  ( -58.35383657723647843, -0.2581369473864316699, -0.1573926582942791197 ) ) ;
#2701 = CARTESIAN_POINT ( 'NONE',  ( 17.24095835932491383, 153.8449085212272678, 1.984086636893841460 ) ) ;
#2702 = CARTESIAN_POINT ( 'NONE',  ( 13.96578288426879944, 123.5874490550988014, -1.342688313448305415 ) ) ;
#2703 = CARTESIAN_POINT ( 'NONE',  ( -8.202033116754899211, 17.84503447943221843, -1.958624548878737492 ) ) ;
#2704 = CARTESIAN_POINT ( 'NONE',  ( -22.06201951068911882, 142.1041199125429557, -1.893492075525809115 ) ) ;
#2705 = CARTESIAN_POINT ( 'NONE',  ( 4.712915829303078397, 117.8947333706760645, -0.7958967948868717057 ) ) ;
#2706 = CARTESIAN_POINT ( 'NONE',  ( 5.402623002109011807, 117.1681999988027911, 0.9004238350613811281 ) ) ;
#2707 = EDGE_CURVE ( 'NONE', #32109, #11189, #16941, .T. ) ;
#2708 = CARTESIAN_POINT ( 'NONE',  ( -4.236260012103463701, 155.8470599587123502, 0.007037385900262245995 ) ) ;
#2709 = CARTESIAN_POINT ( 'NONE',  ( -7.518309192797278051, 120.1328256275108828, -1.363123692563724232 ) ) ;
#2710 = EDGE_CURVE ( 'NONE', #1116, #5222, #5495, .T. ) ;
#2712 = CARTESIAN_POINT ( 'NONE',  ( 5.755466747078162193, -14.97439463182292840, 1.832642420680269613 ) ) ;
#2711 = AXIS2_PLACEMENT_3D ( 'NONE', #25509, #5513, #21659 ) ;
#2713 = CARTESIAN_POINT ( 'NONE',  ( 4.787502628886421974, 118.5931160184169073, 0.9394847329858636575 ) ) ;
#2714 = EDGE_CURVE ( 'NONE', #19419, #30834, #21788, .T. ) ;
#2715 = CARTESIAN_POINT ( 'NONE',  ( -3.116415352288768759, 118.1651002505946764, -0.7896273181905824057 ) ) ;
#2716 = EDGE_LOOP ( 'NONE', ( #13515, #30906, #40079, #3146, #16029 ) ) ;
#2717 = CARTESIAN_POINT ( 'NONE',  ( 18.92921826512563754, 147.2511928822236769, 2.484298966539742359 ) ) ;
#2718 = CARTESIAN_POINT ( 'NONE',  ( -15.72550100231844006, 145.6881679641599021, -0.3142329346387510713 ) ) ;
#2719 = DIRECTION ( 'NONE',  ( -0.000000000000000000, -0.000000000000000000, -1.000000000000000000 ) ) ;
#2720 = CARTESIAN_POINT ( 'NONE',  ( -5.284455934300128277, 122.2451909684448310, 0.05007199584899540284 ) ) ;
#2721 = CARTESIAN_POINT ( 'NONE',  ( -5.729511908840139611, -2.247816343263548511, -6.181412921048518250 ) ) ;
#2722 = CARTESIAN_POINT ( 'NONE',  ( 13.47315239181489055, 134.2048320552371763, 1.097568958570526387 ) ) ;
#2723 = CARTESIAN_POINT ( 'NONE',  ( 13.17783411699392815, 156.9583929045107595, -0.4564371790988700495 ) ) ;
#2724 = CARTESIAN_POINT ( 'NONE',  ( 5.353961913965608055, 57.14999999999869829, -5.213928161019547147 ) ) ;
#2725 = CARTESIAN_POINT ( 'NONE',  ( -58.28013857485719029, -0.1013628303895854899, 0.3875891849807499567 ) ) ;
#2726 = CARTESIAN_POINT ( 'NONE',  ( -2.177780859526504464, 116.2183971991849063, -0.1591026366872899112 ) ) ;
#2728 = FACE_OUTER_BOUND ( 'NONE', #31465, .T. ) ;
#2727 = VECTOR ( 'NONE', #26317, 1000.000000000000000 ) ;
#2729 = CARTESIAN_POINT ( 'NONE',  ( -14.91134437181082717, 120.3281135998953459, -0.2979641475761141134 ) ) ;
#2730 = ORIENTED_EDGE ( 'NONE', *, *, #25110, .T. ) ;
#2731 = CIRCLE ( 'NONE', #26532, 12.69999999999999751 ) ;
#2732 = CARTESIAN_POINT ( 'NONE',  ( -4.472347561024065499, 119.5957418731920825, -0.9224546268043867236 ) ) ;
#2733 = CARTESIAN_POINT ( 'NONE',  ( -5.329475387727676150, 116.0444662015457311, -0.2797177882896795809 ) ) ;
#2734 = CARTESIAN_POINT ( 'NONE',  ( -8.743035643995797912, 123.3024417045633498, -0.5730362264965973562 ) ) ;
#2735 = CARTESIAN_POINT ( 'NONE',  ( -6.997652642833405601, 121.9526520506185676, -0.1398297539000763479 ) ) ;
#2736 = CARTESIAN_POINT ( 'NONE',  ( 22.76738278397251136, 137.3906169244638136, 0.4549464913834384561 ) ) ;
#2737 = VERTEX_POINT ( 'NONE', #27162 ) ;
#2738 = CARTESIAN_POINT ( 'NONE',  ( -0.8823465807374654135, 5.041073445128725794, 4.537322665494407659 ) ) ;
#2739 = CARTESIAN_POINT ( 'NONE',  ( -31.57591258858714767, 52.94298397388165256, 1.523999999999994692 ) ) ;
#2740 = CARTESIAN_POINT ( 'NONE',  ( -4.923150864362091816, 117.4111644033810364, 0.9486898195072187567 ) ) ;
#2741 = CARTESIAN_POINT ( 'NONE',  ( -42.03620417734941839, 22.24401450883962639, 1.718184518069207245 ) ) ;
#2742 = EDGE_CURVE ( 'NONE', #41570, #5222, #32715, .T. ) ;
#2743 = CARTESIAN_POINT ( 'NONE',  ( -7.772068811996249771, 69.25462295839062676, -1.523999999999995580 ) ) ;
#2744 = CARTESIAN_POINT ( 'NONE',  ( -7.015191267815401588, 121.6841711688571905, 0.3965527081801285547 ) ) ;
#2745 = CARTESIAN_POINT ( 'NONE',  ( 3.287934792154566299, 21.71798121574904172, 3.254339964430349230 ) ) ;
#2746 = EDGE_CURVE ( 'NONE', #28854, #5531, #12951, .T. ) ;
#2747 = CARTESIAN_POINT ( 'NONE',  ( 14.55652921886106022, 120.9595740141730289, 1.205336527378881417 ) ) ;
#2748 = CARTESIAN_POINT ( 'NONE',  ( -0.09923067678108841994, 104.6144662015456248, -4.835257341052268565 ) ) ;
#2750 = CARTESIAN_POINT ( 'NONE',  ( 4.957730756931379545, 118.1424809852657773, -0.7901079947696816319 ) ) ;
#2749 = CARTESIAN_POINT ( 'NONE',  ( 2.664052010559913253, -13.52006206191685322, 0.08958796903007473778 ) ) ;
#2751 = CARTESIAN_POINT ( 'NONE',  ( -18.42722449710342048, 147.3262642721504960, 1.661950199828387875 ) ) ;
#2752 = CARTESIAN_POINT ( 'NONE',  ( -0.2501726036287156840, 25.39126883368370002, -4.616104092076634302 ) ) ;
#2753 = CARTESIAN_POINT ( 'NONE',  ( -19.50329963654034060, 128.7319734376252143, -1.320013405138365181 ) ) ;
#2754 = ORIENTED_EDGE ( 'NONE', *, *, #4976, .F. ) ;
#2755 = CARTESIAN_POINT ( 'NONE',  ( -56.38098843839168950, 3.837951075127326916, 1.838241461164903612 ) ) ;
#2756 = CARTESIAN_POINT ( 'NONE',  ( -9.094799215789770130, 123.6795089456687577, 0.2292421281602769478 ) ) ;
#2757 = EDGE_CURVE ( 'NONE', #3380, #22739, #11186, .T. ) ;
#2758 = CARTESIAN_POINT ( 'NONE',  ( 2.103176148521523459, -15.33886314497087611, 5.964097425510020756 ) ) ;
#2759 = CARTESIAN_POINT ( 'NONE',  ( 0.2925446776148338812, 115.7029491485453860, 1.764546176662535659 ) ) ;
#2760 = EDGE_CURVE ( 'NONE', #28898, #15081, #36787, .T. ) ;
#2761 = CARTESIAN_POINT ( 'NONE',  ( -4.585787403902434001, 118.0415163171067832, -0.8248535577628890447 ) ) ;
#2762 = CARTESIAN_POINT ( 'NONE',  ( 9.118174893680169646, 124.1671967267183589, 0.1822028344259499499 ) ) ;
#2763 = ORIENTED_EDGE ( 'NONE', *, *, #24028, .F. ) ;
#2764 = CARTESIAN_POINT ( 'NONE',  ( 3.201321489863619529, 118.6508749770327995, 0.9018090777949859804 ) ) ;
#2765 = FACE_OUTER_BOUND ( 'NONE', #13866, .T. ) ;
#2766 = DIRECTION ( 'NONE',  ( -0.8745520943968240202, 0.4849315768086553402, -6.829619984160650158E-16 ) ) ;
#2767 = ADVANCED_FACE ( 'NONE', ( #33780 ), #30564, .F. ) ;
#2768 = CARTESIAN_POINT ( 'NONE',  ( 5.007034960109912447, 117.4001718673160468, -0.7827158424842978190 ) ) ;
#2769 = CARTESIAN_POINT ( 'NONE',  ( 5.719359222665080011, 159.1232349745254453, -0.1048325176007952469 ) ) ;
#2770 = DIRECTION ( 'NONE',  ( 5.188838149069472160E-16, -1.699382548006136559E-16, -1.000000000000000000 ) ) ;
#2771 = CARTESIAN_POINT ( 'NONE',  ( -11.58677707360117282, 55.41127257906216386, 4.474811398756911807 ) ) ;
#2772 = CARTESIAN_POINT ( 'NONE',  ( 5.624629865489175096, 78.90958242041968163, 5.067363953418781541 ) ) ;
#2773 = CONICAL_SURFACE ( 'NONE', #27236, 2.540000000000002256, 0.7853981633974523868 ) ;
#2774 = CARTESIAN_POINT ( 'NONE',  ( 2.129294072315917052, -15.09917489183357198, 5.751238432448014137 ) ) ;
#2775 = CARTESIAN_POINT ( 'NONE',  ( -44.90991502375803890, 23.16658271142636139, 2.247441098035892981 ) ) ;
#2776 = CARTESIAN_POINT ( 'NONE',  ( 18.10310074716289819, 60.88085900918027704, 4.514343177587270439 ) ) ;
#2777 = CARTESIAN_POINT ( 'NONE',  ( -4.690708456685893424, 118.0052805208300413, 0.5844499725986116445 ) ) ;
#2778 = B_SPLINE_SURFACE_WITH_KNOTS ( 'NONE', 1, 3, ( 
 ( #13093, #12884, #26293, #38878, #19683, #32699, #32276, #32060, #22867, #3535, #19269, #9282, #19899, #38675 ),
 ( #16494, #35690, #3313, #29500, #26085, #19055, #39301, #28867, #12474, #340, #9481, #22445, #6499, #23080 ) ),
 .UNSPECIFIED., .F., .F., .F.,
 ( 2, 2 ),
 ( 4, 3, 2, 2, 3, 4 ),
 ( 0.000000000000000000, 1.000000000000000000 ),
 ( -0.01000000000000000021, 0.000000000000000000, 0.2500000000000000000, 0.5000000000000000000, 1.000000000000000000, 1.016448397156630046 ),
 .UNSPECIFIED. ) ;
#2779 = ORIENTED_EDGE ( 'NONE', *, *, #9655, .T. ) ;
#2780 = VERTEX_POINT ( 'NONE', #39543 ) ;
#2781 = CARTESIAN_POINT ( 'NONE',  ( -1.060522822118417086, 118.7629491485454167, -1.261313721580232805 ) ) ;
#2782 = CARTESIAN_POINT ( 'NONE',  ( -8.390773680403903256, 119.5504231609327093, -1.407582209411027296 ) ) ;
#2783 = CARTESIAN_POINT ( 'NONE',  ( -6.294717182677882938, 121.9812576474260055, -0.2818399057506478789 ) ) ;
#2784 = CARTESIAN_POINT ( 'NONE',  ( 4.656059677840232780, 118.0096173734262806, 0.7826279643646096851 ) ) ;
#2785 = CARTESIAN_POINT ( 'NONE',  ( -53.77660785250559883, 21.61116079084608188, -1.167830173942146849E-14 ) ) ;
#2786 = CARTESIAN_POINT ( 'NONE',  ( -12.05573777011654890, 128.3964238929853252, -1.202367467897995867 ) ) ;
#2787 = CARTESIAN_POINT ( 'NONE',  ( -4.187759052228169132, -5.978784877027076838, 2.003160513425938483 ) ) ;
#2788 = DIRECTION ( 'NONE',  ( -0.000000000000000000, 0.000000000000000000, -1.000000000000000000 ) ) ;
#2789 = CARTESIAN_POINT ( 'NONE',  ( -17.64290547347870941, 83.78857423953914463, -1.270000000000003126 ) ) ;
#2790 = CARTESIAN_POINT ( 'NONE',  ( 5.927223324825469319, 118.9825038774357466, -0.3493763292145122268 ) ) ;
#2791 = CARTESIAN_POINT ( 'NONE',  ( -10.71484998910098341, 123.2317624570580534, -1.496280440855931815 ) ) ;
#2792 = FILL_AREA_STYLE_COLOUR ( '', #1042 ) ;
#2793 = CARTESIAN_POINT ( 'NONE',  ( -2.714942736419990510, 34.21952868525605851, 3.834609254973532444 ) ) ;
#2794 = CARTESIAN_POINT ( 'NONE',  ( -6.985000000000036735, 56.51499999999998636, 0.000000000000000000 ) ) ;
#2795 = CARTESIAN_POINT ( 'NONE',  ( 4.627880361116947228, 7.839802885307131319, -0.3238752845059330032 ) ) ;
#2797 = ORIENTED_EDGE ( 'NONE', *, *, #37350, .T. ) ;
#2796 = CARTESIAN_POINT ( 'NONE',  ( 22.25501949494949372, 137.0232865695268458, 1.151097374996565614 ) ) ;
#2798 = CARTESIAN_POINT ( 'NONE',  ( 4.372714196296951350, 104.6144662015534834, -3.059664787259841923 ) ) ;
#2799 = CARTESIAN_POINT ( 'NONE',  ( 3.418015357486716699, -15.48303273933827917, 3.654867857709153345 ) ) ;
#2800 = CARTESIAN_POINT ( 'NONE',  ( -19.06420633224123407, 149.2349160008635351, 1.736338202726219526 ) ) ;
#2801 = CARTESIAN_POINT ( 'NONE',  ( 0.1071387893147941056, 24.31912984647217968, -0.9680276682219529638 ) ) ;
#2802 = CARTESIAN_POINT ( 'NONE',  ( 0.9699771559235883522, 8.716109271805494885, -0.1015519487743763993 ) ) ;
#2803 = ORIENTED_EDGE ( 'NONE', *, *, #2521, .F. ) ;
#2804 = EDGE_LOOP ( 'NONE', ( #15092, #6381, #25239, #7806 ) ) ;
#2805 = CARTESIAN_POINT ( 'NONE',  ( -4.469853575504566301, 31.48943071249222214, -0.6923489671027511783 ) ) ;
#2806 = CARTESIAN_POINT ( 'NONE',  ( 6.931894935422154624, 124.3275308867733600, 0.1497658092569641719 ) ) ;
#2807 = CARTESIAN_POINT ( 'NONE',  ( -15.79191249938960162, 148.1776054874778197, 0.7900072561285060857 ) ) ;
#2808 = DIRECTION ( 'NONE',  ( -0.5064479475276348897, 0.8622111466057285067, -0.01012003527073121814 ) ) ;
#2809 = CARTESIAN_POINT ( 'NONE',  ( 2.845270837621566518, -14.55731563485390723, 4.954299782322259205 ) ) ;
#2810 = CARTESIAN_POINT ( 'NONE',  ( 17.90094693680099169, 147.7668373613703352, -1.576197898085537563 ) ) ;
#2811 = CARTESIAN_POINT ( 'NONE',  ( -4.492596771379940179, 157.9011380394538833, -1.833279187945892730 ) ) ;
#2812 = CARTESIAN_POINT ( 'NONE',  ( -17.76856900107737403, 61.81127730225986738, -1.269999999999999352 ) ) ;
#2813 = CIRCLE ( 'NONE', #17073, 0.5080000000000000071 ) ;
#2814 = EDGE_CURVE ( 'NONE', #9109, #8970, #573, .T. ) ;
#2815 = CARTESIAN_POINT ( 'NONE',  ( 7.954247503138311970, 121.7101248947803356, 1.090747642478792745 ) ) ;
#2816 = CARTESIAN_POINT ( 'NONE',  ( 4.074910602682932925, 118.2429491485453354, -0.1454311599470142491 ) ) ;
#2817 = CARTESIAN_POINT ( 'NONE',  ( 15.57078937218316206, 147.5402044622178153, -0.01782986306386590697 ) ) ;
#2818 = ORIENTED_EDGE ( 'NONE', *, *, #28206, .T. ) ;
#2819 = AXIS2_PLACEMENT_3D ( 'NONE', #38175, #21956, #5807 ) ;
#2820 = CARTESIAN_POINT ( 'NONE',  ( -8.723850037987370243, 68.58388863026053173, 1.270000000000003126 ) ) ;
#2821 = CARTESIAN_POINT ( 'NONE',  ( -58.81784827865774190, -0.2724209480193806598, 0.09409996577156981568 ) ) ;
#2822 = CARTESIAN_POINT ( 'NONE',  ( -3.928768625441322104, 16.54256788600693895, -7.448509604454663702 ) ) ;
#2823 = CARTESIAN_POINT ( 'NONE',  ( 4.757797086070312709, 156.0326374431741385, 1.238355579604160095 ) ) ;
#2824 = CARTESIAN_POINT ( 'NONE',  ( 15.19943428492308080, 148.1072807477730748, 0.3037208696559882681 ) ) ;
#2825 = CARTESIAN_POINT ( 'NONE',  ( 16.86121613381884288, 155.2078297922403465, 0.3138802613840052658 ) ) ;
#2826 = CARTESIAN_POINT ( 'NONE',  ( -5.235361408262325433, 116.2637919873444190, 0.9632728985350241802 ) ) ;
#2827 = CARTESIAN_POINT ( 'NONE',  ( -5.177913976931298734, 78.94499979771843812, -5.372100000000003206 ) ) ;
#2828 = CARTESIAN_POINT ( 'NONE',  ( 3.758730197597703437, 121.0943292417197199, 0.07510837462871998438 ) ) ;
#2829 = CARTESIAN_POINT ( 'NONE',  ( 12.77966252534833203, 121.3369795956499928, 1.646308105693409685 ) ) ;
#2830 = CARTESIAN_POINT ( 'NONE',  ( 3.722543281321895936, 25.13347685689727484, 7.580879713197038683 ) ) ;
#2831 = CARTESIAN_POINT ( 'NONE',  ( 2.211048372675892715, 116.8625674272878712, -0.4564130614398590469 ) ) ;
#2832 = CARTESIAN_POINT ( 'NONE',  ( 0.01180776362021594868, 120.3637084677655764, -0.5909087754569243289 ) ) ;
#2833 = CARTESIAN_POINT ( 'NONE',  ( -11.73534362491071903, 82.73994711668952107, -1.269999999999999796 ) ) ;
#2834 = CARTESIAN_POINT ( 'NONE',  ( -10.39017547737320157, 56.51499999999998636, 6.098637220230963427E-16 ) ) ;
#2835 = CIRCLE ( 'NONE', #10996, 5.588000000000006295 ) ;
#2836 = CARTESIAN_POINT ( 'NONE',  ( 3.211436584971100849, 28.15539441671475274, -3.345526564039049688 ) ) ;
#2837 = CARTESIAN_POINT ( 'NONE',  ( -47.07934102874902749, 22.98505637820369429, -3.579966862081945145 ) ) ;
#2838 = DIRECTION ( 'NONE',  ( 1.000000000000000000, 0.000000000000000000, 0.000000000000000000 ) ) ;
#2839 = CARTESIAN_POINT ( 'NONE',  ( 3.198224922426783579, -14.19254063666773291, 2.189163805996276579 ) ) ;
#2840 = CARTESIAN_POINT ( 'NONE',  ( 1.052442600544414963, 124.5996987749017109, -0.008430925479885281390 ) ) ;
#2841 = CARTESIAN_POINT ( 'NONE',  ( -1.382728874883544234, 159.5452856091935132, 0.4834108180186511006 ) ) ;
#2842 = VERTEX_POINT ( 'NONE', #2243 ) ;
#2843 = CARTESIAN_POINT ( 'NONE',  ( -10.53334313995851801, 65.32054992887103140, 1.270000000000002904 ) ) ;
#2844 = ORIENTED_EDGE ( 'NONE', *, *, #17977, .F. ) ;
#2845 = CARTESIAN_POINT ( 'NONE',  ( -3.682264917456323339, 72.48346620154573827, -0.07358041635423968885 ) ) ;
#2846 = VECTOR ( 'NONE', #6322, 1000.000000000000000 ) ;
#2847 = CARTESIAN_POINT ( 'NONE',  ( 2.079639979227050350, -15.65372482070806548, 5.795360105834356013 ) ) ;
#2848 = CARTESIAN_POINT ( 'NONE',  ( -2.710741864450691097, 158.4754809254847601, 1.535472453293832640 ) ) ;
#2849 = CARTESIAN_POINT ( 'NONE',  ( 20.76678851138485271, 151.0745573368290593, -1.154740394482948185 ) ) ;
#2850 = CARTESIAN_POINT ( 'NONE',  ( -1.861891798414337940, 1.167894131763866250, -4.247245584637167504 ) ) ;
#2851 = CARTESIAN_POINT ( 'NONE',  ( -53.72989673830909396, 9.763294051742398949, -3.829717019284551771 ) ) ;
#2852 = ORIENTED_EDGE ( 'NONE', *, *, #6404, .T. ) ;
#2853 = CARTESIAN_POINT ( 'NONE',  ( -56.97096143714185246, 2.717004285893137805, -1.832255202883321443 ) ) ;
#2854 = CARTESIAN_POINT ( 'NONE',  ( 0.3606724330767769882, 121.2597428844643161, 0.4428036157107449466 ) ) ;
#2855 = DIRECTION ( 'NONE',  ( 0.000000000000000000, 1.000000000000000000, 0.000000000000000000 ) ) ;
#2856 = CARTESIAN_POINT ( 'NONE',  ( -16.92314199871296054, 144.1809451582817587, 1.383154804529856952 ) ) ;
#2857 = CARTESIAN_POINT ( 'NONE',  ( 17.14499999999999957, 71.11999999999999034, 5.016499999999999737 ) ) ;
#2858 = CARTESIAN_POINT ( 'NONE',  ( 5.904616261062731297, 156.9788419092994047, -1.696979819435221248 ) ) ;
#2859 = AXIS2_PLACEMENT_3D ( 'NONE', #24574, #40999, #27779 ) ;
#2860 = CARTESIAN_POINT ( 'NONE',  ( -16.44465323483264640, 153.5550899668227203, -2.240181424793372678 ) ) ;
#2861 = CARTESIAN_POINT ( 'NONE',  ( -55.60486134785667645, 7.243031971518515633, -3.140198620020504094 ) ) ;
#2862 = ORIENTED_EDGE ( 'NONE', *, *, #3971, .T. ) ;
#2863 = CARTESIAN_POINT ( 'NONE',  ( 14.80764902091315349, 139.2804412874323248, -0.6846718672572658093 ) ) ;
#2864 = ORIENTED_EDGE ( 'NONE', *, *, #3748, .F. ) ;
#2865 = CARTESIAN_POINT ( 'NONE',  ( -13.78152227852080181, 152.5163154464351294, -2.142015651154440370 ) ) ;
#2866 = CARTESIAN_POINT ( 'NONE',  ( 3.466386268343554899, -14.94433061298855492, 0.9111787176236659791 ) ) ;
#2867 = AXIS2_PLACEMENT_3D ( 'NONE', #22531, #29586, #12551 ) ;
#2868 = CARTESIAN_POINT ( 'NONE',  ( -4.065972646788793554, 118.2429491485453070, -0.3080848862740693250 ) ) ;
#2869 = CARTESIAN_POINT ( 'NONE',  ( 14.50851225146812240, 78.09971119798316863, -1.904999999999999583 ) ) ;
#2870 = CARTESIAN_POINT ( 'NONE',  ( -4.773199170040517636, 117.7614384816488240, 0.8821210834465519346 ) ) ;
#2871 = CARTESIAN_POINT ( 'NONE',  ( 17.42038752474475416, 148.2779598588913643, 2.227836471057101697 ) ) ;
#2872 = DIRECTION ( 'NONE',  ( 6.353134868986659519E-16, -1.000000000000000000, 0.000000000000000000 ) ) ;
#2873 = CARTESIAN_POINT ( 'NONE',  ( 0.9564925537785137211, 29.00497265395555857, -4.523030980006896407 ) ) ;
#2874 = CARTESIAN_POINT ( 'NONE',  ( 9.229262982541557747, 124.0999252189730697, 0.4162339757116151340 ) ) ;
#2875 = CARTESIAN_POINT ( 'NONE',  ( -50.82551848962686591, 16.13924203555649228, -4.804203053272171786 ) ) ;
#2877 = ORIENTED_EDGE ( 'NONE', *, *, #41566, .T. ) ;
#2876 = CARTESIAN_POINT ( 'NONE',  ( -47.14728576169839869, 19.79714445405676670, -4.666695388795785604 ) ) ;
#2878 = CARTESIAN_POINT ( 'NONE',  ( -17.32429653712378936, 61.56493206124108042, -1.269999999999999130 ) ) ;
#2879 = CARTESIAN_POINT ( 'NONE',  ( -46.68310778696854157, 26.02399849596702097, -1.327428962946700874 ) ) ;
#2880 = CARTESIAN_POINT ( 'NONE',  ( -49.69646605450807186, 16.77610880525235970, 4.988286919712930256 ) ) ;
#2881 = CARTESIAN_POINT ( 'NONE',  ( -8.682987951664228987, 118.1671358045530695, -0.9199987475528748071 ) ) ;
#2882 = CARTESIAN_POINT ( 'NONE',  ( -5.475330206976867231, 65.30181249999998272, -5.107412922131463695 ) ) ;
#2883 = CARTESIAN_POINT ( 'NONE',  ( -57.80205714066466527, 2.371715784325115095, 1.753227392946289154 ) ) ;
#2884 = CARTESIAN_POINT ( 'NONE',  ( -15.38960455597353416, 120.6961994932685798, -0.07768288530491206101 ) ) ;
#2885 = EDGE_LOOP ( 'NONE', ( #25918, #9135, #41042, #16 ) ) ;
#2886 = CARTESIAN_POINT ( 'NONE',  ( -50.36444701916330047, 17.30043933429478642, -4.508886934713599359 ) ) ;
#2887 = CARTESIAN_POINT ( 'NONE',  ( 7.812860049219216840, 122.5196119963270291, -0.1414684944325806104 ) ) ;
#2888 = EDGE_CURVE ( 'NONE', #8736, #12419, #14571, .T. ) ;
#2889 = CARTESIAN_POINT ( 'NONE',  ( -8.690931667554782081, 74.34623700195145091, -1.523999999999996913 ) ) ;
#2890 = ORIENTED_EDGE ( 'NONE', *, *, #22006, .F. ) ;
#2891 = CARTESIAN_POINT ( 'NONE',  ( 2.044657339584382783, 115.7029490950255592, -1.636397532061663496 ) ) ;
#2892 = CARTESIAN_POINT ( 'NONE',  ( 0.002459394112954048622, 156.3065584682211124, -0.1230781383047672012 ) ) ;
#2893 = CARTESIAN_POINT ( 'NONE',  ( 2.287996554222524903, -15.35138490607948469, 5.941601703801219436 ) ) ;
#2894 = CARTESIAN_POINT ( 'NONE',  ( -21.42146139051196130, 149.1985357531029308, 1.383244442692061371 ) ) ;
#2895 = DIRECTION ( 'NONE',  ( -9.627370216492862708E-17, -1.000000000000000000, 0.000000000000000000 ) ) ;
#2896 = AXIS2_PLACEMENT_3D ( 'NONE', #11932, #9169, #21293 ) ;
#2897 = CARTESIAN_POINT ( 'NONE',  ( 23.31615218609850615, 149.0517038676186417, 0.6965919665178230691 ) ) ;
#2898 = CARTESIAN_POINT ( 'NONE',  ( 7.041682102342773142, 122.0731594768587343, 0.2571765663980097871 ) ) ;
#2899 = CARTESIAN_POINT ( 'NONE',  ( 10.86251533436410277, 78.45482716897161879, 1.904999999999999583 ) ) ;
#2900 = CARTESIAN_POINT ( 'NONE',  ( -0.5883093083485460006, 14.76436220226899465, 0.7776626239079347247 ) ) ;
#2901 = CARTESIAN_POINT ( 'NONE',  ( -3.735388766125086857, 116.6566025657135413, -0.1875874814615930974 ) ) ;
#2902 = DIRECTION ( 'NONE',  ( 3.035386659626960118E-16, -0.000000000000000000, 1.000000000000000000 ) ) ;
#2903 = ORIENTED_EDGE ( 'NONE', *, *, #39425, .T. ) ;
#2904 = CARTESIAN_POINT ( 'NONE',  ( 2.508634252739555759, 116.7753849408351243, 0.5210829680955889609 ) ) ;
#2905 = EDGE_LOOP ( 'NONE', ( #38246, #11736, #28782, #1830 ) ) ;
#2906 = DIRECTION ( 'NONE',  ( 0.7548010569845150508, 0.6559537821943391966, 0.000000000000000000 ) ) ;
#2907 = CARTESIAN_POINT ( 'NONE',  ( -0.009931510163752330436, 117.7854482299006378, 0.4970133802592049954 ) ) ;
#2908 = CARTESIAN_POINT ( 'NONE',  ( 11.07050914993712709, 156.0189320485970086, -1.715486126203028316 ) ) ;
#2909 = CARTESIAN_POINT ( 'NONE',  ( 5.057590804293729647, 14.82039226405042243, -6.742867120243351664 ) ) ;
#2910 = CARTESIAN_POINT ( 'NONE',  ( -20.86915823776865153, 136.4823663107028722, -1.950121757083878027 ) ) ;
#2911 = CARTESIAN_POINT ( 'NONE',  ( 4.732332605385225044, 117.8971787801968674, -0.7794400467109126041 ) ) ;
#2912 = EDGE_CURVE ( 'NONE', #2187, #21980, #1816, .T. ) ;
#2913 = CARTESIAN_POINT ( 'NONE',  ( -17.14500000000466784, 71.11999999999886768, 1.523999999999998689 ) ) ;
#2914 = AXIS2_PLACEMENT_3D ( 'NONE', #14992, #15203, #41001 ) ;
#2915 = CARTESIAN_POINT ( 'NONE',  ( -9.188648150231783163, 124.1858035287836231, -0.09819667026458960002 ) ) ;
#2916 = CARTESIAN_POINT ( 'NONE',  ( -15.10275521329014126, 128.5586215118215705, -2.151272397954998805 ) ) ;
#2917 = CARTESIAN_POINT ( 'NONE',  ( 2.745816630209086728, -15.73397280162352985, 5.435574744647863277 ) ) ;
#2918 = CARTESIAN_POINT ( 'NONE',  ( -10.92199999999999704, 12.96416000000000146, 0.000000000000000000 ) ) ;
#2919 = CARTESIAN_POINT ( 'NONE',  ( -43.49527490626578441, 22.26612824116996237, -2.150709692269579865 ) ) ;
#2920 = ORIENTED_EDGE ( 'NONE', *, *, #2488, .F. ) ;
#2921 = CARTESIAN_POINT ( 'NONE',  ( 8.426631749355106393, 120.7201681212196291, 1.435507493075423913 ) ) ;
#2922 = CARTESIAN_POINT ( 'NONE',  ( 9.132817075745611705E-16, 9.026346327358515609, 0.000000000000000000 ) ) ;
#2923 = CARTESIAN_POINT ( 'NONE',  ( -28.36525985791271154, 77.02308833105713859, -1.524000000000007571 ) ) ;
#2924 = TOROIDAL_SURFACE ( 'NONE', #32831, 0.3810000000000001719, 0.2540000000000000036 ) ;
#2925 = CARTESIAN_POINT ( 'NONE',  ( -3.788670433418693140, 121.1194860566822626, 0.2213384591549591440 ) ) ;
#2926 = CARTESIAN_POINT ( 'NONE',  ( 8.184481992144968743, -14.99546276350015717, -2.142971516962156819 ) ) ;
#2927 = CARTESIAN_POINT ( 'NONE',  ( 9.518183030555334767, 123.9284174147966269, 0.7933090623874852199 ) ) ;
#2928 = CARTESIAN_POINT ( 'NONE',  ( 0.006370369177266787912, 117.0014201992989058, -0.3187993231787207837 ) ) ;
#2929 = DIRECTION ( 'NONE',  ( -0.4849315768086535638, -0.8745520943968251304, -1.030032898892975065E-16 ) ) ;
#2930 = DIRECTION ( 'NONE',  ( 1.011795553208986377E-16, 1.000000000000000000, -0.000000000000000000 ) ) ;
#2931 = AXIS2_PLACEMENT_3D ( 'NONE', #32096, #2929, #10142 ) ;
#2932 = EDGE_CURVE ( 'NONE', #31858, #41583, #14310, .T. ) ;
#2933 = CARTESIAN_POINT ( 'NONE',  ( -23.34374616560295834, 149.0672090665632936, -0.4407082534803007379 ) ) ;
#2934 = ORIENTED_EDGE ( 'NONE', *, *, #1749, .T. ) ;
#2935 = CARTESIAN_POINT ( 'NONE',  ( -6.287620022660915353, 119.9368201151051494, -1.217206256648388996 ) ) ;
#2936 = DIRECTION ( 'NONE',  ( -0.9998004120163608288, 0.000000000000000000, -0.01997839162482749342 ) ) ;
#2937 = CARTESIAN_POINT ( 'NONE',  ( -2.749413646642218101, 120.8469057251343060, -0.2833394764088548734 ) ) ;
#2938 = CARTESIAN_POINT ( 'NONE',  ( -41.25198945386251381, 23.25239630053170714, 1.523999999999992916 ) ) ;
#2939 = CARTESIAN_POINT ( 'NONE',  ( 1.421603664355671315, 159.6054662015457666, 0.02840702444251847966 ) ) ;
#2940 = VERTEX_POINT ( 'NONE', #15201 ) ;
#2941 = CARTESIAN_POINT ( 'NONE',  ( 4.076717266748975277, 8.489475128091552136, -2.202413229635628689 ) ) ;
#2942 = CARTESIAN_POINT ( 'NONE',  ( -28.95189557067410746, 64.41341631820462510, 1.523999999999993360 ) ) ;
#2943 = CARTESIAN_POINT ( 'NONE',  ( -4.977065986284164190, 117.4065423621357382, 0.8841140845778143742 ) ) ;
#2944 = DIRECTION ( 'NONE',  ( -5.188838149069471174E-16, 1.699382548006136313E-16, 1.000000000000000000 ) ) ;
#2945 = CARTESIAN_POINT ( 'NONE',  ( 3.174366308151881810, 71.97546620154574271, 0.06343139340882768262 ) ) ;
#2946 = CARTESIAN_POINT ( 'NONE',  ( 5.993962039581884227, 120.5133896973282361, 0.9940668381815480625 ) ) ;
#2947 = CARTESIAN_POINT ( 'NONE',  ( -3.469956624915944587, 9.623539240006554252, 3.074419811715999984 ) ) ;
#2948 = CARTESIAN_POINT ( 'NONE',  ( 22.54389841724620425, 148.7221180073953235, 1.757920738659724869 ) ) ;
#2949 = CARTESIAN_POINT ( 'NONE',  ( -52.95179419874195048, 11.24610246600658137, -4.133922171301945170 ) ) ;
#2951 = CARTESIAN_POINT ( 'NONE',  ( 0.4229338353207374723, 117.8786474493541050, -0.5307671053780917969 ) ) ;
#2950 = CARTESIAN_POINT ( 'NONE',  ( 0.9116540650998883333, 106.1659180060823644, 5.214520442167681402 ) ) ;
#2952 = AXIS2_PLACEMENT_3D ( 'NONE', #5972, #19351, #38343 ) ;
#2953 = CARTESIAN_POINT ( 'NONE',  ( 2.551181839206869917, 14.82117702134586779, -3.857898856385788999 ) ) ;
#2954 = CARTESIAN_POINT ( 'NONE',  ( -21.51154278844960999, 151.3526640061693342, -1.384567357891492989 ) ) ;
#2955 = AXIS2_PLACEMENT_3D ( 'NONE', #13412, #41977, #3849 ) ;
#2956 = EDGE_LOOP ( 'NONE', ( #36714, #1765, #34518, #33198 ) ) ;
#2957 = CARTESIAN_POINT ( 'NONE',  ( -1.653377498379716481, 156.2910218135955631, 0.4236837486942557351 ) ) ;
#2958 = CARTESIAN_POINT ( 'NONE',  ( 3.016199308703121140, -15.16462411293013979, 5.702656747445028707 ) ) ;
#2959 = DIRECTION ( 'NONE',  ( 0.9998004120163609398, 4.016384292689130894E-17, 0.01997839162482749689 ) ) ;
#2960 = VECTOR ( 'NONE', #14167, 1000.000000000000000 ) ;
#2961 = CARTESIAN_POINT ( 'NONE',  ( -4.641563771631805224, 117.9844563754833899, -0.8830158030444785755 ) ) ;
#2962 = EDGE_CURVE ( 'NONE', #30889, #12049, #40264, .T. ) ;
#2963 = CARTESIAN_POINT ( 'NONE',  ( 3.758730197597703437, 121.0943292417197199, 0.07510837462872009540 ) ) ;
#2964 = ORIENTED_EDGE ( 'NONE', *, *, #11343, .T. ) ;
#2965 = CARTESIAN_POINT ( 'NONE',  ( 19.41896158923237081, 149.6234262069624492, 2.479904253118717428 ) ) ;
#2966 = CARTESIAN_POINT ( 'NONE',  ( 18.35410564743290962, 77.35382415001784295, 1.904999999999988258 ) ) ;
#2967 = CARTESIAN_POINT ( 'NONE',  ( 8.981069108608807028, 123.9698733229553937, 0.1794631345465902139 ) ) ;
#2968 = CARTESIAN_POINT ( 'NONE',  ( -8.125192968412418892, 117.9016134627522945, 0.4934282302770854334 ) ) ;
#2969 = CARTESIAN_POINT ( 'NONE',  ( 4.889703507614793665, 117.4101837603834468, -0.9754936775373431734 ) ) ;
#2970 = CARTESIAN_POINT ( 'NONE',  ( 5.835061174465369760, 117.1115750087645608, -0.2489150398414469723 ) ) ;
#2971 = EDGE_CURVE ( 'NONE', #11359, #20793, #32764, .T. ) ;
#2972 = CARTESIAN_POINT ( 'NONE',  ( -5.449227423685445437, 56.51500000000039847, -5.145694933558188744 ) ) ;
#2973 = CIRCLE ( 'NONE', #4357, 5.080000000000006288 ) ;
#2974 = CARTESIAN_POINT ( 'NONE',  ( -52.53679969070437750, 11.65360597696575873, 4.035185998988639611 ) ) ;
#2975 = CARTESIAN_POINT ( 'NONE',  ( 5.654802103384407808, 78.90710107780496685, 5.057831774704117045 ) ) ;
#2976 = CARTESIAN_POINT ( 'NONE',  ( -4.937650010152420776, 117.4076175032476499, -1.082176492592219041 ) ) ;
#2977 = CARTESIAN_POINT ( 'NONE',  ( -47.00787117332040310, 24.49876931072293829, 2.333946431867817584 ) ) ;
#2978 = CARTESIAN_POINT ( 'NONE',  ( -58.82785807807199063, -0.2608716074412517072, 0.04555283349572796653 ) ) ;
#2979 = CIRCLE ( 'NONE', #36979, 3.683000000000001162 ) ;
#2980 = CARTESIAN_POINT ( 'NONE',  ( -4.687306205058505704, 118.0075146718663461, 0.5901339194766732632 ) ) ;
#2981 = ORIENTED_EDGE ( 'NONE', *, *, #20181, .F. ) ;
#2982 = ORIENTED_EDGE ( 'NONE', *, *, #14629, .T. ) ;
#2983 = CARTESIAN_POINT ( 'NONE',  ( -24.32950799593924884, 77.42192949967211746, -1.524000000000005572 ) ) ;
#2984 = ADVANCED_FACE ( 'NONE', ( #28204 ), #15672, .T. ) ;
#2985 = CARTESIAN_POINT ( 'NONE',  ( -3.396746297042179563, 118.5725545226142401, -0.9267210084873370723 ) ) ;
#2986 = CARTESIAN_POINT ( 'NONE',  ( -5.908534618824000439, 118.9825038774357466, -0.5858829404670614638 ) ) ;
#2987 = CARTESIAN_POINT ( 'NONE',  ( 4.734060133346893906, 117.8958279061648255, 0.9307166829614513803 ) ) ;
#2988 = CARTESIAN_POINT ( 'NONE',  ( 3.221735024265227398, -14.36526069886394730, 2.718910799868354378 ) ) ;
#2989 = CARTESIAN_POINT ( 'NONE',  ( -16.46997841215784675, 146.2355833862463328, -1.608729380348347560 ) ) ;
#2990 = AXIS2_PLACEMENT_3D ( 'NONE', #3329, #12692, #29300 ) ;
#2991 = CARTESIAN_POINT ( 'NONE',  ( -3.489676481241766659, 115.7029491485453434, -1.632600653323997175 ) ) ;
#2992 = EDGE_CURVE ( 'NONE', #24363, #30281, #34138, .T. ) ;
#2993 = CARTESIAN_POINT ( 'NONE',  ( -4.660682439260153131, 113.7930424115631070, 2.024998540755147403 ) ) ;
#2994 = CARTESIAN_POINT ( 'NONE',  ( -4.345705637489785111, 70.43763872253877878, -1.269999999999994023 ) ) ;
#2995 = CARTESIAN_POINT ( 'NONE',  ( 7.093755517943316491, 122.4291926079955317, 0.03209900709771758981 ) ) ;
#2996 = CARTESIAN_POINT ( 'NONE',  ( 0.02615319344467511437, 156.8698190429800832, -1.308812744920978322 ) ) ;
#2997 = CARTESIAN_POINT ( 'NONE',  ( -9.665786669610962889, 55.24499999999999034, 0.1866227975165204167 ) ) ;
#2998 = CARTESIAN_POINT ( 'NONE',  ( -6.446885413170102552, 29.42808026494702389, 0.2842954123359194840 ) ) ;
#2999 = CARTESIAN_POINT ( 'NONE',  ( -3.151729977245023573, 115.7029491485453860, 1.538670711546385572 ) ) ;
#3000 = CARTESIAN_POINT ( 'NONE',  ( 4.224370802630715183, -2.505441902618962935, 1.893578447770203566 ) ) ;
#3002 = ORIENTED_EDGE ( 'NONE', *, *, #23149, .F. ) ;
#3001 = CARTESIAN_POINT ( 'NONE',  ( 5.618954885708931535, 159.1014311945586712, 0.6070295849213357409 ) ) ;
#3003 = DIRECTION ( 'NONE',  ( -1.000000000000000000, 1.288607544181256696E-16, 0.000000000000000000 ) ) ;
#3004 = CIRCLE ( 'NONE', #21326, 8.794749999999993406 ) ;
#3005 = CARTESIAN_POINT ( 'NONE',  ( 3.466386268343554899, -14.94433061298855492, 0.9111787176236659791 ) ) ;
#3006 = CARTESIAN_POINT ( 'NONE',  ( -8.713776656587379321, 120.2102557752085232, 1.142027078586575595 ) ) ;
#3007 = CARTESIAN_POINT ( 'NONE',  ( 0.8997923272943838535, 13.09534505249760805, -0.3740510727227569499 ) ) ;
#3008 = CARTESIAN_POINT ( 'NONE',  ( -0.006055453635351584415, 1.369653838947524349, -0.9756124606672940125 ) ) ;
#3009 = VERTEX_POINT ( 'NONE', #5921 ) ;
#3010 = EDGE_LOOP ( 'NONE', ( #40516, #27985, #744, #41049, #27638, #34437, #8513, #1972, #1418, #39890 ) ) ;
#3011 = CARTESIAN_POINT ( 'NONE',  ( -41.31025181302593552, 22.81788724727718076, 1.523999999999983146 ) ) ;
#3012 = EDGE_CURVE ( 'NONE', #34369, #4125, #30049, .T. ) ;
#3013 = CARTESIAN_POINT ( 'NONE',  ( 3.014030426305779553, 115.9530684888725460, 1.587286815012126207 ) ) ;
#3014 =( NAMED_UNIT ( * ) PLANE_ANGLE_UNIT ( ) SI_UNIT ( $, .RADIAN. ) );
#3015 = CARTESIAN_POINT ( 'NONE',  ( -0.006077178772743973764, 120.4695998130595598, 0.3041268764237435862 ) ) ;
#3016 = DIRECTION ( 'NONE',  ( -0.1906721105965087926, 0.9816537812491085147, 0.000000000000000000 ) ) ;
#3017 = CARTESIAN_POINT ( 'NONE',  ( 2.668130780779813360, -14.68804970414791455, 5.313657848291281738 ) ) ;
#3018 = CARTESIAN_POINT ( 'NONE',  ( 8.280704432558463779, 121.1361926620737393, -1.000371422393417475 ) ) ;
#3019 = AXIS2_PLACEMENT_3D ( 'NONE', #16498, #25672, #28871 ) ;
#3020 = CARTESIAN_POINT ( 'NONE',  ( -14.77311812546558123, 125.6006210965460781, -2.040279103193882282 ) ) ;
#3021 = FACE_OUTER_BOUND ( 'NONE', #32541, .T. ) ;
#3022 = CARTESIAN_POINT ( 'NONE',  ( 8.564519932783092315, 118.7250576737585845, 1.182609549202882082 ) ) ;
#3023 = CARTESIAN_POINT ( 'NONE',  ( -5.530486672362699530, 32.07197567765449975, 2.641630925256825080 ) ) ;
#3024 = CARTESIAN_POINT ( 'NONE',  ( 6.058098509843102164, 155.3491655920357459, -0.2313079102920780339 ) ) ;
#3025 = ORIENTED_EDGE ( 'NONE', *, *, #12507, .F. ) ;
#3026 = DIRECTION ( 'NONE',  ( 5.206863593109713661E-17, -1.000000000000000000, 1.077750396879097183E-30 ) ) ;
#3027 = CARTESIAN_POINT ( 'NONE',  ( -6.615214180512292604E-14, 94.32746620154571815, -2.829521569843129660E-18 ) ) ;
#3028 = AXIS2_PLACEMENT_3D ( 'NONE', #42158, #3174, #32994 ) ;
#3029 = EDGE_CURVE ( 'NONE', #14963, #32351, #15483, .T. ) ;
#3030 = DIRECTION ( 'NONE',  ( -1.000000000000000000, 0.000000000000000000, 0.000000000000000000 ) ) ;
#3031 = CARTESIAN_POINT ( 'NONE',  ( 9.757351933493456642, 123.8372022493589100, 0.9812814142356128810 ) ) ;
#3032 = LINE ( 'NONE', #15987, #30102 ) ;
#3033 = CARTESIAN_POINT ( 'NONE',  ( 1.806356699219098250, 116.4728921782852922, -0.003255218499346594716 ) ) ;
#3034 = CARTESIAN_POINT ( 'NONE',  ( -4.488494058616981697, 111.2667756541687538, 2.954587190001159325 ) ) ;
#3035 = CARTESIAN_POINT ( 'NONE',  ( -4.375468101073169969, 118.7629491485454309, 0.8819984256705631909 ) ) ;
#3036 = CARTESIAN_POINT ( 'NONE',  ( -11.58677707360137532, 17.14499999999999957, 4.474811398758258285 ) ) ;
#3037 = CARTESIAN_POINT ( 'NONE',  ( -0.5257358919991518276, 34.34849739310375583, 0.2665863176793757394 ) ) ;
#3038 = CARTESIAN_POINT ( 'NONE',  ( 20.83122434882616858, 148.6614476615901594, 2.397187407820276395 ) ) ;
#3039 = CARTESIAN_POINT ( 'NONE',  ( -3.632229383214316876, 17.08265688572556584, -2.901706292871565562 ) ) ;
#3040 = CARTESIAN_POINT ( 'NONE',  ( 7.100331465950064036, 27.70181474634058461, -4.559502152892632942 ) ) ;
#3041 = CARTESIAN_POINT ( 'NONE',  ( 2.181699532838504929, 116.7361444524075864, -0.4061292330571752984 ) ) ;
#3042 = CARTESIAN_POINT ( 'NONE',  ( -0.2537530607705146823, 113.0327356262573915, -2.627782494400415558 ) ) ;
#3043 = CARTESIAN_POINT ( 'NONE',  ( -23.34387769576312621, 77.71194901948682343, 1.269999999999993134 ) ) ;
#3044 = CARTESIAN_POINT ( 'NONE',  ( 2.874628747758903646, 107.8418180396803336, -4.365346587048165361 ) ) ;
#3045 = CARTESIAN_POINT ( 'NONE',  ( 2.609247996698298877, 104.6144662015478843, 4.655519476068421980 ) ) ;
#3046 = CARTESIAN_POINT ( 'NONE',  ( 3.874746376330849618, 18.20996518813934628, -2.522041008920607563 ) ) ;
#3047 = EDGE_CURVE ( 'NONE', #16319, #16174, #16899, .T. ) ;
#3048 = DIRECTION ( 'NONE',  ( -0.9454731675810336133, 0.3256999990547843615, -5.459396135145337199E-16 ) ) ;
#3049 = CARTESIAN_POINT ( 'NONE',  ( 3.131015516031846690, -14.62848841321586946, 3.524024012273756501 ) ) ;
#3050 = CARTESIAN_POINT ( 'NONE',  ( 2.504607545376390298, 120.2382744777187611, -0.4047138806074997985 ) ) ;
#3051 = CARTESIAN_POINT ( 'NONE',  ( -14.93494801707998576, 120.8072429308574414, 0.3831319127562622384 ) ) ;
#3052 = ORIENTED_EDGE ( 'NONE', *, *, #1205, .T. ) ;
#3053 = DIRECTION ( 'NONE',  ( -0.6594218222380214822, -0.7517731442105972661, -2.144082946226365319E-16 ) ) ;
#3054 =( BOUNDED_CURVE ( )  B_SPLINE_CURVE ( 3, ( #28704, #41713, #12519, #28909 ),
 .UNSPECIFIED., .F., .T. ) 
 B_SPLINE_CURVE_WITH_KNOTS ( ( 4, 4 ),
 ( 4.712388980384686121, 5.673871460451326065 ),
 .UNSPECIFIED. ) 
 CURVE ( )  GEOMETRIC_REPRESENTATION_ITEM ( )  RATIONAL_B_SPLINE_CURVE ( ( 1.000000000000000000, 0.9244349266169030743, 0.9244349266169030743, 1.000000000000000000 ) ) 
 REPRESENTATION_ITEM ( '' )  );
#3055 = EDGE_LOOP ( 'NONE', ( #23597, #21939, #2058, #29396 ) ) ;
#3056 = CARTESIAN_POINT ( 'NONE',  ( -43.04734275525184728, 21.71211564561841101, -2.244749861974538074 ) ) ;
#3057 = CARTESIAN_POINT ( 'NONE',  ( 5.007622726684139991, -15.39085649315211057, 3.402342850907996041 ) ) ;
#3058 = CARTESIAN_POINT ( 'NONE',  ( -13.10063739191627086, 155.4510764517707742, 1.634185922311342631 ) ) ;
#3059 = CARTESIAN_POINT ( 'NONE',  ( 17.11036550247942145, 125.2153959547233910, -0.9255656842583630528 ) ) ;
#3060 = CARTESIAN_POINT ( 'NONE',  ( 2.229080734463354307, 9.364070591990056869, -4.050418370856919914 ) ) ;
#3061 = CARTESIAN_POINT ( 'NONE',  ( -56.38145225766449187, 4.490824468634439626, -2.575949247650338503 ) ) ;
#3062 = ORIENTED_EDGE ( 'NONE', *, *, #26982, .T. ) ;
#3063 = CARTESIAN_POINT ( 'NONE',  ( -48.97544177847666447, 17.83334834807594049, -5.075951225172628867 ) ) ;
#3064 = CARTESIAN_POINT ( 'NONE',  ( -0.01111760956581894950, 120.5507043431653784, 0.5563706444132522355 ) ) ;
#3065 =( NAMED_UNIT ( * ) PLANE_ANGLE_UNIT ( ) SI_UNIT ( $, .RADIAN. ) );
#3066 = CARTESIAN_POINT ( 'NONE',  ( -16.40043613793208621, 149.3997711511537148, 1.468335723160356654 ) ) ;
#3067 = CARTESIAN_POINT ( 'NONE',  ( -17.14500000000466784, 71.11999999999886768, 1.523999999999998689 ) ) ;
#3068 = CARTESIAN_POINT ( 'NONE',  ( 10.22873863908706404, 155.5514087735115822, -1.732306429912916723 ) ) ;
#3069 = CARTESIAN_POINT ( 'NONE',  ( -2.740693480742399490, 158.6924860557018064, -1.553331106148862384 ) ) ;
#3070 = CARTESIAN_POINT ( 'NONE',  ( -57.57967628038989005, 1.451576601202181349, -1.494865757154152153 ) ) ;
#3071 = ORIENTED_EDGE ( 'NONE', *, *, #31245, .T. ) ;
#3072 = CARTESIAN_POINT ( 'NONE',  ( 4.599907942160887053, 118.0774652753429450, -0.5280204677610548236 ) ) ;
#3073 = CARTESIAN_POINT ( 'NONE',  ( 11.75634259954068739, 128.3321206738457647, -0.5010001888332089592 ) ) ;
#3074 = ORIENTED_EDGE ( 'NONE', *, *, #3776, .T. ) ;
#3075 = CARTESIAN_POINT ( 'NONE',  ( -15.43964774321195144, 150.7699688800196611, -2.159935508548367356 ) ) ;
#3076 = CARTESIAN_POINT ( 'NONE',  ( 3.246941722412215459, -15.25025356868572857, 3.602141857564104210 ) ) ;
#3077 = DIRECTION ( 'NONE',  ( 0.9998004120163609398, 0.000000000000000000, 0.01997839162482749689 ) ) ;
#3078 = CARTESIAN_POINT ( 'NONE',  ( -4.801647862234980302, 117.4032733357427105, 1.015449305853463491 ) ) ;
#3079 = CARTESIAN_POINT ( 'NONE',  ( -4.797757306094807994, 117.7649951200880025, 0.8642570761844743377 ) ) ;
#3080 = CARTESIAN_POINT ( 'NONE',  ( 1.975234429548441195, 156.8313070664539168, 1.415192030232629072 ) ) ;
#3081 = CARTESIAN_POINT ( 'NONE',  ( 0.1949087904810299920, 33.82644263972942156, 0.4054292462034601585 ) ) ;
#3082 = CARTESIAN_POINT ( 'NONE',  ( 8.369577038434204752, -11.69170392490758381, 0.7719616968112763544 ) ) ;
#3083 = CARTESIAN_POINT ( 'NONE',  ( 15.29340151118736735, 148.0176312819745874, 0.6334265850898870287 ) ) ;
#3084 = DIRECTION ( 'NONE',  ( -0.3582377630123906309, 0.9336303900108855469, 0.000000000000000000 ) ) ;
#3086 = EDGE_LOOP ( 'NONE', ( #8479, #22620, #4696, #3580 ) ) ;
#3085 = CARTESIAN_POINT ( 'NONE',  ( -49.14072577824710208, 13.89916973120787524, -0.4067138869237436061 ) ) ;
#3087 = CARTESIAN_POINT ( 'NONE',  ( -0.4175747659228876696, 118.1588898423965048, 0.8928943804540209195 ) ) ;
#3088 = CARTESIAN_POINT ( 'NONE',  ( -47.66286930719412851, 20.62480072838431155, 5.054501799269492501 ) ) ;
#3089 = CARTESIAN_POINT ( 'NONE',  ( -53.96359711957523331, 9.317927474182681635, 3.738358014028002607 ) ) ;
#3090 = LINE ( 'NONE', #19457, #7963 ) ;
#3091 = CARTESIAN_POINT ( 'NONE',  ( 2.081416901521091933, -15.50639809317535089, 5.943648939154567934 ) ) ;
#3092 = DIRECTION ( 'NONE',  ( 5.188838149069472160E-16, -1.699382548006136559E-16, -1.000000000000000000 ) ) ;
#3093 = CARTESIAN_POINT ( 'NONE',  ( -55.38777061991515183, 7.924152594517688719, 2.969223861581042012 ) ) ;
#3094 = CARTESIAN_POINT ( 'NONE',  ( -3.754954749907463807, 116.6824454826851820, 0.08209545411912770596 ) ) ;
#3095 = EDGE_LOOP ( 'NONE', ( #4542, #38939, #15926, #25195 ) ) ;
#3096 = CARTESIAN_POINT ( 'NONE',  ( -54.80060171144386771, 10.20856468236482684, -2.175828276708582365 ) ) ;
#3097 = CARTESIAN_POINT ( 'NONE',  ( -7.817668890232951640, 122.4248663112730782, -0.5901703440876553408 ) ) ;
#3098 = ORIENTED_EDGE ( 'NONE', *, *, #15474, .T. ) ;
#3099 = CARTESIAN_POINT ( 'NONE',  ( 2.338193611591690146, 115.7028059236074142, -1.613667146768946958 ) ) ;
#3100 = CARTESIAN_POINT ( 'NONE',  ( -1.603837441938277930, 120.9755568995931156, -0.09629321774905863496 ) ) ;
#3101 = CARTESIAN_POINT ( 'NONE',  ( 5.673832624563095450, -13.47712647082498272, 2.605829897212420754 ) ) ;
#3102 = CARTESIAN_POINT ( 'NONE',  ( -0.009513433763575551705, 117.6614778598761291, 0.4760911276077181564 ) ) ;
#3103 = CARTESIAN_POINT ( 'NONE',  ( -17.14500000000466784, 71.11999999999886768, 1.269999999999998241 ) ) ;
#3104 = CARTESIAN_POINT ( 'NONE',  ( 22.79149376799268722, 150.3987591554885626, 0.7843734907460314654 ) ) ;
#3105 = CARTESIAN_POINT ( 'NONE',  ( 15.78018659616589581, 146.2345701426180824, 0.4496550483759581551 ) ) ;
#3106 = DIRECTION ( 'NONE',  ( 5.188838149069472160E-16, -1.699382548006136559E-16, -1.000000000000000000 ) ) ;
#3107 = CARTESIAN_POINT ( 'NONE',  ( -0.2244654480080381653, 11.31155722793083918, -0.9512810396025579429 ) ) ;
#3108 = CARTESIAN_POINT ( 'NONE',  ( -16.10347893962658361, 121.2391669109744186, -0.4275719782727095408 ) ) ;
#3109 = DIRECTION ( 'NONE',  ( 0.01731298258488772612, -0.9998501190848633202, 1.788962107505314604E-16 ) ) ;
#3110 = CARTESIAN_POINT ( 'NONE',  ( -10.92199999999999704, 55.24499999999999034, -7.690731210240437325E-16 ) ) ;
#3111 = CIRCLE ( 'NONE', #24828, 0.2540000000000052771 ) ;
#3112 = CARTESIAN_POINT ( 'NONE',  ( 5.533182690628008160, 117.2225855060814013, 0.7735903190986758160 ) ) ;
#3113 = ORIENTED_EDGE ( 'NONE', *, *, #18091, .F. ) ;
#3114 = CARTESIAN_POINT ( 'NONE',  ( -58.36160036302118215, -0.2744091231881636284, -0.1136734763339792287 ) ) ;
#3115 = CARTESIAN_POINT ( 'NONE',  ( 21.10167996235824717, 141.7209635633906259, 2.240609589767335486 ) ) ;
#3116 = CARTESIAN_POINT ( 'NONE',  ( 6.464497043865751635, 157.5392376370035095, -1.685792624679405494 ) ) ;
#3117 = CARTESIAN_POINT ( 'NONE',  ( -8.002357889267953439, 8.121853428443936096, -2.619265908643666929 ) ) ;
#3118 = CARTESIAN_POINT ( 'NONE',  ( -13.94627971010885403, 121.2764344996515717, -1.482775695869144483 ) ) ;
#3119 = CARTESIAN_POINT ( 'NONE',  ( 4.735283304133474758, 117.8439692571760986, -0.8354117580122082387 ) ) ;
#3120 = CARTESIAN_POINT ( 'NONE',  ( 0.6715300310779280801, 105.9424719104300436, 5.313162126831953103 ) ) ;
#3121 = CARTESIAN_POINT ( 'NONE',  ( -1.612929917264666502, 120.9971453638330985, -0.006532979378300230941 ) ) ;
#3122 = CARTESIAN_POINT ( 'NONE',  ( -14.67610382776227418, 152.8628051715174365, -2.323547792494559339 ) ) ;
#3123 = CARTESIAN_POINT ( 'NONE',  ( 3.255875469058810978, -15.74984210207193414, 5.086368125509904026 ) ) ;
#3124 = CARTESIAN_POINT ( 'NONE',  ( -13.99440778436217414, 79.95103047660883533, -1.270000000000000462 ) ) ;
#3125 = CARTESIAN_POINT ( 'NONE',  ( -45.76673701974917208, 25.51931200435043934, -1.524000000000008237 ) ) ;
#3126 = ORIENTED_EDGE ( 'NONE', *, *, #14081, .F. ) ;
#3127 = B_SPLINE_SURFACE_WITH_KNOTS ( 'NONE', 1, 3, ( 
 ( #10981, #39979, #23751, #36982, #4413, #7380, #29950, #36772, #20764, #13764, #36366, #4616, #17777, #17572, #14371, #27381, #10565, #33995 ),
 ( #40391, #30774, #13558, #26547, #10357, #23329, #20141, #33163, #14789, #25234, #21377, #34403, #12025, #17987, #41437, #21174, #27585, #11815 ) ),
 .UNSPECIFIED., .F., .F., .F.,
 ( 2, 2 ),
 ( 4, 2, 2, 2, 2, 2, 2, 2, 4 ),
 ( 0.000000000000000000, 1.000000000000000000 ),
 ( 0.000000000000000000, 0.06250000000000000000, 0.1250000000000000000, 0.1875000000000000000, 0.2500000000000000000, 0.3750000000000000000, 0.5000000000000000000, 0.7500000000000000000, 1.000000000000000000 ),
 .UNSPECIFIED. ) ;
#3128 = CARTESIAN_POINT ( 'NONE',  ( -0.01051219832189233434, 119.4384375980492194, 0.5260733902271049756 ) ) ;
#3129 = DIRECTION ( 'NONE',  ( 1.011795553208986377E-16, 1.000000000000000000, -0.000000000000000000 ) ) ;
#3130 = DIRECTION ( 'NONE',  ( 5.188838149069472160E-16, -1.699382548006136559E-16, -1.000000000000000000 ) ) ;
#3131 = CARTESIAN_POINT ( 'NONE',  ( -1.980194564007182745, 113.2583846565721757, 2.436415359710689010 ) ) ;
#3132 = CARTESIAN_POINT ( 'NONE',  ( 1.359589829139859152, 24.67768052395325284, 8.332721669750835503 ) ) ;
#3133 = CARTESIAN_POINT ( 'NONE',  ( 12.10601879509723844, 151.9817061558079274, 1.041216838735509409 ) ) ;
#3134 = AXIS2_PLACEMENT_3D ( 'NONE', #33597, #36580, #389 ) ;
#3135 = CARTESIAN_POINT ( 'NONE',  ( 22.21083362159523134, 150.4821223471089411, -0.6270836034604136966 ) ) ;
#3136 = DIRECTION ( 'NONE',  ( 0.9998004120163608288, 0.000000000000000000, 0.01997839162482762526 ) ) ;
#3137 = UNCERTAINTY_MEASURE_WITH_UNIT (LENGTH_MEASURE( 1.000000000000000082E-05 ), #37495, 'distance_accuracy_value', 'NONE');
#3138 = CARTESIAN_POINT ( 'NONE',  ( -4.717508175643587265, 116.7562497393984415, -0.08034061319516418165 ) ) ;
#3139 = VERTEX_POINT ( 'NONE', #18883 ) ;
#3140 = CARTESIAN_POINT ( 'NONE',  ( -6.546631412653550086, 120.5239780760649211, -1.124119359349389002 ) ) ;
#3141 = CARTESIAN_POINT ( 'NONE',  ( 23.21373371908085304, 149.6306211361744829, 0.4638656453230914356 ) ) ;
#3142 = CARTESIAN_POINT ( 'NONE',  ( -15.56637720654312851, 147.8873989650969918, -1.033077377765619698 ) ) ;
#3143 = CARTESIAN_POINT ( 'NONE',  ( 4.031918519141627577, -13.48391852982397410, 3.589295450856327729 ) ) ;
#3144 = CYLINDRICAL_SURFACE ( 'NONE', #17880, 0.5080000000000000071 ) ;
#3145 = CARTESIAN_POINT ( 'NONE',  ( 18.84770637050841202, 125.3331924886369961, 0.3953412214710180783 ) ) ;
#3146 = ORIENTED_EDGE ( 'NONE', *, *, #3265, .T. ) ;
#3147 = CARTESIAN_POINT ( 'NONE',  ( 4.627880361116947228, 7.839802885307131319, -0.3238752845059330032 ) ) ;
#3148 = CARTESIAN_POINT ( 'NONE',  ( -3.703049682113393359, 116.6240124373522065, -0.07399574541707862330 ) ) ;
#3149 = CARTESIAN_POINT ( 'NONE',  ( -4.902142009400407119, 117.4083702128866804, 0.9678786404911806640 ) ) ;
#3150 = DIRECTION ( 'NONE',  ( -0.8745520943968243532, 0.4849315768086547296, -5.361993529360573944E-16 ) ) ;
#3151 = CARTESIAN_POINT ( 'NONE',  ( -4.506407954616146405, 27.87871297014265792, 0.5132454074226986407 ) ) ;
#3152 = CARTESIAN_POINT ( 'NONE',  ( -6.073003016519146868, 120.6640402819336515, 0.7109903207712315876 ) ) ;
#3153 = CARTESIAN_POINT ( 'NONE',  ( -1.220754042303205500, 16.12054255322086860, -4.471266627502475721 ) ) ;
#3154 = CARTESIAN_POINT ( 'NONE',  ( -0.006942562093360102847, 117.0978366787122127, 0.3474341964894884782 ) ) ;
#3155 = CARTESIAN_POINT ( 'NONE',  ( 15.76285804746337504, 145.9067145067647289, 0.3149794173055761592 ) ) ;
#3157 = CARTESIAN_POINT ( 'NONE',  ( 13.77700084449465301, 121.8522644830672590, -1.120765626652496127 ) ) ;
#3156 = CARTESIAN_POINT ( 'NONE',  ( 4.825844303143274949, 56.51499999999997215, 4.829557277217847222 ) ) ;
#3158 = CARTESIAN_POINT ( 'NONE',  ( -2.426139246716550346, 10.07336736126799437, 3.943011612146583023 ) ) ;
#3159 = CARTESIAN_POINT ( 'NONE',  ( 0.01289612358321986542, 159.5048567107479585, -0.6453747585945881493 ) ) ;
#3160 = AXIS2_PLACEMENT_3D ( 'NONE', #38302, #6142, #38510 ) ;
#3161 = ORIENTED_EDGE ( 'NONE', *, *, #5173, .T. ) ;
#3162 = AXIS2_PLACEMENT_3D ( 'NONE', #9047, #22423, #3084 ) ;
#3163 = CARTESIAN_POINT ( 'NONE',  ( -0.6274479277951703349, 120.8480686026657196, 0.1451731132019953019 ) ) ;
#3164 = VECTOR ( 'NONE', #24276, 1000.000000000000000 ) ;
#3165 = CARTESIAN_POINT ( 'NONE',  ( 4.021138818454151220, -15.00176662281678475, 5.141887924562631440 ) ) ;
#3166 = CARTESIAN_POINT ( 'NONE',  ( -25.81615557310160369, 74.46796499802707103, 1.269999999999993578 ) ) ;
#3167 = VERTEX_POINT ( 'NONE', #323 ) ;
#3168 = CARTESIAN_POINT ( 'NONE',  ( 4.110343450561533274, 118.7489093234570561, 1.002437571585374831 ) ) ;
#3169 = DIRECTION ( 'NONE',  ( -1.000000000000000000, -6.353134868986659519E-16, 0.000000000000000000 ) ) ;
#3170 = DIRECTION ( 'NONE',  ( -0.9998004120163608288, 0.000000000000000000, -0.01997839162482749342 ) ) ;
#3171 = CARTESIAN_POINT ( 'NONE',  ( -20.14555658732733079, 152.4688535085772685, 0.7444337660854593031 ) ) ;
#3172 = CARTESIAN_POINT ( 'NONE',  ( 4.825435570034072086, 117.4745258938095134, -0.9995196418742542388 ) ) ;
#3173 = CARTESIAN_POINT ( 'NONE',  ( 1.399407963385772113, 159.5796833544862352, -0.3162364300534755701 ) ) ;
#3174 = DIRECTION ( 'NONE',  ( 4.017660918040594346E-17, -1.000000000000000000, -2.376309959284834438E-19 ) ) ;
#3175 = CARTESIAN_POINT ( 'NONE',  ( -46.65771312250404179, 26.07706844218929731, 1.303905986063749411 ) ) ;
#3176 = CARTESIAN_POINT ( 'NONE',  ( 5.594725610051233922, 78.91206791035247647, 5.077866005995121057 ) ) ;
#3177 = CARTESIAN_POINT ( 'NONE',  ( 1.898988921116985251, -15.25340086675062956, 5.381265105722330411 ) ) ;
#3178 = ORIENTED_EDGE ( 'NONE', *, *, #27512, .T. ) ;
#3179 = CARTESIAN_POINT ( 'NONE',  ( -43.93316818929329770, 24.49458088220322338, 1.523999999999992916 ) ) ;
#3180 = FACE_OUTER_BOUND ( 'NONE', #20121, .T. ) ;
#3181 = ADVANCED_FACE ( 'NONE', ( #33108 ), #41626, .T. ) ;
#3182 = CARTESIAN_POINT ( 'NONE',  ( -4.601728189754446419, 118.0704954893843990, 0.5721313084656637349 ) ) ;
#3183 = FACE_BOUND ( 'NONE', #18284, .T. ) ;
#3184 = AXIS2_PLACEMENT_3D ( 'NONE', #23963, #20974, #13964 ) ;
#3185 = ORIENTED_EDGE ( 'NONE', *, *, #35246, .F. ) ;
#3186 = DIRECTION ( 'NONE',  ( -0.8745520943968148053, 0.4849315768086717160, -5.691349986800521255E-16 ) ) ;
#3187 = CARTESIAN_POINT ( 'NONE',  ( -5.887631883382205444, 119.0670759175282001, -1.260654324767885859 ) ) ;
#3188 = CARTESIAN_POINT ( 'NONE',  ( -3.394470486402190623, 108.6891572770382624, -4.119616105806037432 ) ) ;
#3189 = CARTESIAN_POINT ( 'NONE',  ( 4.764019565006264223, 117.8854380970585680, 0.8884589727399109238 ) ) ;
#3190 = CARTESIAN_POINT ( 'NONE',  ( 2.664052010559913253, -13.52006206191685322, 0.08958796903007473778 ) ) ;
#3191 = CARTESIAN_POINT ( 'NONE',  ( -16.40115699206388555, 147.1833543704171348, -1.602497317185074710 ) ) ;
#3192 = CARTESIAN_POINT ( 'NONE',  ( -2.812965544484426594, 115.7033311652958787, -1.680242139021033143 ) ) ;
#3193 = CARTESIAN_POINT ( 'NONE',  ( -6.059261036834476144, 56.58343591620776181, 4.712961528314683513 ) ) ;
#3194 = CARTESIAN_POINT ( 'NONE',  ( -23.62918761621517305, 82.45577215708875940, 1.523999999999993360 ) ) ;
#3195 = CARTESIAN_POINT ( 'NONE',  ( 1.571019246621431664, 106.2535611835979239, -5.108158685570669988 ) ) ;
#3196 = CARTESIAN_POINT ( 'NONE',  ( -11.12341512264673682, 124.6236798342360856, -1.410428355923976529 ) ) ;
#3197 = ADVANCED_FACE ( 'NONE', ( #29690 ), #34806, .T. ) ;
#3198 = FACE_OUTER_BOUND ( 'NONE', #31075, .T. ) ;
#3199 = CARTESIAN_POINT ( 'NONE',  ( -0.02615319344480911481, 156.8698190429800832, 1.308812744920978322 ) ) ;
#3200 = CARTESIAN_POINT ( 'NONE',  ( -3.795109032377635749, 115.7029491485453576, 1.459792008210426539 ) ) ;
#3201 = CARTESIAN_POINT ( 'NONE',  ( 2.522041008973656240, -3.380034811851382770, 3.874746376371965173 ) ) ;
#3203 = VERTEX_POINT ( 'NONE', #28483 ) ;
#3202 = CARTESIAN_POINT ( 'NONE',  ( 3.210256534570805620, 159.4348965051207756, 0.5208765431038288041 ) ) ;
#3204 = LINE ( 'NONE', #32803, #23997 ) ;
#3205 = CARTESIAN_POINT ( 'NONE',  ( 3.752486096903807855, -15.17702595220350759, -0.4382564666907802220 ) ) ;
#3206 = CARTESIAN_POINT ( 'NONE',  ( -18.05326814683172287, 150.0321773811041339, 1.740468527814021282 ) ) ;
#3207 = CARTESIAN_POINT ( 'NONE',  ( -0.6470182227010313758, 8.987660258844066163, 0.7316552229444387434 ) ) ;
#3208 = CIRCLE ( 'NONE', #11338, 3.175000000000001155 ) ;
#3209 = CARTESIAN_POINT ( 'NONE',  ( -1.853717367163283836, 116.5907236856068181, -0.2192087907590278273 ) ) ;
#3210 = AXIS2_PLACEMENT_3D ( 'NONE', #15167, #11982, #24976 ) ;
#3211 = CARTESIAN_POINT ( 'NONE',  ( 0.9752960398044887569, 8.493769703755262412, 0.04006526980912952091 ) ) ;
#3212 = ORIENTED_EDGE ( 'NONE', *, *, #4040, .T. ) ;
#3213 = ORIENTED_EDGE ( 'NONE', *, *, #38388, .F. ) ;
#3214 = CARTESIAN_POINT ( 'NONE',  ( -47.69647088358534859, 18.57426963660985209, 3.960430087866664284 ) ) ;
#3215 = CARTESIAN_POINT ( 'NONE',  ( 4.076169972524736451, 117.8719421043398370, 0.8561738758874235522 ) ) ;
#3216 = APPLICATION_PROTOCOL_DEFINITION ( 'draft international standard', 'automotive_design', 1998, #22944 ) ;
#3217 = CARTESIAN_POINT ( 'NONE',  ( -2.684237737021801795, 120.5579296053302727, 0.3360084551914350182 ) ) ;
#3218 = CARTESIAN_POINT ( 'NONE',  ( 1.975269416564901404, -15.10067923695700109, 5.832845082603779652 ) ) ;
#3219 = CARTESIAN_POINT ( 'NONE',  ( 5.414978495245504675, 156.5090806470891209, -1.537019876316039868 ) ) ;
#3220 = CIRCLE ( 'NONE', #34506, 13.46199999999999619 ) ;
#3221 = CARTESIAN_POINT ( 'NONE',  ( -17.65052098649054813, 151.6044147853587845, -2.418251502674879205 ) ) ;
#3222 = DIRECTION ( 'NONE',  ( -0.8745520943968241312, 0.4849315768086548406, -5.691349986800536046E-16 ) ) ;
#3223 = CARTESIAN_POINT ( 'NONE',  ( 2.233078627056604759, -15.14192004606506536, 5.083345892419886880 ) ) ;
#3224 = CARTESIAN_POINT ( 'NONE',  ( -1.804899523998967803, 35.85624791583304471, 1.055339088927661262 ) ) ;
#3225 = ADVANCED_FACE ( 'NONE', ( #2728 ), #13858, .T. ) ;
#3226 = CARTESIAN_POINT ( 'NONE',  ( 9.203139800278290039, 153.8854248570426080, -0.2095608753156673887 ) ) ;
#3227 = CIRCLE ( 'NONE', #8661, 0.2539999999999992819 ) ;
#3228 = ORIENTED_EDGE ( 'NONE', *, *, #6639, .F. ) ;
#3229 = DIRECTION ( 'NONE',  ( 0.6559537821943236535, -0.7548010569845287066, 4.686333752532406881E-16 ) ) ;
#3230 = EDGE_CURVE ( 'NONE', #25709, #9800, #4902, .T. ) ;
#3231 = LINE ( 'NONE', #13229, #9569 ) ;
#3232 = ADVANCED_FACE ( 'NONE', ( #14324 ), #35503, .T. ) ;
#3233 = FACE_OUTER_BOUND ( 'NONE', #39932, .T. ) ;
#3234 = CARTESIAN_POINT ( 'NONE',  ( -16.04309792416813707, 12.96416000000000146, 5.016499999999999737 ) ) ;
#3235 = CARTESIAN_POINT ( 'NONE',  ( 1.419391870195661376, 159.6052071245950970, -0.01540741456718461473 ) ) ;
#3236 = CARTESIAN_POINT ( 'NONE',  ( -7.328771362700684300, 123.0350022594044219, -0.07777345538050987883 ) ) ;
#3237 = PRESENTATION_LAYER_ASSIGNMENT (  '', '', ( #21570 ) ) ;
#3238 = CARTESIAN_POINT ( 'NONE',  ( -6.733080298864849599E-14, 123.6644662015457214, 4.141858957710797243E-18 ) ) ;
#3239 = DIRECTION ( 'NONE',  ( 0.1469470846586743706, -1.414713986243376972E-17, 0.9891443546370348727 ) ) ;
#3240 = CARTESIAN_POINT ( 'NONE',  ( 0.8256988760359594837, 37.88232708988313391, -1.149614905092997796 ) ) ;
#3241 = CARTESIAN_POINT ( 'NONE',  ( 14.79112219052226784, 123.2524255416106342, 1.763561952744266081 ) ) ;
#3242 = CARTESIAN_POINT ( 'NONE',  ( -0.2501726036287156840, 25.39126883368370002, -4.616104092076634302 ) ) ;
#3243 = CARTESIAN_POINT ( 'NONE',  ( -3.184215270518052421, -12.39116543543024562, -7.798991864805400631 ) ) ;
#3244 = CARTESIAN_POINT ( 'NONE',  ( -8.715807593838684753, 118.0255461215873254, -0.7900476978637416270 ) ) ;
#3245 = CARTESIAN_POINT ( 'NONE',  ( -0.7524737301091138919, 120.0979018405971175, -0.6085003676253138982 ) ) ;
#3246 = DIRECTION ( 'NONE',  ( -0.8745520943968243532, 0.4849315768086547296, -6.829619984160642269E-16 ) ) ;
#3247 = CARTESIAN_POINT ( 'NONE',  ( 0.2371669961381878411, 105.9788885827711340, -5.291421317388997458 ) ) ;
#3248 = CARTESIAN_POINT ( 'NONE',  ( 2.608302318560305366, 105.1243950483077185, 4.653828818123431077 ) ) ;
#3249 = CARTESIAN_POINT ( 'NONE',  ( 0.6590154617207463206, 19.50938314818779062, -4.574821423538240950 ) ) ;
#3250 = DIRECTION ( 'NONE',  ( -0.8745520943968235761, 0.4849315768086558398, -4.268512490100410909E-16 ) ) ;
#3251 = DIRECTION ( 'NONE',  ( 9.627370216492862708E-17, 1.000000000000000000, -0.000000000000000000 ) ) ;
#3252 = CARTESIAN_POINT ( 'NONE',  ( 3.216637634036228821, -14.25892527173770752, 2.941440830758975888 ) ) ;
#3253 = CARTESIAN_POINT ( 'NONE',  ( 3.292372560053815178, 124.4927030837263118, 0.04348745598417508296 ) ) ;
#3254 = CARTESIAN_POINT ( 'NONE',  ( -22.15286039372332993, 136.9573810088325843, 0.3857095667871865974 ) ) ;
#3255 = CIRCLE ( 'NONE', #27716, 6.350000000000004974 ) ;
#3256 = ORIENTED_EDGE ( 'NONE', *, *, #25445, .F. ) ;
#3257 = DIRECTION ( 'NONE',  ( -0.9998501190848629872, -0.01731298258490740830, -8.537024980200807027E-16 ) ) ;
#3258 = ORIENTED_EDGE ( 'NONE', *, *, #6887, .T. ) ;
#3259 = DIRECTION ( 'NONE',  ( 6.353134868986659519E-16, -1.000000000000000000, 0.000000000000000000 ) ) ;
#3260 = CARTESIAN_POINT ( 'NONE',  ( 2.577823224604873786, -15.72362945599133077, 5.534267358606157039 ) ) ;
#3261 = CARTESIAN_POINT ( 'NONE',  ( -14.47132921234248748, 123.3930721568691382, 1.260850717050816083 ) ) ;
#3262 = CARTESIAN_POINT ( 'NONE',  ( 15.81089186882080710, 155.0373533369262589, -1.166412807380551309 ) ) ;
#3263 = CARTESIAN_POINT ( 'NONE',  ( 4.076717266748975277, 8.489475128091552136, -2.202413229635628689 ) ) ;
#3264 = CARTESIAN_POINT ( 'NONE',  ( -58.69116746987842959, -0.3144157293073903681, -0.2986533189990187576 ) ) ;
#3265 = EDGE_CURVE ( 'NONE', #25412, #27671, #1563, .T. ) ;
#3266 = VERTEX_POINT ( 'NONE', #26912 ) ;
#3267 = CARTESIAN_POINT ( 'NONE',  ( -58.40429423216704663, -0.3346038877942508760, -0.4235997928873705964 ) ) ;
#3268 = CARTESIAN_POINT ( 'NONE',  ( -0.003073426023290456131, 123.4679809879534247, 0.1538068059577046287 ) ) ;
#3269 = DIRECTION ( 'NONE',  ( -1.000000000000000000, 1.044409991968846932E-16, 0.000000000000000000 ) ) ;
#3270 = CARTESIAN_POINT ( 'NONE',  ( -17.57956382101115622, 146.6691408387931688, 1.464727724346842397 ) ) ;
#3271 = DIRECTION ( 'NONE',  ( -5.188838149069472160E-16, 1.699382548006136559E-16, 1.000000000000000000 ) ) ;
#3272 = CARTESIAN_POINT ( 'NONE',  ( 12.30591244053531774, 123.0735437985678971, -1.316165607245708413 ) ) ;
#3273 = CARTESIAN_POINT ( 'NONE',  ( -13.36424875645665900, 155.6061939908119882, -2.069718186823301664 ) ) ;
#3274 = CARTESIAN_POINT ( 'NONE',  ( -5.653927021192587610, 78.90752773945908416, 4.880377097574616130 ) ) ;
#3275 = AXIS2_PLACEMENT_3D ( 'NONE', #6670, #19223, #39468 ) ;
#3276 = ORIENTED_EDGE ( 'NONE', *, *, #3870, .T. ) ;
#3277 = CARTESIAN_POINT ( 'NONE',  ( 4.486692410979344459, 118.1299448241766186, -0.5327426128926098237 ) ) ;
#3278 = CARTESIAN_POINT ( 'NONE',  ( 16.05525886874792718, 145.8417561620165372, -0.5351738620951715930 ) ) ;
#3279 = EDGE_LOOP ( 'NONE', ( #29860, #37245, #7086, #6080 ) ) ;
#3280 = CARTESIAN_POINT ( 'NONE',  ( -17.70445710129711259, 147.3864036964934598, -2.239206817186280229 ) ) ;
#3281 = CARTESIAN_POINT ( 'NONE',  ( 3.462569250300066681, -15.15729918637651075, 2.757833548007345037 ) ) ;
#3282 = CARTESIAN_POINT ( 'NONE',  ( 3.032540074886261205, 105.1244957488249980, -4.437742800387862729 ) ) ;
#3283 = EDGE_CURVE ( 'NONE', #40944, #23764, #32088, .T. ) ;
#3284 = CARTESIAN_POINT ( 'NONE',  ( 14.50851225146812240, 78.09971119798316863, -5.392902600000141433 ) ) ;
#3285 = CARTESIAN_POINT ( 'NONE',  ( -4.776051034590975242, 117.6653734182690556, 0.9389516368186912043 ) ) ;
#3286 = CARTESIAN_POINT ( 'NONE',  ( 10.53370020345040103, 154.2769816202975051, 1.888232850154635045 ) ) ;
#3287 = CARTESIAN_POINT ( 'NONE',  ( -46.58649794690494872, 25.68081001442251221, 1.571531081468684032 ) ) ;
#3288 = CARTESIAN_POINT ( 'NONE',  ( 8.408789229792210662, -11.58028725773715628, 0.1531400924992341317 ) ) ;
#3289 = CARTESIAN_POINT ( 'NONE',  ( 15.80103543825234880, 146.2514283349100594, 0.5462135236119776138 ) ) ;
#3290 = DIRECTION ( 'NONE',  ( -0.2883665106726627791, -0.9575201071113198514, -8.211810011157224448E-16 ) ) ;
#3292 = ORIENTED_EDGE ( 'NONE', *, *, #3466, .T. ) ;
#3291 = CARTESIAN_POINT ( 'NONE',  ( -47.74911022259793469, 17.86741523025699152, -3.129844374475875934 ) ) ;
#3293 = PLANE ( 'NONE',  #20297 ) ;
#3294 = CARTESIAN_POINT ( 'NONE',  ( -48.00704091872448487, 20.04541143072568232, 5.176114466449816653 ) ) ;
#3295 = CARTESIAN_POINT ( 'NONE',  ( -17.97610982144389524, 83.97333317030323485, 1.269999999999995799 ) ) ;
#3296 = LINE ( 'NONE', #321, #32462 ) ;
#3297 = AXIS2_PLACEMENT_3D ( 'NONE', #39203, #32181, #31969 ) ;
#3298 = DIRECTION ( 'NONE',  ( 0.8745520943968235761, -0.4849315768086558398, 4.268512490100410909E-16 ) ) ;
#3299 = CARTESIAN_POINT ( 'NONE',  ( -6.194847070882102180, 64.72978607931611350, 1.270000000000005125 ) ) ;
#3300 = CARTESIAN_POINT ( 'NONE',  ( -55.64884842185075087, 8.819639511685364752, 1.021878145082198763 ) ) ;
#3301 = CARTESIAN_POINT ( 'NONE',  ( -57.09878488423309051, 3.216020309495956742, 2.217633722229532367 ) ) ;
#3302 = CARTESIAN_POINT ( 'NONE',  ( -14.68764241912311519, 120.3119357913517291, 0.01896423869846143237 ) ) ;
#3303 = ORIENTED_EDGE ( 'NONE', *, *, #19897, .T. ) ;
#3304 = CARTESIAN_POINT ( 'NONE',  ( -50.72152632752359125, 17.59631655692102470, -3.767527310968358911 ) ) ;
#3305 = CARTESIAN_POINT ( 'NONE',  ( -6.059742184461669900, 121.4333258338537291, -0.1238882853059191380 ) ) ;
#3306 = ORIENTED_EDGE ( 'NONE', *, *, #35725, .T. ) ;
#3307 = CARTESIAN_POINT ( 'NONE',  ( -15.65552799280940022, 147.2250547476223801, -0.5422809309331373395 ) ) ;
#3308 = CARTESIAN_POINT ( 'NONE',  ( 5.456921283009238621, -14.23391906346564717, 3.426434758229824240 ) ) ;
#3309 = CARTESIAN_POINT ( 'NONE',  ( -12.17409717887521303, 120.5818589831333441, 1.028275848330292952 ) ) ;
#3310 = DIRECTION ( 'NONE',  ( -0.9816537812491089587, -0.1906721105965065444, -4.769617732184475162E-16 ) ) ;
#3311 = CARTESIAN_POINT ( 'NONE',  ( 15.13553065988576307, 156.1345691653134509, 0.5893329488795889803 ) ) ;
#3312 = CARTESIAN_POINT ( 'NONE',  ( 0.6398660015929856781, 156.3034662015459446, 0.08424640074850882343 ) ) ;
#3313 = CARTESIAN_POINT ( 'NONE',  ( 4.831486089547707863, 118.5266822147775940, -0.7499602601522077361 ) ) ;
#3314 = CARTESIAN_POINT ( 'NONE',  ( 0.05241920358452190065, 15.83596528477922405, 0.9742995972537078497 ) ) ;
#3315 = CARTESIAN_POINT ( 'NONE',  ( -5.738526254234522561, 159.1207877133979309, -0.2162537097210230630 ) ) ;
#3316 = DIRECTION ( 'NONE',  ( -0.9998004120163609398, 0.000000000000000000, -0.01997839162482749689 ) ) ;
#3317 = CARTESIAN_POINT ( 'NONE',  ( -18.19824605342069290, 84.09650579081264254, 1.269999999999996465 ) ) ;
#3318 = ORIENTED_EDGE ( 'NONE', *, *, #27124, .T. ) ;
#3319 = CARTESIAN_POINT ( 'NONE',  ( 2.394807681685032552, 116.5915636595390623, 0.4284483426437976639 ) ) ;
#3320 = ORIENTED_EDGE ( 'NONE', *, *, #24903, .T. ) ;
#3321 = DIRECTION ( 'NONE',  ( -0.1469470846586743706, 1.414713986243376972E-17, -0.9891443546370348727 ) ) ;
#3322 = CARTESIAN_POINT ( 'NONE',  ( 21.52870603658934812, 148.1022500232506616, 2.247031159961964342 ) ) ;
#3323 = CARTESIAN_POINT ( 'NONE',  ( 12.49437611722087205, 122.1796674805547980, -1.295212323302052937 ) ) ;
#3324 = CARTESIAN_POINT ( 'NONE',  ( -0.9744428630873758213, 7.697845052497760854, 0.001242513977635927719 ) ) ;
#3325 = CARTESIAN_POINT ( 'NONE',  ( 6.022233187337456606, 12.22246943312702427, 5.887876567768997482 ) ) ;
#3326 = AXIS2_PLACEMENT_3D ( 'NONE', #13453, #16635, #4514 ) ;
#3327 = CARTESIAN_POINT ( 'NONE',  ( -21.50396862640735307, 149.5883454796168621, -2.135274339423805401 ) ) ;
#3328 = CARTESIAN_POINT ( 'NONE',  ( 4.703873350422621336, 117.8348676116459472, -0.8530165572518777495 ) ) ;
#3329 = CARTESIAN_POINT ( 'NONE',  ( -19.33375693323417366, 80.42273151551299293, 1.523999999999995802 ) ) ;
#3330 = CARTESIAN_POINT ( 'NONE',  ( 3.544426656953406862, 120.3814187630814132, -0.4774784233729820193 ) ) ;
#3331 = CARTESIAN_POINT ( 'NONE',  ( -0.0005023639978753125738, 120.9974662015457056, 0.02514034870427569318 ) ) ;
#3332 = ORIENTED_EDGE ( 'NONE', *, *, #19873, .T. ) ;
#3333 = CARTESIAN_POINT ( 'NONE',  ( -4.079782966556147805, 157.3082466949932723, -1.825029598092313687 ) ) ;
#3334 = ADVANCED_FACE ( 'NONE', ( #40347 ), #8283, .T. ) ;
#3335 = CARTESIAN_POINT ( 'NONE',  ( 6.125566448072323311, -14.60357603047697594, -0.1915981853098273624 ) ) ;
#3336 = CARTESIAN_POINT ( 'NONE',  ( 5.240472681551541889, 115.6909491485453145, 1.017784315483886814 ) ) ;
#3337 = EDGE_CURVE ( 'NONE', #10933, #31748, #29980, .T. ) ;
#3338 = CARTESIAN_POINT ( 'NONE',  ( -48.04822308881582416, 19.89521662531995005, -5.294633059834412236 ) ) ;
#3339 = ORIENTED_EDGE ( 'NONE', *, *, #25682, .F. ) ;
#3340 = CARTESIAN_POINT ( 'NONE',  ( 4.224706347173564858, 119.5670751559891585, 0.9504096833562339919 ) ) ;
#3341 = DIRECTION ( 'NONE',  ( -1.000000000000000000, 0.000000000000000000, 4.553079989440437711E-16 ) ) ;
#3342 = AXIS2_PLACEMENT_3D ( 'NONE', #39599, #30984, #26590 ) ;
#3343 = TOROIDAL_SURFACE ( 'NONE', #27792, 0.3810000000000002829, 0.2540000000000000036 ) ;
#3344 = DIRECTION ( 'NONE',  ( -5.188838149069472160E-16, 1.699382548006136559E-16, 1.000000000000000000 ) ) ;
#3345 = CARTESIAN_POINT ( 'NONE',  ( -2.274554406286753316, 117.6064948828932444, 1.027890184761801384 ) ) ;
#3346 = CARTESIAN_POINT ( 'NONE',  ( 6.528609751734300914, 25.78175851779908356, 5.377075232920663694 ) ) ;
#3347 = CARTESIAN_POINT ( 'NONE',  ( 9.400309931224008153, 124.0858766813489780, 0.6109843400649571654 ) ) ;
#3348 = CARTESIAN_POINT ( 'NONE',  ( 1.955870317219520871, 116.9162416783649689, -0.3393494064863859516 ) ) ;
#3349 = CARTESIAN_POINT ( 'NONE',  ( -47.84356795211461844, 19.38525671449500010, -5.197506975155170572 ) ) ;
#3350 = FACE_OUTER_BOUND ( 'NONE', #5948, .T. ) ;
#3351 = CARTESIAN_POINT ( 'NONE',  ( -11.73725613052212324, 118.7267541726749869, -0.2187512536375164351 ) ) ;
#3352 = ORIENTED_EDGE ( 'NONE', *, *, #19649, .F. ) ;
#3353 = CARTESIAN_POINT ( 'NONE',  ( 8.152322075550674896, 120.9500479307340299, -1.022460547729552083 ) ) ;
#3354 = DIRECTION ( 'NONE',  ( 0.9336303900108815501, 0.3582377630124009560, 4.235673982319039874E-16 ) ) ;
#3355 = CARTESIAN_POINT ( 'NONE',  ( -10.59645057104367716, 153.0636280899912549, -0.8695332296301786501 ) ) ;
#3356 = CARTESIAN_POINT ( 'NONE',  ( 2.309263497243444263, -14.96449433386182193, 5.702862618531368888 ) ) ;
#3357 = CARTESIAN_POINT ( 'NONE',  ( -5.148936812350190628, 116.8706406773187894, 0.04504664567876282694 ) ) ;
#3358 = CARTESIAN_POINT ( 'NONE',  ( 17.29877781292318417, 122.7677429521249053, 0.3633837628929261210 ) ) ;
#3359 = ORIENTED_EDGE ( 'NONE', *, *, #10292, .F. ) ;
#3360 = CARTESIAN_POINT ( 'NONE',  ( -2.406711483539481389, 4.503775517365914638, 3.979180414515509412 ) ) ;
#3361 = CARTESIAN_POINT ( 'NONE',  ( -6.439947148575337965E-14, 116.4254662015457313, 1.493913655526859821E-16 ) ) ;
#3362 = CARTESIAN_POINT ( 'NONE',  ( -4.902238121359880019, 117.4071601550653838, 0.9680467791073505968 ) ) ;
#3363 = LINE ( 'NONE', #6762, #28527 ) ;
#3364 = CARTESIAN_POINT ( 'NONE',  ( 7.898376164620551698, 121.9960575332709425, 0.9517411587677502283 ) ) ;
#3365 = AXIS2_PLACEMENT_3D ( 'NONE', #37717, #35158, #38560 ) ;
#3366 = CARTESIAN_POINT ( 'NONE',  ( 1.368391094521330897, 11.37271669962338372, 4.434453701053673313 ) ) ;
#3367 = CARTESIAN_POINT ( 'NONE',  ( 1.027358375535017521, 117.1967307433898640, 0.4586652788708822093 ) ) ;
#3369 = VECTOR ( 'NONE', #13402, 1000.000000000000000 ) ;
#3368 = DIRECTION ( 'NONE',  ( -5.188838149069472160E-16, 1.699382548006136559E-16, 1.000000000000000000 ) ) ;
#3371 = CARTESIAN_POINT ( 'NONE',  ( 20.76034172958447499, 149.5879773183856685, -1.515053003442401458 ) ) ;
#3370 = CARTESIAN_POINT ( 'NONE',  ( 5.449227423779250401, 57.14999999999996305, 5.145694933688582218 ) ) ;
#3372 = CARTESIAN_POINT ( 'NONE',  ( -3.833338661037195561, 9.423677021345861604, 2.587938769098377279 ) ) ;
#3373 = CARTESIAN_POINT ( 'NONE',  ( -20.09973570640927676, 152.4688535085772685, -1.548630484586873024 ) ) ;
#3374 = VERTEX_POINT ( 'NONE', #37137 ) ;
#3375 = CARTESIAN_POINT ( 'NONE',  ( -15.33898570969108910, 143.5038931315047535, 0.1524207748662386730 ) ) ;
#3376 = CARTESIAN_POINT ( 'NONE',  ( 5.208971126070756519, -14.02307540452116186, 3.677211492609324228 ) ) ;
#3377 = DIRECTION ( 'NONE',  ( 1.000000000000000000, 1.004817652842027660E-15, 0.000000000000000000 ) ) ;
#3378 = CARTESIAN_POINT ( 'NONE',  ( 3.150244473240279675, -14.07033042043420146, 1.813758411523331393 ) ) ;
#3379 = ADVANCED_FACE ( 'NONE', ( #14538 ), #7331, .F. ) ;
#3380 = VERTEX_POINT ( 'NONE', #37341 ) ;
#3381 = CARTESIAN_POINT ( 'NONE',  ( 4.285767465938623566, 157.6046910967438066, 1.850878756276731485 ) ) ;
#3382 = CARTESIAN_POINT ( 'NONE',  ( 6.113380087472956159E-17, 0.6350000000000001199, 0.000000000000000000 ) ) ;
#3383 = DIRECTION ( 'NONE',  ( -5.188838149069471174E-16, 1.699382548006136313E-16, 1.000000000000000000 ) ) ;
#3384 = CARTESIAN_POINT ( 'NONE',  ( -22.52700986351724310, 149.9757045183965261, 0.6247156920787648726 ) ) ;
#3385 = TOROIDAL_SURFACE ( 'NONE', #26527, 0.7620000000000000107, 0.2540000000000000036 ) ;
#3386 = CARTESIAN_POINT ( 'NONE',  ( 1.881116149107284752, 116.6503132507590124, -0.1904188032791131469 ) ) ;
#3387 = AXIS2_PLACEMENT_3D ( 'NONE', #32321, #6550, #16756 ) ;
#3388 = CARTESIAN_POINT ( 'NONE',  ( -13.85159022459153988, 59.63164443796365077, 5.016499999999999737 ) ) ;
#3389 =( REPRESENTATION_RELATIONSHIP ('NONE','NONE', #30767, #11484 ) REPRESENTATION_RELATIONSHIP_WITH_TRANSFORMATION ( #1499 )SHAPE_REPRESENTATION_RELATIONSHIP( ) );
#3390 = CARTESIAN_POINT ( 'NONE',  ( -51.34742739204327222, 13.85210956937153348, 4.439032809404257485 ) ) ;
#3391 = CARTESIAN_POINT ( 'NONE',  ( 5.736468567008338404, 78.90050738914777639, 5.037638016205330693 ) ) ;
#3392 = CARTESIAN_POINT ( 'NONE',  ( 16.04309792416813707, 12.96416000000000146, 5.016499999999999737 ) ) ;
#3393 = CARTESIAN_POINT ( 'NONE',  ( -51.09990735641632398, 14.52648110433587370, 4.713018929684107405 ) ) ;
#3394 = DIRECTION ( 'NONE',  ( -0.9998004120163609398, 0.000000000000000000, -0.01997839162482749689 ) ) ;
#3395 = CARTESIAN_POINT ( 'NONE',  ( -4.656930922224128189, 118.0313578534626089, 0.5881568660916046687 ) ) ;
#3396 = CARTESIAN_POINT ( 'NONE',  ( -5.654802103384504619, 78.90710107780492422, -5.057831774704119709 ) ) ;
#3397 = EDGE_LOOP ( 'NONE', ( #41828, #17194, #23312, #35964 ) ) ;
#3398 = CARTESIAN_POINT ( 'NONE',  ( 0.02551629668039365542, 118.7629491485454025, -1.276939826301569658 ) ) ;
#3399 = CARTESIAN_POINT ( 'NONE',  ( -3.418166037675369306, 118.5938114843297342, -0.9285938376095641544 ) ) ;
#3400 = CARTESIAN_POINT ( 'NONE',  ( -4.713882987175448847, 112.7966860322829206, -2.559857038700545928 ) ) ;
#3401 = CARTESIAN_POINT ( 'NONE',  ( 4.706919409142078514, 117.7550815031327573, 1.085396228939788932 ) ) ;
#3402 = CARTESIAN_POINT ( 'NONE',  ( -47.01067208220106863, 24.90190543975541360, -1.870441909736414221 ) ) ;
#3403 = CARTESIAN_POINT ( 'NONE',  ( -9.757351933493584539, 123.8372022493589100, -0.9812814142356128810 ) ) ;
#3404 = CARTESIAN_POINT ( 'NONE',  ( -3.088186736232249263, 115.7029548917814026, -1.663143839991825468 ) ) ;
#3405 = LINE ( 'NONE', #22962, #37379 ) ;
#3406 = DIRECTION ( 'NONE',  ( 5.206863593109713661E-17, -1.000000000000000000, 1.077750396879097183E-30 ) ) ;
#3407 = CARTESIAN_POINT ( 'NONE',  ( 0.8777885371162424955, 105.9485402691003060, -5.279836415571006469 ) ) ;
#3408 = CARTESIAN_POINT ( 'NONE',  ( -16.06787389343327277, 149.3012944676311804, -2.013231008103360864 ) ) ;
#3409 = CARTESIAN_POINT ( 'NONE',  ( -13.83234216238653858, 16.68269501491596785, -5.016499999999998849 ) ) ;
#3410 = CARTESIAN_POINT ( 'NONE',  ( -0.03153862713815891450, 157.4657262375360176, 1.578321868909182690 ) ) ;
#3411 = CARTESIAN_POINT ( 'NONE',  ( -28.36525985791271154, 77.02308833105713859, 1.269999999999991580 ) ) ;
#3412 = CARTESIAN_POINT ( 'NONE',  ( -2.879335978063669810, 156.0997340136324851, -0.01403285518562221064 ) ) ;
#3413 = ADVANCED_FACE ( 'NONE', ( #4985 ), #17943, .T. ) ;
#3414 = CARTESIAN_POINT ( 'NONE',  ( -3.812863311134618183, 2.017465188139291765, -2.614655560905410958 ) ) ;
#3416 = ORIENTED_EDGE ( 'NONE', *, *, #10958, .T. ) ;
#3415 = CARTESIAN_POINT ( 'NONE',  ( 7.903286925170525556, 158.6683511845044734, 0.6884992853041227434 ) ) ;
#3417 = CARTESIAN_POINT ( 'NONE',  ( 4.808131379915038472, 104.6144662015457669, -0.4149153341867673483 ) ) ;
#3418 = CARTESIAN_POINT ( 'NONE',  ( 3.847030120444227208, -15.22745156820166912, 0.3463556848800000143 ) ) ;
#3419 = CARTESIAN_POINT ( 'NONE',  ( -5.877700541659460320, 119.5807162246413498, 0.9453723347071266714 ) ) ;
#3420 = CARTESIAN_POINT ( 'NONE',  ( 0.1873809172457601979, 14.59626481882237492, -0.9553521702420578743 ) ) ;
#3421 = CARTESIAN_POINT ( 'NONE',  ( -22.84108495963322838, 150.1122123445777277, -1.048654020290956224 ) ) ;
#3422 = CARTESIAN_POINT ( 'NONE',  ( 0.8051319862491574941, 7.640635046448309708, 0.5515409728216702501 ) ) ;
#3423 = ORIENTED_EDGE ( 'NONE', *, *, #6687, .T. ) ;
#3424 = EDGE_CURVE ( 'NONE', #33118, #4862, #30711, .T. ) ;
#3425 = AXIS2_PLACEMENT_3D ( 'NONE', #9397, #250, #6420 ) ;
#3426 = ORIENTED_EDGE ( 'NONE', *, *, #30280, .F. ) ;
#3427 = CARTESIAN_POINT ( 'NONE',  ( -42.09164859969784089, 21.98995510696678934, 0.2271816505417205145 ) ) ;
#3428 = CARTESIAN_POINT ( 'NONE',  ( 1.786380800136739833, 106.8720524443079967, 4.898415999051429992 ) ) ;
#3429 = CARTESIAN_POINT ( 'NONE',  ( -10.29759560803370277, 124.8461398015159745, 0.5204633524205696249 ) ) ;
#3430 = CARTESIAN_POINT ( 'NONE',  ( 4.137648320759505616, -13.26899632091267733, 3.249298663494996298 ) ) ;
#3431 = CARTESIAN_POINT ( 'NONE',  ( 11.07124803888933506, 123.5714170083676748, -1.086458317614992231 ) ) ;
#3432 = CARTESIAN_POINT ( 'NONE',  ( -2.300165013716055196, 118.7486697826011977, -0.8022418554901108445 ) ) ;
#3433 = CARTESIAN_POINT ( 'NONE',  ( -47.85244527695891037, 19.39403540832952544, -5.219971639306605127 ) ) ;
#3434 = EDGE_CURVE ( 'NONE', #31942, #3896, #27315, .T. ) ;
#3435 = CARTESIAN_POINT ( 'NONE',  ( 2.356490753556696571, -15.00856118213019030, 5.009515689243722925 ) ) ;
#3436 = CARTESIAN_POINT ( 'NONE',  ( -0.09153888643297225514, 38.16702564188061331, -1.140315812098650960 ) ) ;
#3437 = CARTESIAN_POINT ( 'NONE',  ( 7.884012465051688956, 154.6027768716304820, -0.2197914096094749914 ) ) ;
#3438 = ORIENTED_EDGE ( 'NONE', *, *, #14708, .F. ) ;
#3439 = CARTESIAN_POINT ( 'NONE',  ( -4.659482878567669850, 112.0093730493838819, 2.672389468958488834 ) ) ;
#3440 = DIRECTION ( 'NONE',  ( -0.9998004119305863302, -1.254898720634597213E-08, -0.01997839591733275785 ) ) ;
#3441 = CARTESIAN_POINT ( 'NONE',  ( -28.09515292912719175, 77.51021392068167870, -1.270000000000007345 ) ) ;
#3442 = TOROIDAL_SURFACE ( 'NONE', #4817, 8.794749999999996959, 0.2540000000000000036 ) ;
#3443 = CYLINDRICAL_SURFACE ( 'NONE', #2180, 0.5080000000000000071 ) ;
#3444 = ADVANCED_FACE ( 'NONE', ( #27748 ), #14962, .T. ) ;
#3445 = CYLINDRICAL_SURFACE ( 'NONE', #40339, 2.539999999999999591 ) ;
#3446 = CARTESIAN_POINT ( 'NONE',  ( 13.64797835309719076, 119.6379125180634446, 0.1726152169769649691 ) ) ;
#3447 = CARTESIAN_POINT ( 'NONE',  ( -6.943414100881930118, 121.8132169909553966, 0.01755787080488258392 ) ) ;
#3448 = AXIS2_PLACEMENT_3D ( 'NONE', #4549, #17507, #1347 ) ;
#3449 = CARTESIAN_POINT ( 'NONE',  ( -2.253372707275640430, 115.6909491485452577, 1.622700018657069920 ) ) ;
#3450 = CARTESIAN_POINT ( 'NONE',  ( 1.686640475165922748, -9.627085671684914914, -4.319569293544198274 ) ) ;
#3451 = CARTESIAN_POINT ( 'NONE',  ( -4.854047724237823047, 31.68081860726809751, -0.1332975631430312891 ) ) ;
#3452 = CARTESIAN_POINT ( 'NONE',  ( 10.46214381725860498, 120.0128241960130424, 1.483189230905844758 ) ) ;
#3453 = EDGE_CURVE ( 'NONE', #37511, #3974, #10137, .T. ) ;
#3454 = CARTESIAN_POINT ( 'NONE',  ( -0.8806307086779237014, 20.21867702141905099, 4.540528814573361771 ) ) ;
#3455 = CARTESIAN_POINT ( 'NONE',  ( -2.299398447937291756, 29.65396322172144039, -8.101725167555347440 ) ) ;
#3456 = CARTESIAN_POINT ( 'NONE',  ( -8.699715645159683319, 118.0981485975619734, -0.8502983169828192134 ) ) ;
#3457 = CARTESIAN_POINT ( 'NONE',  ( -0.7855309748069307929, 120.8419495465347069, -0.4764688261655855017 ) ) ;
#3458 = CARTESIAN_POINT ( 'NONE',  ( -23.34372044208206631, 149.0681261006343163, -0.4664630893998606975 ) ) ;
#3459 = CARTESIAN_POINT ( 'NONE',  ( 1.119229806841262498, 106.1659139100990785, -5.173940658946511562 ) ) ;
#3460 = CARTESIAN_POINT ( 'NONE',  ( -1.280639713796333012, 104.6144662015413331, 5.189622541085106455 ) ) ;
#3461 = CARTESIAN_POINT ( 'NONE',  ( 3.043391175932955495, 18.63480288530714191, -3.501419995799015528 ) ) ;
#3462 = DIRECTION ( 'NONE',  ( 0.9998004120163608288, 0.000000000000000000, 0.01997839162482750383 ) ) ;
#3463 = LINE ( 'NONE', #9627, #40991 ) ;
#3464 = CARTESIAN_POINT ( 'NONE',  ( 2.931439949929583122, -14.82325452411255640, 4.117531814738872420 ) ) ;
#3465 = AXIS2_PLACEMENT_3D ( 'NONE', #40175, #13957, #10348 ) ;
#3466 = EDGE_CURVE ( 'NONE', #16450, #8022, #18188, .T. ) ;
#3467 = CARTESIAN_POINT ( 'NONE',  ( 2.121281617406954645, 114.8832439220486350, -1.889083087725354826 ) ) ;
#3468 = CARTESIAN_POINT ( 'NONE',  ( -23.06568927493573895, 148.7220611141358404, 0.3950670065760724659 ) ) ;
#3469 = ORIENTED_EDGE ( 'NONE', *, *, #5401, .T. ) ;
#3470 = CARTESIAN_POINT ( 'NONE',  ( 5.965356522962860453, 53.58606249999999704, 5.016499999999999737 ) ) ;
#3471 = ORIENTED_EDGE ( 'NONE', *, *, #4804, .T. ) ;
#3472 = CARTESIAN_POINT ( 'NONE',  ( -5.250802080936233907, 115.7029491485453718, 0.9230947160017799469 ) ) ;
#3473 = CARTESIAN_POINT ( 'NONE',  ( 3.918620257527314799, -15.59263167233598857, 4.836928646374421881 ) ) ;
#3474 = CARTESIAN_POINT ( 'NONE',  ( -5.882864265865931586, 118.8996324090661147, 0.9452689120681909696 ) ) ;
#3475 = AXIS2_PLACEMENT_3D ( 'NONE', #16288, #25880, #29078 ) ;
#3476 = CARTESIAN_POINT ( 'NONE',  ( 9.838452836889429065, 157.5983698538113629, -1.280564089889915547 ) ) ;
#3477 = EDGE_CURVE ( 'NONE', #20581, #20298, #10043, .T. ) ;
#3478 = B_SPLINE_CURVE_WITH_KNOTS ( 'NONE', 3,
 ( #21225, #37857, #21431, #8253, #18241, #11032, #27224, #30412, #34256, #5085, #14840, #27845, #24861, #4873, #11654, #28052 ),
 .UNSPECIFIED., .F., .F.,
 ( 4, 2, 2, 2, 2, 2, 2, 4 ),
 ( 0.000000000000000000, 0.005261262525262890531, 0.007891893787894345771, 0.01052252505052580014, 0.01578378757578872624, 0.01709910320710445950, 0.01841441883842019275, 0.02104505010105165580 ),
 .UNSPECIFIED. ) ;
#3479 = CARTESIAN_POINT ( 'NONE',  ( -0.8823465807374654135, 5.041073445128725794, 4.537322665494407659 ) ) ;
#3480 = CARTESIAN_POINT ( 'NONE',  ( -58.65524206761604376, -0.3162046652864728413, -0.3252180803564949096 ) ) ;
#3481 = VERTEX_POINT ( 'NONE', #31998 ) ;
#3482 = LINE ( 'NONE', #16442, #39497 ) ;
#3483 = CARTESIAN_POINT ( 'NONE',  ( 0.3783624953763569110, 110.0486234891351245, 3.695659563127995373 ) ) ;
#3484 = CARTESIAN_POINT ( 'NONE',  ( -4.646525074885831330, 117.9326234303812555, 0.7781659370121971619 ) ) ;
#3485 = B_SPLINE_SURFACE_WITH_KNOTS ( 'NONE', 3, 3, ( 
 ( #9925, #19711, #32731, #13551, #996, #7797, #17566, #1408, #30569, #23958, #26541, #577, #23746, #40385, #36976, #39548, #30353, #4611, #33574, #783, #14364, #16733, #33157, #10351, #11180, #4408, #27375, #40178, #7174, #36765, #23322, #36358, #23531, #10974, #37174, #20758, #24165, #13758, #33783, #19928, #32945, #3774, #17365, #13960, #29737, #7584, #26755 ),
 ( #20335, #20545, #10559, #20133, #3985, #39973, #27168, #16945, #30155, #29943, #1202, #26959, #39764, #14162, #36558, #10764, #7375, #33360, #4193, #17155, #41592, #22368, #38180, #25179, #12802, #33989, #28792, #9403, #12400, #17770, #21166, #8994, #37380, #27579, #30768, #5813, #38393, #9204, #2825, #8195, #34198, #1618, #31566, #2407, #25589, #35393, #42005 ),
 ( #22163, #14574, #5022, #3033, #40586, #18560, #21962, #6019, #25793, #6222, #31987, #18769, #7998, #11386, #15367, #28373, #18983, #24372, #41380, #15784, #20966, #12186, #34992, #31778, #2619, #15579, #19192, #41804, #35193, #12602, #38596, #28584, #32199, #25390, #15988, #28989, #4816, #33256, #17046, #10028, #16838, #6425, #10451, #22998, #255, #3235, #36029 ),
 ( #3658, #22578, #39646, #16194, #39432, #32614, #19398, #20026, #7270, #13008, #29631, #6841, #3446, #29415, #39220, #42, #32403, #13231, #26001, #19812, #39011, #32829, #35821, #36450, #26639, #16624, #29199, #30046, #29838, #23422, #469, #678, #20232, #9820, #22786, #26214, #4087, #6635, #19602, #886, #16409, #35609, #13441, #13857, #26428, #38798, #10237 ),
 ( #23206, #9610, #36241, #7061, #33044, #3875, #13647, #11286, #1517, #4923, #14473, #4296, #34305, #17261, #20861, #31089, #10658, #30669, #30881, #4502, #40072, #14263, #11488, #33886, #23855, #27273, #24273, #1927, #24475, #8096, #37078, #26854, #33469, #10868, #33680, #37277, #30252, #36875, #21070, #39861, #1093, #7691, #17465, #20651, #40288, #37479, #34095 ),
 ( #27483, #30461, #8305, #11080, #1305, #40694, #23638, #21275, #5134, #24066, #17878, #36660, #18085, #7898, #4714, #14061, #17669, #7482, #20441, #40492, #27065, #27685, #1722, #14679, #8726, #24689, #38331, #25535, #31292, #5758, #12127, #21688, #5542, #15310, #18290, #37697, #18500, #2136, #25116, #15097, #28315, #11916, #12545, #2769, #41324, #8519, #35337 ),
 ( #38119, #5963, #15725, #28098, #21477, #31504, #22313, #41110, #24905, #38536, #34510, #40898, #34712, #28730, #37905, #14888, #2564, #2352, #8934, #21902, #9351, #34931, #6166, #32139, #5336, #35135, #41533, #31720, #18921, #15524, #18710, #19135, #28526, #12339, #27891, #11702, #25328, #31932, #9150, #22107, #41742, #29787, #9969, #29139, #26161, #26371, #35759 ),
 ( #12750, #32776, #9764, #3386, #16353, #12952, #29360, #3606, #6575, #26585, #19338, #22942, #10181, #7220, #13173, #9551, #13383, #39163, #35553, #16569, #36403, #35970, #626, #19543, #32553, #15935, #6786, #16785, #197, #19753, #20182, #28931, #23150, #3822, #29580, #25736, #16138, #414, #32345, #22523, #38744, #39379, #36188, #7008, #19976, #3173, #42156 ),
 ( #41949, #32993, #39595, #13597, #10399, #25943, #23370, #2970, #6368, #22729, #38954, #37227, #37429, #37030, #29991, #16992, #14628, #1257, #33411, #4243, #33626, #4455, #27220, #7846, #40642, #20386, #8046, #8250, #27013, #24010, #14212, #1461, #11436, #30202, #40234, #831, #20807, #33833, #24424, #26803, #11029, #21019, #30826, #27631, #1673, #34042, #39812 ),
 ( #33206, #4870, #10605, #14421, #17828, #4661, #14007, #4031, #13806, #17205, #23585, #36609, #17617, #7428, #11233, #1043, #30619, #40022, #10816, #36818, #24217, #23799, #7637, #20596, #17412, #30408, #27428, #40440, #25495, #34878, #2301, #31034, #8885, #28049, #21427, #8472, #1875, #2084, #18034, #12291, #2723, #15261, #18452, #34456, #12077, #31457, #18878 ),
 ( #25278, #38493, #25065, #14837, #5082, #15681, #28265, #5288, #18238, #21637, #34663, #41272, #38068, #28684, #31240, #38283, #21222, #15047, #21849, #5710, #31674, #41693, #41058, #18667, #27842, #2514, #15478, #12503, #40849, #28479, #9102, #31887, #34252, #11651, #22067, #24636, #37647, #41484, #11868, #35094, #24858, #5916, #37854, #8677, #5491, #19934, #6125 ),
 ( #28894, #16738, #41909, #3348, #13554, #35297, #13130, #13340, #29101, #22480, #38911, #36147, #16314, #35508, #32517, #32735, #42120, #372, #6328, #9930, #19090, #19298, #3779, #32094, #32304, #9723, #6747, #26544, #6962, #3566, #19506, #9311, #15890, #3135, #16095, #19715, #12709, #12913, #16527, #22273, #25698, #25906, #22689, #35722, #6531, #32950, #29536 ),
 ( #2928, #26327, #10141, #26120, #38704, #29318, #160, #9511, #39124, #22898, #35935, #39333, #23111, #29742, #582, #23961, #33160, #1207, #33787, #17368, #23536, #17570, #23326, #26758, #7177, #14368, #30358, #4614, #40183, #786, #20548, #16948, #3989, #33363, #10978, #11183, #36980, #40389, #36562, #7800, #30572, #27379, #39551, #14165, #10769, #20138, #4411 ),
 ( #7378, #999, #27172, #4196, #1412, #13761, #7587, #20762, #10354, #23749, #29946, #36362, #39768, #30158, #10563, #20339, #17158, #13963, #26966, #39976, #33578, #36769, #1380, #34374, #30542, #17957, #14551, #34586, #34171, #11364, #21558, #33756, #2221, #28184, #21142, #27970, #17541, #5415, #4999, #24350, #14338, #30957, #41189, #27348, #14760, #4582, #8594 ),
 ( #1594, #40361, #31165, #18370, #24141, #40771, #1797, #27559, #40566, #8175, #11156, #37149, #37356, #7971, #27761, #20940, #11569, #4793, #31377, #37770, #24555, #33965, #11992, #40980, #15181, #37559, #11782, #24987, #17744, #30744, #8385, #7769, #21349, #5207, #20732, #18162, #2006, #14968, #24772, #5839, #37987, #25614, #12211, #25417, #21985, #19006, #19217 ),
 ( #35018, #38624, #5629, #9022, #32431, #18587, #18792, #38418, #35421, #70, #22605, #32227, #6044, #13039, #2432, #31805, #2642, #6248, #41404, #15602, #3059, #8811, #25201, #28607, #41615, #12425, #9230, #35637, #31596, #22397, #15393, #32010, #22188, #6451, #35218, #2849, #9637, #21770, #3262, #16222, #15809, #16016, #28399, #19425, #28817, #41832, #38205 ),
 ( #12626, #9427, #34796, #38827, #29015, #42035, #12830, #25818, #29228, #37256, #283, #16866, #23236, #32857, #16650, #26458, #29444, #6664, #29657, #13256, #36271, #26240, #39462, #23027, #24248, #14448, #10264, #19627, #4900, #4690, #27458, #7091, #17646, #40471, #39248, #32642, #497, #34073, #10056, #36057, #8074, #3476, #9845, #3689, #11262, #6871, #26029 ),
 ( #17855, #30648, #16437, #36476, #21048, #39676, #19843, #30856, #22812, #13469, #20053, #1701, #10479, #39038, #1491, #33072, #706, #3903, #29866, #13677, #35850, #26668, #23448, #7296, #20837, #33861, #35117, #41300, #41511, #34905, #1903, #31483, #18062, #21251, #18267, #5737, #31913, #31700, #18903, #37674, #2542, #28503, #5944, #14656, #28293, #37881, #24453 ),
 ( #15076, #24665, #28076, #15288, #5316, #38308, #31065, #34691, #21879, #27660, #24884, #34281, #25093, #8704, #5110, #2328, #40671, #21667, #12317, #31270, #2112, #11463, #5520, #25305, #8913, #18478, #12104, #38098, #18690, #15503, #9129, #37457, #27869, #41087, #14866, #40877, #8281, #11895, #22090, #11678, #8497, #21454, #34484, #12525, #25720, #41719, #35956 ),
 ( #42144, #2951, #35744, #12938, #397, #22504, #2750, #6770, #6988, #6556, #25516, #28710, #26353, #25928, #15915, #28915, #3157, #16121, #38936, #19531, #10164, #32121, #19736, #19957, #38727, #32538, #9747, #13153, #23132, #41930, #22716, #38516, #3371, #16337, #36170, #9333, #29342, #32757, #13364, #39359, #15705, #3591, #22296, #35321, #184, #6148, #16552 ),
 ( #29561, #26146, #9535, #19114, #12731, #35534, #6353, #19324, #32328, #29124, #39148, #9952, #22925, #23778, #30184, #30602, #10588, #32976, #37008, #37209, #36799, #29770, #16763, #14400, #1025, #33187, #4015, #33390, #4224, #26994, #7617, #40418, #20162, #7827, #8029, #26783, #20578, #13989, #1238, #11214, #29971, #40005, #606, #33604, #4437, #24198, #26568 ),
 ( #39794, #20789, #811, #3801, #17395, #7204, #20368, #10796, #27408, #23566, #13580, #39575, #10381, #11010, #30387, #14194, #23989, #27199, #23350, #36388, #16972, #40212, #13787, #36588, #33814, #4641, #7406, #17185, #17598, #1440, #28027, #5059, #2063, #2279, #11628, #12054, #18015, #21615, #30803, #34230, #15456, #1652, #31012, #21404, #18429, #25259, #5689 ),
 ( #38264, #31219, #27612, #31437, #15027, #11420, #8655, #12270, #41037, #18646, #24615, #37623, #34025, #11846, #34857, #15243, #24833, #37828, #28244, #41248, #21828, #34642, #14607, #1855, #34432, #8231, #40622, #24406, #18218, #5470, #25043, #38046, #21204, #14818, #37412, #31653, #5266, #8446, #27820, #8866, #41463, #40829, #2493, #4850, #28457, #21000, #17806 ),
 ( #32495, #19693, #25477, #42099, #6307, #15871, #41890, #9491, #12483, #31862, #12688, #38473, #19279, #9291, #22456, #6103, #6725, #39102, #35485, #2702, #29512, #29294, #9905, #32287, #137, #22877, #22252, #15659, #25678, #16505, #35278, #19066, #32710, #28663, #35075, #28877, #35915, #32072, #9081, #38889, #2908, #38685, #3116, #3544, #16076, #351, #26304 ),
 ( #35700, #25882, #13104, #9701, #41675, #13318, #29080, #12894, #22046, #5896, #22667, #26096, #6511, #19486, #3323, #18858, #16290, #23302, #20316, #20527, #29927, #30335, #36339, #39952, #6939, #10332, #33766, #19910, #7155, #39743, #36746, #1390, #23940, #33557, #7357, #14346, #3756, #20114, #3966, #7567, #559, #33136, #4389, #39313, #13534, #16927, #765 ),
 ( #36957, #32925, #23727, #16714, #33343, #13741, #7778, #23511, #26735, #10953, #23091, #4591, #17550, #10542, #17347, #29717, #1182, #20741, #10746, #36538, #30551, #36125, #4173, #26522, #10120, #14145, #39528, #27148, #17135, #13943, #30137, #976, #26941, #40160, #2443, #2231, #31605, #8183, #15191, #41200, #18597, #27357, #40988, #8395, #37158, #14978, #34181 ),
 ( #27770, #27980, #17967, #8820, #1603, #5217, #34595, #40369, #37568, #33973, #37780, #21357, #17752, #11791, #11164, #34383, #12004, #30966, #1807, #24149, #18171, #24996, #21567, #31174, #2015, #24782, #5424, #28194, #8605, #7980, #40575, #40781, #14559, #4801, #20949, #24564, #18379, #31388, #37996, #27566, #11372, #30752, #21151, #24359, #21779, #34805, #5639 ),
 ( #37364, #5007, #14768, #11579, #6256, #12637, #22199, #6054, #15819, #18803, #38214, #19015, #31814, #25624, #15610, #28827, #12433, #13047, #3272, #41841, #9031, #35860, #35647, #16233, #38634, #6461, #29237, #28615, #21996, #32020, #22823, #41625, #2651, #26038, #35028, #41414, #35228, #80, #25426, #15404, #3068, #38427, #2858, #9438, #9853, #25210, #9241 ),
 ( #39047, #22406, #35431, #19226, #32236, #16026, #6673, #29026, #28408, #19435, #19638, #42045, #12220, #5848, #32653, #12841, #25827, #38836, #9646, #22613, #32441, #20265, #10900, #32867, #7515, #20692, #39471, #36485, #13687, #13895, #23890, #507, #26679, #29453, #33293, #7306, #36908, #39259, #39686, #33503, #1128, #27096, #14097, #20476, #10065, #26249, #4122 ),
 ( #23036, #26887, #30287, #17082, #26467, #40106, #292, #16659, #36068, #7725, #30083, #3488, #23673, #3699, #921, #6883, #19853, #7100, #36692, #16447, #4332, #13265, #10275, #17297, #29666, #13480, #23246, #39896, #10488, #36279, #10693, #20061, #3913, #33082, #16875, #29876, #714, #23458, #7931, #11530, #40937, #37947, #1759, #40322, #1966, #14719, #24103 ),
 ( #27721, #18332, #37315, #24310, #4538, #24511, #5377, #27930, #40730, #8343, #31129, #11745, #34552, #37518, #1339, #4751, #34129, #20900, #11114, #14296, #30921, #21311, #34341, #24732, #33921, #17704, #37735, #18124, #5170, #8559, #14930, #37111, #41149, #30703, #21519, #8772, #17499, #31335, #2179, #11321, #1553, #21105, #15138, #28141, #14508, #11955, #24946 ),
 ( #33716, #27307, #27522, #30497, #40529, #8131, #4956, #17915, #25989, #6412, #3018, #31973, #38998, #28357, #5797, #28568, #32185, #25164, #31762, #15975, #21732, #38164, #18753, #41576, #2605, #35177, #19384, #15352, #6208, #2393, #2810, #12385, #32388, #6004, #25372, #35595, #5588, #16181, #31, #18966, #41991, #31547, #3219, #15771, #38376, #41365, #28776 ),
 ( #41786, #18544, #22566, #12168, #22354, #15564, #8978, #28972, #29184, #21945, #12586, #25575, #9190, #22146, #38579, #34974, #9391, #35379, #19179, #12788, #25778, #38786, #9596, #12995, #34754, #10223, #32598, #30239, #30031, #10645, #20014, #872, #39850, #22987, #16396, #26415, #17246, #10014, #26202, #7467, #29402, #35806, #16612, #23626, #19797, #9807, #39633 ),
 ( #3861, #4282, #29620, #1079, #27052, #242, #33033, #26625, #7258, #13844, #36645, #13634, #19588, #36014, #23192, #39206, #13219, #3431, #7048, #10438, #23409, #4073, #6828, #32817, #3647, #455, #6620, #26842, #33454, #16825, #29827, #13427, #666, #36440, #20427, #39419, #22775, #14048, #36226, #20218, #33244, #17033, #21464, #8084, #40273, #11068, #40480 ),
 ( #14666, #5325, #27258, #1914, #15085, #33872, #30865, #21057, #8291, #18278, #37067, #34083, #23839, #27670, #1711, #31279, #33666, #4910, #27878, #37684, #34494, #8506, #14876, #4490, #20636, #40681, #2123, #40887, #17449, #21261, #24675, #11473, #20847, #40059, #36860, #24052, #30448, #10852, #24462, #7677, #18073, #7885, #37467, #1293, #14250, #1502, #31074 ),
 ( #4702, #17656, #11689, #30657, #14458, #27470, #34291, #17865, #11274, #5120, #24257, #37265, #38107, #28514, #29301, #18699, #10125, #2338, #5952, #35921, #32931, #38320, #34701, #39108, #9139, #18487, #16299, #19916, #22098, #13323, #31710, #2551, #41097, #18912, #357, #22883, #25315, #34917, #15512, #41521, #31493, #8715, #12327, #15297, #35126, #28303, #32501 ),
 ( #41309, #32718, #3761, #21888, #3330, #145, #9913, #6948, #25104, #13111, #11904, #26103, #6731, #28086, #21677, #19699, #16511, #26311, #23097, #39319, #3552, #5530, #12114, #29517, #24893, #36130, #8923, #37890, #5747, #30341, #39752, #27363, #13539, #29932, #39533, #37162, #1189, #1395, #36964, #3972, #33563, #20119, #23310, #20322, #7785, #33976, #33771 ),
 ( #4598, #30556, #7984, #20954, #14150, #39959, #26528, #4396, #23517, #17142, #26742, #30144, #17352, #7364, #40374, #33144, #36753, #23946, #16720, #26946, #36345, #27153, #10751, #7160, #40167, #29723, #23733, #14351, #33349, #4178, #565, #7572, #11169, #10959, #20533, #20746, #17554, #24153, #10339, #16933, #770, #13747, #983, #10548, #36545, #13949, #2018 ),
 ( #41203, #5012, #34185, #14564, #27773, #1607, #38001, #28412, #40992, #14982, #17971, #37783, #27984, #2447, #24567, #4805, #30757, #41417, #25215, #18175, #25000, #27569, #18602, #31177, #8399, #11375, #11796, #38218, #40578, #24785, #24362, #5643, #37368, #5427, #40784, #8186, #28198, #15407, #21155, #8608, #21572, #11584, #37573, #5221, #30970, #1810, #21360 ),
 ( #14773, #34598, #34386, #12224, #34809, #18383, #31391, #9036, #8823, #31608, #2236, #21783, #22000, #15195, #12007, #17756, #298, #35233, #9245, #32659, #12437, #18807, #41845, #22828, #2863, #35032, #22619, #22202, #22410, #29031, #29459, #12641, #26254, #10070, #25430, #13052, #19440, #9651, #26043, #35653, #38430, #13270, #6058, #42052, #39264, #31817, #38842 ),
 ( #19018, #35437, #19644, #12847, #32025, #16031, #16239, #25629, #39053, #15824, #6466, #2655, #28832, #5851, #15613, #38639, #6261, #32446, #28618, #3494, #29242, #3073, #41629, #9444, #19232, #32242, #3278, #25833, #87, #9858, #35865, #6678, #16453, #719, #33087, #36490, #20696, #16664, #7519, #3705, #33299, #29881, #7730, #7310, #26684, #36912, #14102 ),
 ( #36286, #17504, #29671, #20066, #23464, #20481, #27312, #33720, #4340, #4127, #40326, #512, #7107, #13694, #33507, #26473, #3918, #17301, #23042, #39477, #16880, #39694, #10494, #20270, #4545, #13486, #30292, #10281, #17087, #30089, #30502, #928, #13901, #1344, #6890, #14300, #36073, #26891, #1134, #32874, #19858, #39903, #10698, #23252, #23678, #36698, #27101 ),
 ( #23895, #40112, #10905, #4961, #20906, #34556, #21737, #27527, #1970, #8347, #17921, #1764, #11535, #14516, #33927, #14724, #40533, #21317, #11327, #24517, #8137, #8777, #41154, #37523, #4758, #31554, #31341, #11960, #34345, #2186, #24952, #24314, #17709, #27725, #18550, #37321, #21110, #34760, #30708, #37115, #30926, #37953, #34135, #11120, #40943, #40734, #5175 ),
 ( #18128, #2398, #28363, #1558, #15144, #37740, #27936, #28147, #11749, #31133, #15357, #14934, #24737, #24108, #7935, #8563, #5594, #21524, #5381, #18337, #25994, #6214, #25377, #22359, #22571, #31978, #8983, #22152, #38170, #32393, #22780, #35384, #38586, #41582, #32190, #9395, #39003, #18971, #41370, #3226, #3437, #3024, #21951, #25170, #35811, #19185, #12390 ),
 ( #41793, #15980, #28978, #6627, #28574, #16186, #16402, #35183, #41997, #12794, #9602, #19594, #38383, #25783, #34981, #38791, #35601, #32604, #5803, #6418, #29190, #9814, #12174, #18758, #36, #31768, #2610, #19389, #15569, #13001, #9195, #6009, #2817, #15776, #28781, #12592, #25580, #461, #10020, #7683, #13849, #14054, #7474, #16618, #4080, #32822, #36019 ),
 ( #4496, #4288, #33673, #10229, #17253, #1087, #20642, #29407, #878, #10444, #39212, #17038, #36232, #29833, #39423, #671, #30037, #20020, #10858, #3651, #7263, #36652, #247, #39638, #6833, #39855, #23415, #19804, #26848, #13225, #36445, #27058, #33038, #3866, #26208, #20223, #40066, #23632, #33250, #10651, #20433, #33461, #30245, #23847, #22992, #13434, #13639 ),
 ( #36868, #29625, #26420, #26632, #16831, #23198, #7053, #24264, #2128, #1716, #21062, #31285, #1299, #11909, #37897, #30872, #37690, #27264, #15091, #14672, #34088, #24057, #27676, #8719, #40281, #24469, #14255, #18283, #37072, #18078, #11279, #11073, #40892, #28092, #33880, #8299, #40688, #37270, #8090, #17871, #20852, #7891, #4917, #4708, #11480, #17661, #37472 ),
 ( #5329, #21268, #30662, #21681, #8512, #41103, #34297, #21471, #24898, #1510, #14464, #5127, #34705, #27476, #40485, #17457, #31081, #1920, #14882, #30455, #27884, #11696, #24682, #34501, #25319, #5956, #38736, #15517, #35545, #6361, #12120, #6157, #25526, #28722, #35330, #41732, #25109, #9544, #38113, #18915, #5535, #31497, #12538, #32131, #28519, #5751, #38325 ),
 ( #18703, #31925, #19125, #41526, #2963, #31714, #38527, #15302, #34924, #22514, #28308, #2556, #9143, #9343, #18493, #25729, #15925, #2762, #2345, #12332, #22100, #35129, #28923, #15717, #22306, #41941, #41315, #12741, #8927, #21895, #11408, #14806, #41238, #37196, #28016, #24186, #11617, #24604, #8017, #11834, #37609, #34010, #31208, #34846, #8435, #28232, #5047 ),
 ( #34420, #15233, #37816, #21393, #18207, #41026, #21604, #2269, #5253, #11200, #14594, #1842, #30790, #20988, #4839, #40816, #2051, #15016, #8643, #1640, #27599, #17793, #24395, #40406, #34632, #25032, #24821, #5459, #40609, #18419, #31427, #12043, #21191, #1429, #38035, #5679, #8855, #37400, #27395, #21819, #18637, #8218, #34218, #27808, #14388, #18002, #31000 ),
 ( #35689, #6713, #25467, #22444, #41878, #42088, #9893, #28653, #12677, #15444, #6297, #35473, #22866, #25250, #25667, #19476, #29283, #13092, #127, #6498, #38254, #12257, #19268, #35904, #32484, #9071, #12883, #16278, #3105, #12473, #26084, #28447, #2691, #22036, #31642, #16066, #39091, #9689, #18848, #32275, #35064, #5886, #35267, #22656, #2482, #3312, #41452 ),
 ( #31852, #15648, #29069, #38674, #41665, #25871, #38463, #32059, #9281, #2898, #38877, #22241, #6091, #19054, #9480, #15860, #28866, #1172, #29916, #19898, #32913, #20101, #33125, #13730, #36527, #27137, #6927, #23716, #36948, #13522, #10531, #755, #30126, #40150, #16701, #26724, #3534, #7347, #23500, #10943, #13305, #39732, #7557, #17336, #14135, #30327, #36734 ) ),
 .UNSPECIFIED., .F., .F., .F.,
 ( 4, 1, 1, 1, 1, 1, 1, 1, 1, 1, 1, 1, 1, 1, 1, 1, 1, 1, 1, 1, 1, 1, 1, 1, 1, 1, 1, 1, 1, 1, 1, 1, 1, 1, 1, 1, 1, 1, 1, 1, 1, 1, 1, 1, 1, 1, 3, 4 ),
 ( 4, 1, 1, 1, 1, 1, 1, 1, 1, 1, 1, 1, 2, 1, 1, 1, 2, 1, 1, 1, 1, 1, 2, 1, 1, 1, 1, 1, 1, 1, 2, 1, 1, 1, 1, 1, 1, 1, 1, 1, 4 ),
 ( 0.000000000000000000, 0.007812500000000000000, 0.01562500000000000000, 0.02343750000000000000, 0.03125000000000000000, 0.04687500000000000000, 0.06250000000000000000, 0.07812500000000000000, 0.09375000000000000000, 0.1093750000000000000, 0.1250000000000000000, 0.1406250000000000000, 0.1562500000000000000, 0.1875000000000000000, 0.2187500000000000000, 0.2500000000000000000, 0.2812500000000000000, 0.3125000000000000000, 0.3281250000000000000, 0.3437500000000000000, 0.3750000000000000000, 0.4062500000000000000, 0.4375000000000000000, 0.4687500000000000000, 0.5000000000000000000, 0.5312500000000000000, 0.5625000000000000000, 0.5937500000000000000, 0.6250000000000000000, 0.6562500000000000000, 0.6718750000000000000, 0.6875000000000000000, 0.7187500000000000000, 0.7500000000000000000, 0.7812500000000000000, 0.8125000000000000000, 0.8437500000000000000, 0.8750000000000000000, 0.8906250000000000000, 0.9062500000000000000, 0.9218750000000000000, 0.9375000000000000000, 0.9531250000000000000, 0.9687500000000000000, 0.9765625000000000000, 0.9843750000000000000, 1.000000000000000000, 1.020392624918932789 ),
 ( 0.000000000000000000, 0.01539374999999999945, 0.03078749999999999890, 0.04618125000000002089, 0.06157499999999999779, 0.07696875000000003020, 0.09236250000000004179, 0.1077562499999999979, 0.1231499999999999956, 0.1431375000000000008, 0.1631250000000000200, 0.1831125000000000114, 0.2031000000000000028, 0.2063375000000000070, 0.2095750000000000113, 0.2128125000000000155, 0.2160500000000000198, 0.2667375000000000163, 0.3174250000000000682, 0.3681125000000000647, 0.4188000000000000611, 0.5201750000000000540, 0.6215500000000000469, 0.6266374999999999584, 0.6317250000000000920, 0.6368124999999997815, 0.6418999999999999151, 0.6469874999999999376, 0.6520749999999999602, 0.6571624999999999828, 0.6622500000000000053, 0.7044687500000000879, 0.7466875000000001705, 0.7889062500000000311, 0.8010555555555555207, 0.8311249999999998916, 0.8733437499999998632, 0.9155625000000000568, 0.9403166666666666895, 0.9577812500000000284, 1.000000000000000000 ),
 .UNSPECIFIED. ) ;
#3486 = CARTESIAN_POINT ( 'NONE',  ( -10.40651172546669301, 123.5464890276372785, 0.9122707376378308419 ) ) ;
#3487 = DIRECTION ( 'NONE',  ( -4.017660918040594346E-17, 1.000000000000000000, 2.376309959284834438E-19 ) ) ;
#3488 = CARTESIAN_POINT ( 'NONE',  ( 9.425666535144223701, 121.4347015428822374, -1.122958709584367831 ) ) ;
#3489 = AXIS2_PLACEMENT_3D ( 'NONE', #21685, #5132, #18708 ) ;
#3490 = CARTESIAN_POINT ( 'NONE',  ( -20.78747236883577543, 145.7124547906547889, -2.408930808681182256 ) ) ;
#3491 = CARTESIAN_POINT ( 'NONE',  ( -58.50860430493789721, 0.7049166599848305514, -0.9756837515128595761 ) ) ;
#3492 = ORIENTED_EDGE ( 'NONE', *, *, #14908, .F. ) ;
#3493 = CARTESIAN_POINT ( 'NONE',  ( 4.527352789474797135, 118.1161674766824206, -0.5309711699598146373 ) ) ;
#3494 = CARTESIAN_POINT ( 'NONE',  ( 10.17757484390027756, 124.8647468421599598, -0.4356504197092352926 ) ) ;
#3495 = ORIENTED_EDGE ( 'NONE', *, *, #4575, .T. ) ;
#3496 = CARTESIAN_POINT ( 'NONE',  ( -10.71652553037534794, 154.3566586077636487, -1.965850361453045814 ) ) ;
#3497 = CARTESIAN_POINT ( 'NONE',  ( 3.057239904206551895, -15.51127639645041789, 4.278020201805971645 ) ) ;
#3498 = DIRECTION ( 'NONE',  ( -5.206863593109713661E-17, 1.000000000000000000, -1.077750396879097183E-30 ) ) ;
#3499 = FACE_OUTER_BOUND ( 'NONE', #20995, .T. ) ;
#3500 = ADVANCED_FACE ( 'NONE', ( #32420 ), #32214, .T. ) ;
#3501 = CARTESIAN_POINT ( 'NONE',  ( -4.942855899094846350, 117.6285334314414399, 0.7732941537803618148 ) ) ;
#3502 = CARTESIAN_POINT ( 'NONE',  ( 6.550279792842248483, 120.6599796251122427, 1.081144621291421304 ) ) ;
#3503 = CARTESIAN_POINT ( 'NONE',  ( -2.667392527469404140, 31.33771804890096746, 0.9893360403373157030 ) ) ;
#3504 = AXIS2_PLACEMENT_3D ( 'NONE', #14295, #27306, #40321 ) ;
#3505 = CARTESIAN_POINT ( 'NONE',  ( 3.400481176189167343, 25.78150505744974552, 3.158589348000393482 ) ) ;
#3506 = CARTESIAN_POINT ( 'NONE',  ( 8.827910802434928428, 123.6950213215744583, 0.2595790122280457468 ) ) ;
#3507 = DIRECTION ( 'NONE',  ( -0.7770581983690836303, 0.6294287539884032556, -5.101669463485833779E-16 ) ) ;
#3509 = ORIENTED_EDGE ( 'NONE', *, *, #4350, .T. ) ;
#3508 = CARTESIAN_POINT ( 'NONE',  ( -46.62078961162516322, 17.34433182989875277, -0.7188397291161608971 ) ) ;
#3510 = CARTESIAN_POINT ( 'NONE',  ( 7.017589760824501255, 78.79342665089201603, 2.556811674275345059 ) ) ;
#3511 = CARTESIAN_POINT ( 'NONE',  ( 3.302029177305205732, 159.4671159221996959, 0.06598240135525389183 ) ) ;
#3512 = CIRCLE ( 'NONE', #16406, 5.080000000000006288 ) ;
#3513 = DIRECTION ( 'NONE',  ( 0.000000000000000000, 0.000000000000000000, -1.000000000000000000 ) ) ;
#3514 = CARTESIAN_POINT ( 'NONE',  ( -8.438946883131665189, 119.3197881592811029, -1.362662033712001453 ) ) ;
#3515 = CARTESIAN_POINT ( 'NONE',  ( -5.965356522962950159, 88.73331249999998249, 5.016499999999999737 ) ) ;
#3516 = CARTESIAN_POINT ( 'NONE',  ( -4.074955089416341991, 118.2429491485453354, 0.1454234154749719787 ) ) ;
#3517 = CARTESIAN_POINT ( 'NONE',  ( -23.14542444889682216, 82.37908244650444090, 1.269999999999993578 ) ) ;
#3518 = CARTESIAN_POINT ( 'NONE',  ( -57.71825614945207406, 2.868614883688350048, 0.7691332274306142969 ) ) ;
#3519 = CARTESIAN_POINT ( 'NONE',  ( -57.71946847630993460, 1.146847591362354368, 1.351507486235933975 ) ) ;
#3520 = CARTESIAN_POINT ( 'NONE',  ( -13.57554913733971347, 119.6371495169912436, -0.05144635950012913655 ) ) ;
#3521 = ORIENTED_EDGE ( 'NONE', *, *, #15903, .T. ) ;
#3522 = CARTESIAN_POINT ( 'NONE',  ( -53.89938688035451975, 11.68864614896874343, -3.017114338529875095 ) ) ;
#3523 = CARTESIAN_POINT ( 'NONE',  ( 6.979485140712072599, 121.9514898806366006, 0.06293811663084028507 ) ) ;
#3524 = ADVANCED_FACE ( 'NONE', ( #23015, #6652 ), #38610, .F. ) ;
#3525 = ORIENTED_EDGE ( 'NONE', *, *, #6317, .T. ) ;
#3526 = CARTESIAN_POINT ( 'NONE',  ( 4.357800360384668004, 115.7036734823842323, -1.373096195996742264 ) ) ;
#3527 = CARTESIAN_POINT ( 'NONE',  ( -1.611903344789388903, 120.9971453638330985, -0.05790686387416373038 ) ) ;
#3528 = CARTESIAN_POINT ( 'NONE',  ( 6.098373624802439608, -13.52034412102339012, 1.767782016118699895 ) ) ;
#3529 = VECTOR ( 'NONE', #29481, 1000.000000000000000 ) ;
#3530 = CARTESIAN_POINT ( 'NONE',  ( -21.28061085028127764, 148.8133262010608462, 1.460188425234498100 ) ) ;
#3531 = LINE ( 'NONE', #32057, #31548 ) ;
#3532 = CARTESIAN_POINT ( 'NONE',  ( -0.003073183581815366015, 116.5806198863164838, 0.1537946732117061177 ) ) ;
#3533 = EDGE_CURVE ( 'NONE', #12640, #35416, #15741, .T. ) ;
#3534 = CARTESIAN_POINT ( 'NONE',  ( 13.58627218224582656, 150.2694722113990338, 0.4661934924574481776 ) ) ;
#3535 = CARTESIAN_POINT ( 'NONE',  ( 4.965622106538171820, 115.6909491485453145, -1.258976657945148458 ) ) ;
#3536 = CARTESIAN_POINT ( 'NONE',  ( 0.7743132463278736832, -9.628960163071635492, -0.5975928149734356376 ) ) ;
#3537 = CARTESIAN_POINT ( 'NONE',  ( -23.32994265436209602, 149.0590277239482475, -0.6203886826157011258 ) ) ;
#3538 = CARTESIAN_POINT ( 'NONE',  ( 5.965356522962859565, 57.14999999999999858, -5.016499999999999737 ) ) ;
#3539 = CARTESIAN_POINT ( 'NONE',  ( -8.727017694313293106, 118.0966776702152004, 0.5009128790051901037 ) ) ;
#3540 = VERTEX_POINT ( 'NONE', #32629 ) ;
#3541 = CARTESIAN_POINT ( 'NONE',  ( -11.64084037886373224, 123.0696236843973281, 1.242201319703144291 ) ) ;
#3542 = CARTESIAN_POINT ( 'NONE',  ( -58.36955422849574404, -0.2910357702952456882, -0.02058977239408909393 ) ) ;
#3543 = CARTESIAN_POINT ( 'NONE',  ( 7.913941031674588622, 118.5968412048868288, 1.173277403367298577 ) ) ;
#3544 = CARTESIAN_POINT ( 'NONE',  ( 4.562247774926673216, 157.9011380394538833, -1.652341844578318231 ) ) ;
#3545 = CARTESIAN_POINT ( 'NONE',  ( -0.9635192623308774795, 7.475506455475952272, -0.1398073520734665620 ) ) ;
#3546 = VECTOR ( 'NONE', #22113, 1000.000000000000114 ) ;
#3547 = CARTESIAN_POINT ( 'NONE',  ( -21.70872022418687308, 149.0176745010074342, -2.143008773150906432 ) ) ;
#3548 = CARTESIAN_POINT ( 'NONE',  ( 4.846611013106016941, 117.8246425087505713, -0.6900207181998705419 ) ) ;
#3549 = AXIS2_PLACEMENT_3D ( 'NONE', #20288, #32680, #42071 ) ;
#3550 = CARTESIAN_POINT ( 'NONE',  ( -23.91048590848665967, 81.84235438443283783, 1.269999999999993801 ) ) ;
#3551 = AXIS2_PLACEMENT_3D ( 'NONE', #28708, #40875, #5108 ) ;
#3552 = CARTESIAN_POINT ( 'NONE',  ( 11.70197428064578737, 126.1299551460304542, -0.9179571146301047646 ) ) ;
#3553 = CARTESIAN_POINT ( 'NONE',  ( -5.966562942538025993, 155.3820107761045790, -0.07923228615413194231 ) ) ;
#3554 = ORIENTED_EDGE ( 'NONE', *, *, #35530, .T. ) ;
#3555 = CARTESIAN_POINT ( 'NONE',  ( 0.03153862713803012863, 157.4657262375360176, -1.578321868909182246 ) ) ;
#3556 = CARTESIAN_POINT ( 'NONE',  ( 2.279390105945505507, -15.60765617898064761, 5.834426787525912594 ) ) ;
#3557 = DIRECTION ( 'NONE',  ( 0.000000000000000000, -1.000000000000000000, 0.000000000000000000 ) ) ;
#3558 = CARTESIAN_POINT ( 'NONE',  ( -48.65005484009959957, 18.46594748123760965, -5.297328305960443018 ) ) ;
#3559 = ORIENTED_EDGE ( 'NONE', *, *, #27736, .F. ) ;
#3560 = CARTESIAN_POINT ( 'NONE',  ( 18.35242356974463718, 147.0160646422468744, 2.398428600884452866 ) ) ;
#3561 = CARTESIAN_POINT ( 'NONE',  ( -15.77133435453296606, 146.5691041611200660, -0.3151487940933135334 ) ) ;
#3562 = LINE ( 'NONE', #156, #2846 ) ;
#3563 = CARTESIAN_POINT ( 'NONE',  ( -3.258544586981842794, 118.6786177306206014, 0.6136036933997359721 ) ) ;
#3564 = CARTESIAN_POINT ( 'NONE',  ( 8.062851560922409178, 27.27981867468588462, -2.430221966868060690 ) ) ;
#3565 = CARTESIAN_POINT ( 'NONE',  ( 15.96902210417518475, 146.0164801329953548, 1.048924711619907191 ) ) ;
#3566 = CARTESIAN_POINT ( 'NONE',  ( 22.74464968533188269, 149.4207734315791072, -0.6238039466385614240 ) ) ;
#3567 = CARTESIAN_POINT ( 'NONE',  ( 4.610436209567292387, 117.9340757871244847, 0.9619774773656434297 ) ) ;
#3568 = DIRECTION ( 'NONE',  ( 0.6294287539883864913, 0.7770581983690970640, 0.000000000000000000 ) ) ;
#3569 = AXIS2_PLACEMENT_3D ( 'NONE', #12145, #18308, #25137 ) ;
#3570 = UNCERTAINTY_MEASURE_WITH_UNIT (LENGTH_MEASURE( 1.000000000000000082E-05 ), #19633, 'distance_accuracy_value', 'NONE');
#3571 = CARTESIAN_POINT ( 'NONE',  ( -1.806356699219227036, 116.4728921782852922, 0.003255218499346703570 ) ) ;
#3572 = EDGE_LOOP ( 'NONE', ( #40114, #32875, #2213, #32243, #14251, #31489, #20934, #6341, #3416 ) ) ;
#3573 = CARTESIAN_POINT ( 'NONE',  ( -5.594070761475127718, 120.8783406922565860, -0.6737976942813748149 ) ) ;
#3574 = CARTESIAN_POINT ( 'NONE',  ( 5.498428541007762682, -14.58429751298133326, 3.325033752563948841 ) ) ;
#3575 = CARTESIAN_POINT ( 'NONE',  ( -4.509850150708960115, 121.0527503406816123, -0.3565835012282696503 ) ) ;
#3576 = CARTESIAN_POINT ( 'NONE',  ( 3.392078256862109953, -14.39927144874259035, 5.014931565121842461 ) ) ;
#3577 = DIRECTION ( 'NONE',  ( -0.8745520943968250194, 0.4849315768086532863, -5.361993529360574930E-16 ) ) ;
#3578 = CARTESIAN_POINT ( 'NONE',  ( 16.86029543505349082, 155.2078297922403465, 0.3599557924993779801 ) ) ;
#3579 = ADVANCED_FACE ( 'NONE', ( #22593 ), #26229, .F. ) ;
#3580 = ORIENTED_EDGE ( 'NONE', *, *, #24523, .F. ) ;
#3581 = CARTESIAN_POINT ( 'NONE',  ( -1.178223178616622402, 14.53665720681882689, 4.476207649055042204 ) ) ;
#3582 = CARTESIAN_POINT ( 'NONE',  ( -15.56076557482332490, 120.7233670659379214, -0.3109411287488704767 ) ) ;
#3583 = DIRECTION ( 'NONE',  ( -0.8745520943968383420, 0.4849315768086291945, -4.268512490100416826E-16 ) ) ;
#3584 = CIRCLE ( 'NONE', #2914, 3.683000000000001162 ) ;
#3585 = CARTESIAN_POINT ( 'NONE',  ( 2.928857528687646372, 107.6124775248579937, 4.448914392086990688 ) ) ;
#3586 = CARTESIAN_POINT ( 'NONE',  ( -7.018365211845482676, 121.6248220782754146, 0.4451966353337011295 ) ) ;
#3587 = CARTESIAN_POINT ( 'NONE',  ( 0.7325351754718939512, 15.47086736126800766, -4.571311019245588803 ) ) ;
#3588 = CARTESIAN_POINT ( 'NONE',  ( 22.34249146463927715, 149.5981344557702641, 1.749037778780574426 ) ) ;
#3589 = CARTESIAN_POINT ( 'NONE',  ( -22.85582906289733529, 78.03019435252696212, 1.269999999999994245 ) ) ;
#3591 = CARTESIAN_POINT ( 'NONE',  ( 9.409928955097466741, 157.3305555497073271, -1.526371511294253303 ) ) ;
#3590 = CARTESIAN_POINT ( 'NONE',  ( -5.078986093043185157, 68.92746620154572668, -0.1014902294541231847 ) ) ;
#3592 = CARTESIAN_POINT ( 'NONE',  ( -0.5832499861179958334, 10.72304255322087307, 4.598074068532726599 ) ) ;
#3593 = CARTESIAN_POINT ( 'NONE',  ( -21.67644226493410287, 136.7703657609320658, -1.576579429902727814 ) ) ;
#3594 = ORIENTED_EDGE ( 'NONE', *, *, #6327, .T. ) ;
#3595 = CARTESIAN_POINT ( 'NONE',  ( -6.058098509843230950, 155.3491655920357459, 0.2313079102920782559 ) ) ;
#3596 = CARTESIAN_POINT ( 'NONE',  ( 4.583978111877545558, -14.49189839317011064, 4.572462404262108038 ) ) ;
#3597 = CARTESIAN_POINT ( 'NONE',  ( -30.20416046766210272, 71.17241488000101413, -1.524000000000007571 ) ) ;
#3598 = AXIS2_PLACEMENT_3D ( 'NONE', #41612, #15389, #25413 ) ;
#3599 = ORIENTED_EDGE ( 'NONE', *, *, #37027, .T. ) ;
#3600 = CARTESIAN_POINT ( 'NONE',  ( 0.4661379286530221155, 118.8635629087341954, 0.6143748731645415351 ) ) ;
#3601 = CARTESIAN_POINT ( 'NONE',  ( 3.223859242259402791, 50.63946620154572997, -1.416295642791934650 ) ) ;
#3602 = DIRECTION ( 'NONE',  ( -0.9998004120163608288, 0.000000000000000000, -0.01997839162482749342 ) ) ;
#3603 = CARTESIAN_POINT ( 'NONE',  ( -22.76023949468089214, 146.4845460041848355, 0.7370798038890575832 ) ) ;
#3604 = CARTESIAN_POINT ( 'NONE',  ( 4.144591825430580911, 15.01708852069707945, -7.363685156706923252 ) ) ;
#3605 = AXIS2_PLACEMENT_3D ( 'NONE', #20595, #33624, #40021 ) ;
#3606 = CARTESIAN_POINT ( 'NONE',  ( 5.826550815406353223, 117.0573985505404693, -0.1859578237674346934 ) ) ;
#3607 = CARTESIAN_POINT ( 'NONE',  ( -14.95453923199683643, 61.75387968257833649, 5.016499999999999737 ) ) ;
#3608 = CARTESIAN_POINT ( 'NONE',  ( -49.36011206067185242, 17.22521247008247158, 4.983413103225731611 ) ) ;
#3609 = CARTESIAN_POINT ( 'NONE',  ( -49.59145623469802899, 21.58002366008788542, 1.574391596335662058 ) ) ;
#3610 = CARTESIAN_POINT ( 'NONE',  ( 1.880425555005761362, -15.05705604436505318, 5.673589828627330967 ) ) ;
#3611 = CARTESIAN_POINT ( 'NONE',  ( -49.13940628111213016, 17.59503125033257120, 5.062072503518671773 ) ) ;
#3612 = CARTESIAN_POINT ( 'NONE',  ( -4.757346424997288103, 117.3993836135861386, -1.207075064218979810 ) ) ;
#3613 = CARTESIAN_POINT ( 'NONE',  ( -4.408801154305764136, 118.1814785907497480, 0.3997980591957170371 ) ) ;
#3614 = CARTESIAN_POINT ( 'NONE',  ( -5.594725610051334286, 78.91206791035253332, -5.077866005995125498 ) ) ;
#3615 = ORIENTED_EDGE ( 'NONE', *, *, #3047, .F. ) ;
#3616 = ORIENTED_EDGE ( 'NONE', *, *, #14158, .F. ) ;
#3617 = CARTESIAN_POINT ( 'NONE',  ( -1.984596792730465076, 115.6909491485466646, -1.718749578237781073 ) ) ;
#3618 = CARTESIAN_POINT ( 'NONE',  ( -6.126668539192166030, 119.5961181856799556, -1.251232543939694519 ) ) ;
#3619 = CARTESIAN_POINT ( 'NONE',  ( -2.472230802051619936, 107.2388417251876547, -4.724420784806152795 ) ) ;
#3620 = CARTESIAN_POINT ( 'NONE',  ( 4.495330299262407792, 118.0850605857251452, 0.7940255090980337105 ) ) ;
#3621 = CARTESIAN_POINT ( 'NONE',  ( -46.68114719912644262, 26.04180998113828238, -1.171086909392329956 ) ) ;
#3622 = CARTESIAN_POINT ( 'NONE',  ( -12.48065534322216941, 152.0704867801853766, -1.458211671286261835 ) ) ;
#3623 = AXIS2_PLACEMENT_3D ( 'NONE', #16863, #39673, #494 ) ;
#3624 = CARTESIAN_POINT ( 'NONE',  ( -3.722927991306443918, 115.7030846131066397, -1.610849859475568024 ) ) ;
#3625 = CARTESIAN_POINT ( 'NONE',  ( -0.7530120751189652850, 106.0529022055765296, 5.240410227246371733 ) ) ;
#3626 = CARTESIAN_POINT ( 'NONE',  ( 7.588858076165080568, 124.2943531750336490, 0.1426133663090956294 ) ) ;
#3627 = CARTESIAN_POINT ( 'NONE',  ( -17.23442203377900128, 146.5563353440282981, -2.056614067264090462 ) ) ;
#3628 = SURFACE_STYLE_USAGE ( .BOTH. , #6808 ) ;
#3629 = DIRECTION ( 'NONE',  ( -5.188838149069472160E-16, 1.699382548006136559E-16, 1.000000000000000000 ) ) ;
#3630 = CARTESIAN_POINT ( 'NONE',  ( 8.366466113708492358, 119.9145198431062340, -1.112176479753337333 ) ) ;
#3631 = CARTESIAN_POINT ( 'NONE',  ( -12.80217232463537336, 133.7150629370494244, -0.1325446241630061361 ) ) ;
#3632 = CARTESIAN_POINT ( 'NONE',  ( -1.504723661876595786, -8.552649586842417051, -4.374500482163298898 ) ) ;
#3633 = CARTESIAN_POINT ( 'NONE',  ( 18.33253411489121731, 154.1536317137893661, 1.165609363665846665 ) ) ;
#3634 = CARTESIAN_POINT ( 'NONE',  ( 19.68500000000000227, 71.11999999999999034, -5.016499999999999737 ) ) ;
#3635 = CARTESIAN_POINT ( 'NONE',  ( 3.347262984424072219, -14.85936863781750539, 0.1546827838429291613 ) ) ;
#3636 = CARTESIAN_POINT ( 'NONE',  ( -4.214263934994832539, 119.2415290214368042, 0.8241011934941721018 ) ) ;
#3637 = CARTESIAN_POINT ( 'NONE',  ( -0.5928395319016861453, 6.288998576159460008, -0.7801151024821093571 ) ) ;
#3638 = CARTESIAN_POINT ( 'NONE',  ( -15.04006788896557012, 156.1474796653986630, -0.8176042244810638460 ) ) ;
#3639 = VECTOR ( 'NONE', #14630, 1000.000000000000000 ) ;
#3640 = CARTESIAN_POINT ( 'NONE',  ( -0.7776641127062334791, -6.825634839940509124, -0.5883101582535473772 ) ) ;
#3641 = VERTEX_POINT ( 'NONE', #26017 ) ;
#3642 = VERTEX_POINT ( 'NONE', #39026 ) ;
#3643 = CARTESIAN_POINT ( 'NONE',  ( -45.58494389689084869, 18.10922195552001313, -6.304117962515870643E-15 ) ) ;
#3644 = CARTESIAN_POINT ( 'NONE',  ( 5.349033702192260264, 117.2069880336854197, 0.8964318704791016668 ) ) ;
#3645 = CARTESIAN_POINT ( 'NONE',  ( -7.748985956666807340, 122.1869765257964673, 0.4223483383238799682 ) ) ;
#3646 = CARTESIAN_POINT ( 'NONE',  ( 4.218352450475082449, -13.04292013931325478, 2.887648331721151873 ) ) ;
#3647 = CARTESIAN_POINT ( 'NONE',  ( 16.48900842742850870, 139.9843038322558186, -1.489460148179643673 ) ) ;
#3648 = CARTESIAN_POINT ( 'NONE',  ( -19.73710541150947506, 148.2167131080949787, -2.515028838702476399 ) ) ;
#3649 = CARTESIAN_POINT ( 'NONE',  ( 3.177488185987922709, -14.13217061847354472, 2.003775387181677026 ) ) ;
#3650 = CARTESIAN_POINT ( 'NONE',  ( -4.679832524073478162, 32.47693947602098063, 1.143146696348500413 ) ) ;
#3651 = CARTESIAN_POINT ( 'NONE',  ( 9.679874449561324923, 124.8500477395539576, 0.02572261534930073840 ) ) ;
#3652 = ORIENTED_EDGE ( 'NONE', *, *, #11204, .F. ) ;
#3653 = DIRECTION ( 'NONE',  ( -5.188838149069471174E-16, 1.699382548006136313E-16, 1.000000000000000000 ) ) ;
#3654 = CARTESIAN_POINT ( 'NONE',  ( -6.437058721807690810E-14, 62.83146620154573014, 4.519164521849267879E-29 ) ) ;
#3655 = CARTESIAN_POINT ( 'NONE',  ( -23.75665686005077504, 76.91945007112674659, 1.523999999999994248 ) ) ;
#3656 = CARTESIAN_POINT ( 'NONE',  ( -3.590790587123838709E-14, 56.51998046905274009, 0.000000000000000000 ) ) ;
#3657 = AXIS2_PLACEMENT_3D ( 'NONE', #25269, #18657, #38482 ) ;
#3658 = CARTESIAN_POINT ( 'NONE',  ( 0.001319893060084358647, 116.4580521601689185, -0.06605284600166361209 ) ) ;
#3659 = PLANE ( 'NONE',  #32946 ) ;
#3660 = VECTOR ( 'NONE', #1051, 1000.000000000000227 ) ;
#3661 = CARTESIAN_POINT ( 'NONE',  ( -3.987655724683881076, 118.7629491485398319, 0.9447994846549702119 ) ) ;
#3662 = CARTESIAN_POINT ( 'NONE',  ( -28.65049350906917880, 77.81814547195517662, -1.270000000000007789 ) ) ;
#3663 = CARTESIAN_POINT ( 'NONE',  ( 2.424293868422599640, 38.64141628508733817, -1.187741880963723462 ) ) ;
#3664 = CARTESIAN_POINT ( 'NONE',  ( 19.67869083727173773, 136.1149058410947532, 2.266608711299010093 ) ) ;
#3665 = CARTESIAN_POINT ( 'NONE',  ( 4.453423564604278795, 13.74662854910535792, -1.294644163995742225 ) ) ;
#3666 = CARTESIAN_POINT ( 'NONE',  ( 8.431793794909870243, 26.85621209503467455, -0.1224882448600171925 ) ) ;
#3667 = B_SPLINE_CURVE_WITH_KNOTS ( 'NONE', 3,
 ( #24949, #27932, #41367, #5172 ),
 .UNSPECIFIED., .F., .F.,
 ( 4, 4 ),
 ( 0.6010210485952584003, 1.000000000000000000 ),
 .UNSPECIFIED. ) ;
#3668 = CARTESIAN_POINT ( 'NONE',  ( 5.512878477348360562, 117.1944552775264583, -0.5780071930592981522 ) ) ;
#3669 = CARTESIAN_POINT ( 'NONE',  ( -2.033169340630109012, 122.5452913651401587, -0.2335185838714207707 ) ) ;
#3670 = DIRECTION ( 'NONE',  ( -3.035386659626960118E-16, 0.000000000000000000, -1.000000000000000000 ) ) ;
#3671 = CARTESIAN_POINT ( 'NONE',  ( -3.542958166033328027, 109.5877865956762918, -3.777787172267635274 ) ) ;
#3672 = CARTESIAN_POINT ( 'NONE',  ( 1.647191011186240006, 104.6144662015456817, 4.545328325604496733 ) ) ;
#3673 = CARTESIAN_POINT ( 'NONE',  ( -3.957843245660688680, 22.95775517496322848, 2.395914033147342970 ) ) ;
#3674 = CARTESIAN_POINT ( 'NONE',  ( -3.466430381603673005, 50.13146620154573441, -1.339521056010489319 ) ) ;
#3675 = CARTESIAN_POINT ( 'NONE',  ( -1.569967658166198543, 117.3993836205931700, -1.461707296722773775 ) ) ;
#3676 = CARTESIAN_POINT ( 'NONE',  ( 3.394644278243977187, -13.41358914320520057, 2.304069835958892032 ) ) ;
#3677 = EDGE_CURVE ( 'NONE', #29032, #25412, #35408, .T. ) ;
#3678 = ADVANCED_FACE ( 'NONE', ( #6236 ), #19206, .F. ) ;
#3679 = CARTESIAN_POINT ( 'NONE',  ( 0.9959059386942926695, 109.5507526474568607, -3.831187545969640951 ) ) ;
#3680 = CARTESIAN_POINT ( 'NONE',  ( -22.91546036685028653, 149.1739538623130272, 0.5130544771887699529 ) ) ;
#3681 = DIRECTION ( 'NONE',  ( -0.3582377630123915746, 0.9336303900108851028, -3.445432962228667069E-16 ) ) ;
#3682 = ORIENTED_EDGE ( 'NONE', *, *, #26631, .F. ) ;
#3683 = CARTESIAN_POINT ( 'NONE',  ( -11.34554992887676406, 77.73165686004495001, 1.270000000000000462 ) ) ;
#3684 = ORIENTED_EDGE ( 'NONE', *, *, #15651, .F. ) ;
#3685 = CARTESIAN_POINT ( 'NONE',  ( -6.442660433036017764, 29.32943145771791649, -0.01012415147099491285 ) ) ;
#3686 = CIRCLE ( 'NONE', #1617, 0.2540000000000015024 ) ;
#3687 = CARTESIAN_POINT ( 'NONE',  ( 5.680254533628135150, -15.02324869320220735, 2.089386157847644920 ) ) ;
#3688 = CARTESIAN_POINT ( 'NONE',  ( -19.92238394974720350, 148.9191654756151024, 1.700261758071553775 ) ) ;
#3689 = CARTESIAN_POINT ( 'NONE',  ( 5.164160201466080125, 158.7070047875298826, -1.240540739692758576 ) ) ;
#3690 = CARTESIAN_POINT ( 'NONE',  ( -4.288638401707804526, -7.253218809911426312, -1.756103832032595680 ) ) ;
#3691 = CARTESIAN_POINT ( 'NONE',  ( -58.82051709867915434, -0.2694835746722941683, -0.08083543577478463638 ) ) ;
#3692 = ORIENTED_EDGE ( 'NONE', *, *, #11857, .T. ) ;
#3693 = CARTESIAN_POINT ( 'NONE',  ( -27.82636559844506152, 59.51700088791086074, -1.270000000000004237 ) ) ;
#3694 = CARTESIAN_POINT ( 'NONE',  ( 0.6121664022496100532, 114.3327162918516962, 2.181662845130500905 ) ) ;
#3695 = CARTESIAN_POINT ( 'NONE',  ( -4.799585727462988949, 117.4716807894286461, 1.004530280717990331 ) ) ;
#3696 = TOROIDAL_SURFACE ( 'NONE', #9122, 8.794749999999998735, 0.2540000000000000036 ) ;
#3697 = CARTESIAN_POINT ( 'NONE',  ( -16.13547353508420557, 149.3012944676311804, 1.369731486774125262 ) ) ;
#3698 = DIRECTION ( 'NONE',  ( 6.353134868986659519E-16, -1.000000000000000000, 0.000000000000000000 ) ) ;
#3699 = CARTESIAN_POINT ( 'NONE',  ( 11.06957317628260995, 122.5598569164413334, -1.209814958810230712 ) ) ;
#3700 = CARTESIAN_POINT ( 'NONE',  ( -4.930931983215480763, 118.2512723699127832, -1.012396356527061503 ) ) ;
#3701 = CARTESIAN_POINT ( 'NONE',  ( -57.15088083682995546, 2.378576142695001838, -1.865916551128065981 ) ) ;
#3702 = CIRCLE ( 'NONE', #14550, 8.794749999999993406 ) ;
#3703 = VERTEX_POINT ( 'NONE', #271 ) ;
#3704 = CARTESIAN_POINT ( 'NONE',  ( 4.364081292726229577, 118.1821858711944486, -0.4478306246164636129 ) ) ;
#3705 = CARTESIAN_POINT ( 'NONE',  ( 9.401300499464312566, 153.8930958044198576, -0.5598851911991605812 ) ) ;
#3706 = ORIENTED_EDGE ( 'NONE', *, *, #30257, .F. ) ;
#3707 = CARTESIAN_POINT ( 'NONE',  ( -17.26689864452599110, 148.5513402141484391, -2.222558794446809927 ) ) ;
#3708 = CARTESIAN_POINT ( 'NONE',  ( 3.228916932056940858, -14.69740968606676823, 0.4668019137946345376 ) ) ;
#3709 = AXIS2_PLACEMENT_3D ( 'NONE', #28921, #41524, #42150 ) ;
#3710 = CARTESIAN_POINT ( 'NONE',  ( -3.174366308152011484, 63.84746620154572838, -0.06343139340882730792 ) ) ;
#3711 = ADVANCED_FACE ( 'NONE', ( #57 ), #10980, .T. ) ;
#3712 = CARTESIAN_POINT ( 'NONE',  ( -58.34169784303173856, -0.2326338189565652081, 0.2089577666115795540 ) ) ;
#3713 = CARTESIAN_POINT ( 'NONE',  ( 4.577905313181523717, 13.52175256873284326, -0.6256056815880789435 ) ) ;
#3714 = CARTESIAN_POINT ( 'NONE',  ( 1.409834354326054529, 119.9358631726476574, 0.5453972335014175554 ) ) ;
#3715 = CARTESIAN_POINT ( 'NONE',  ( -3.148634455474564220, 30.89457961443325118, -0.4672107454865900844 ) ) ;
#3716 = VECTOR ( 'NONE', #19059, 1000.000000000000000 ) ;
#3717 = CARTESIAN_POINT ( 'NONE',  ( -2.707926769430928804, 11.08828375386998033, -3.745406074561137721 ) ) ;
#3718 = CARTESIAN_POINT ( 'NONE',  ( 8.575029486087361263, 123.3373102669514765, 0.3234659723512186003 ) ) ;
#3719 = CARTESIAN_POINT ( 'NONE',  ( -10.28897677580358305, 57.14999999999998437, 5.016499999999999737 ) ) ;
#3720 = CARTESIAN_POINT ( 'NONE',  ( -54.90394170586843359, 6.776736168479208011, -2.460356751892069038 ) ) ;
#3721 = CARTESIAN_POINT ( 'NONE',  ( -2.182332153769093619, 116.1897970674740748, -0.04360822100399409929 ) ) ;
#3722 = DIRECTION ( 'NONE',  ( -0.003125310045706406609, -0.9876883405951376593, 0.1564032425800100379 ) ) ;
#3723 = CARTESIAN_POINT ( 'NONE',  ( -47.35944255389389923, 21.37623662739411401, 4.722871667523157235 ) ) ;
#3724 = DIRECTION ( 'NONE',  ( 0.8745520943968235761, -0.4849315768086558398, 0.000000000000000000 ) ) ;
#3725 = CARTESIAN_POINT ( 'NONE',  ( -29.27789202445837091, 65.71096991539570809, -1.269999999999910090 ) ) ;
#3726 = CARTESIAN_POINT ( 'NONE',  ( -58.63679809531443965, -0.7731007215655836262, -1.422417852365874970E-12 ) ) ;
#3727 = DIRECTION ( 'NONE',  ( -0.9998004120163608288, 0.000000000000000000, -0.01997839162482747608 ) ) ;
#3728 = DIRECTION ( 'NONE',  ( -0.7548010569845451379, -0.6559537821943047797, 0.000000000000000000 ) ) ;
#3729 = CARTESIAN_POINT ( 'NONE',  ( -57.67985703563598321, 3.143487229238031588, 0.2637475255842167132 ) ) ;
#3730 = ADVANCED_FACE ( 'NONE', ( #16638 ), #18445, .T. ) ;
#3731 = CARTESIAN_POINT ( 'NONE',  ( -57.22363667057550884, 2.289652018204080264, 1.875138655370640173 ) ) ;
#3732 = CARTESIAN_POINT ( 'NONE',  ( -15.55989727259158606, 120.8127473925414108, -0.08007127899889533718 ) ) ;
#3733 = ORIENTED_EDGE ( 'NONE', *, *, #22706, .T. ) ;
#3734 = CARTESIAN_POINT ( 'NONE',  ( -53.35592009511452716, 14.94916803242400682, -1.377413129700665539 ) ) ;
#3735 = CARTESIAN_POINT ( 'NONE',  ( 7.793436386033940622, 122.5978578380440638, 0.02760177019608184637 ) ) ;
#3736 = ORIENTED_EDGE ( 'NONE', *, *, #24238, .T. ) ;
#3737 = FACE_OUTER_BOUND ( 'NONE', #19043, .T. ) ;
#3738 = CARTESIAN_POINT ( 'NONE',  ( -11.84172335778374041, 151.9972573545839225, -0.3576891575424541725 ) ) ;
#3739 = CARTESIAN_POINT ( 'NONE',  ( 2.113928706699719218, -15.46215275738946282, 5.949113654003534535 ) ) ;
#3740 = CARTESIAN_POINT ( 'NONE',  ( -17.54996479678720434, 128.5781302034472162, 1.330722490425295668 ) ) ;
#3741 = CARTESIAN_POINT ( 'NONE',  ( 4.037907715354051241, 27.70556447992504445, -2.267523456217593214 ) ) ;
#3742 = CARTESIAN_POINT ( 'NONE',  ( 18.54376275836449040, 154.1690995007799927, 0.7937872377295740467 ) ) ;
#3743 = CARTESIAN_POINT ( 'NONE',  ( 2.189939624171645338, -15.48487759952872622, 5.886065356993532838 ) ) ;
#3744 = CARTESIAN_POINT ( 'NONE',  ( 11.58677707360137532, 17.14500000000046498, -4.474811398758258285 ) ) ;
#3745 = CARTESIAN_POINT ( 'NONE',  ( -0.2812775050834619428, 1.806455656379289287, -0.9370761103187740249 ) ) ;
#3746 = CARTESIAN_POINT ( 'NONE',  ( -23.33231982438486085, 148.8574307740229585, -0.6970557703302364683 ) ) ;
#3747 = DIRECTION ( 'NONE',  ( 4.017660918040594346E-17, -1.000000000000000000, -2.376309959284834438E-19 ) ) ;
#3748 = EDGE_CURVE ( 'NONE', #38326, #37552, #39233, .T. ) ;
#3749 = CARTESIAN_POINT ( 'NONE',  ( 14.73199999999999754, 61.59499999999999886, 5.016499999999999737 ) ) ;
#3750 = ORIENTED_EDGE ( 'NONE', *, *, #4875, .T. ) ;
#3751 = CARTESIAN_POINT ( 'NONE',  ( 8.785006194573600879, 117.7265864523129721, 0.3950309330525467733 ) ) ;
#3752 = VERTEX_POINT ( 'NONE', #33485 ) ;
#3753 = CARTESIAN_POINT ( 'NONE',  ( -10.76835564758012609, 122.7614441063800399, 1.139041423164458333 ) ) ;
#3754 = CARTESIAN_POINT ( 'NONE',  ( -58.25346979615795817, -0.04388205940947602357, -0.4484691845572629787 ) ) ;
#3755 = CARTESIAN_POINT ( 'NONE',  ( 21.29267830536744555, 148.0064520001644723, 2.314741142932118745 ) ) ;
#3756 = CARTESIAN_POINT ( 'NONE',  ( 17.46034360794347506, 151.5007859583534753, -1.733980983366192330 ) ) ;
#3757 = CARTESIAN_POINT ( 'NONE',  ( 0.9605196170170531289, 3.153480984720312019, -0.1630338022177024171 ) ) ;
#3758 = CARTESIAN_POINT ( 'NONE',  ( -17.24095835932504528, 153.8449085212272678, -1.984086636893841460 ) ) ;
#3759 = CARTESIAN_POINT ( 'NONE',  ( 4.614683254511476207, 118.0411034907158978, -0.6410491579301769161 ) ) ;
#3760 = CARTESIAN_POINT ( 'NONE',  ( 4.497658079232150996, 104.6144662015457527, 1.758835774424003962 ) ) ;
#3761 = CARTESIAN_POINT ( 'NONE',  ( 1.473868052710539889, 120.2326517397585377, -0.4086940711265544257 ) ) ;
#3762 = CARTESIAN_POINT ( 'NONE',  ( -8.770618086121094947, 123.6813396614493712, -0.1752578222716850431 ) ) ;
#3763 = ORIENTED_EDGE ( 'NONE', *, *, #25627, .F. ) ;
#3764 = CARTESIAN_POINT ( 'NONE',  ( -13.63191106101887407, 125.8243951943327517, -1.964466803988918153 ) ) ;
#3765 = CARTESIAN_POINT ( 'NONE',  ( 4.930802857217395641, -15.55747185075553851, 2.516589264972601825 ) ) ;
#3766 = CARTESIAN_POINT ( 'NONE',  ( -4.801647862234980302, 117.4032733357427105, 1.015449305853463491 ) ) ;
#3767 = CARTESIAN_POINT ( 'NONE',  ( -4.553380338773690639, 118.0136081097811029, -0.8849348180924038187 ) ) ;
#3768 = EDGE_CURVE ( 'NONE', #5200, #39243, #23208, .T. ) ;
#3769 = CARTESIAN_POINT ( 'NONE',  ( -46.31144060707497090, 24.05480373873685451, -2.308638262703932575 ) ) ;
#3770 = CARTESIAN_POINT ( 'NONE',  ( -5.177913976931285411, 57.14999999999999858, -5.372100000000001430 ) ) ;
#3771 = CARTESIAN_POINT ( 'NONE',  ( 18.05261769607643174, 144.6555253171603397, 2.402359405240795276 ) ) ;
#3772 = DIRECTION ( 'NONE',  ( -5.188838149069471174E-16, 1.699382548006136313E-16, 1.000000000000000000 ) ) ;
#3773 = ADVANCED_FACE ( 'NONE', ( #40509 ), #21173, .T. ) ;
#3774 = CARTESIAN_POINT ( 'NONE',  ( 10.83330528665002923, 157.8980211815716928, 0.2164752214609689529 ) ) ;
#3775 = CARTESIAN_POINT ( 'NONE',  ( -4.148164184366740059, 118.0988315448752530, 0.6394906134413954613 ) ) ;
#3776 = EDGE_CURVE ( 'NONE', #5931, #35130, #2000, .T. ) ;
#3777 = CARTESIAN_POINT ( 'NONE',  ( -1.087716277807347254, 29.42523365726748708, -8.383486966309323662 ) ) ;
#3778 = CARTESIAN_POINT ( 'NONE',  ( 15.98475566209939913, 146.3393691146323761, 1.048177900600803625 ) ) ;
#3779 = CARTESIAN_POINT ( 'NONE',  ( 20.72298665840521892, 132.2482564273973935, -0.5730191400310227223 ) ) ;
#3780 = CARTESIAN_POINT ( 'NONE',  ( 4.788875734160475517, 117.8399135866531680, 0.9345395952325853406 ) ) ;
#3781 = CARTESIAN_POINT ( 'NONE',  ( -17.58995245299100674, 75.15621874538170744, -1.270000000000001572 ) ) ;
#3782 = CARTESIAN_POINT ( 'NONE',  ( -1.421603664355800101, 159.6054662015457666, -0.02840702444251828190 ) ) ;
#3783 = AXIS2_PLACEMENT_3D ( 'NONE', #18313, #31315, #41556 ) ;
#3784 = ORIENTED_EDGE ( 'NONE', *, *, #12552, .T. ) ;
#3785 = CARTESIAN_POINT ( 'NONE',  ( -6.683353917540686417, 120.8996509036314819, -1.027146486415592586 ) ) ;
#3786 = CARTESIAN_POINT ( 'NONE',  ( 22.53527615164647457, 150.7831677823004952, 0.4503084484864791626 ) ) ;
#3787 = CARTESIAN_POINT ( 'NONE',  ( -8.161245858290207877, 122.8283871457973362, -0.4521822771171595812 ) ) ;
#3788 = CARTESIAN_POINT ( 'NONE',  ( 4.240324834746892257, -11.68880992198167945, 0.6883502328505933798 ) ) ;
#3789 = CARTESIAN_POINT ( 'NONE',  ( -22.35542929045595528, 148.9358926463403918, 0.9984386947210763807 ) ) ;
#3790 = DIRECTION ( 'NONE',  ( 0.3256999990547897461, 0.9454731675810318370, 0.000000000000000000 ) ) ;
#3791 = CARTESIAN_POINT ( 'NONE',  ( 18.62929286701944420, 154.1293031355326946, 0.4449488992651827735 ) ) ;
#3792 = ORIENTED_EDGE ( 'NONE', *, *, #38602, .T. ) ;
#3793 = CARTESIAN_POINT ( 'NONE',  ( -3.416230376366909294, -5.529048218071860532, 3.121479803864907865 ) ) ;
#3794 = CARTESIAN_POINT ( 'NONE',  ( 4.783155644945383145, 105.1214970594926257, 2.386995739668397398 ) ) ;
#3795 = CARTESIAN_POINT ( 'NONE',  ( 4.646169936107913401, 117.9325745699973282, -0.7782960047779410306 ) ) ;
#3796 = CARTESIAN_POINT ( 'NONE',  ( -4.948559212928203443, 119.0884032316885737, 0.9007675068828924214 ) ) ;
#3797 = CARTESIAN_POINT ( 'NONE',  ( 4.623297697159335584, 3.588818502778304609, 0.3943307014320480697 ) ) ;
#3798 = CARTESIAN_POINT ( 'NONE',  ( 14.34385702226353132, 155.9958976045614349, 1.592240502911361766 ) ) ;
#3799 = CARTESIAN_POINT ( 'NONE',  ( 15.38000172824457046, 147.8312228276848543, 0.3073290369001837052 ) ) ;
#3801 = CARTESIAN_POINT ( 'NONE',  ( 2.213227627077498205, 118.1205262787358663, -0.6644466414026560797 ) ) ;
#3800 = DIRECTION ( 'NONE',  ( -0.01997839162482737546, -1.040247600000940825E-18, 0.9998004120163610509 ) ) ;
#3802 = CARTESIAN_POINT ( 'NONE',  ( -3.522755225739859775, -9.592572062075928940, 3.019445982675781348 ) ) ;
#3803 = CARTESIAN_POINT ( 'NONE',  ( -22.71086789718629717, 148.5871737753741115, -1.637050152828072092 ) ) ;
#3804 = ORIENTED_EDGE ( 'NONE', *, *, #34186, .F. ) ;
#3805 = CARTESIAN_POINT ( 'NONE',  ( -9.163388821854908883, 124.2347608867413413, -0.1831063163140473349 ) ) ;
#3806 = ADVANCED_FACE ( 'NONE', ( #24288 ), #10828, .F. ) ;
#3807 = CARTESIAN_POINT ( 'NONE',  ( -1.609565093910659161, 156.2658572007470639, 0.2453390865415089050 ) ) ;
#3808 = CARTESIAN_POINT ( 'NONE',  ( 4.956269154958684808, -14.57630274377035029, 4.209183869072664841 ) ) ;
#3809 =( BOUNDED_CURVE ( )  B_SPLINE_CURVE ( 3, ( #22267, #35717, #35930, #19501 ),
 .UNSPECIFIED., .F., .T. ) 
 B_SPLINE_CURVE_WITH_KNOTS ( ( 4, 4 ),
 ( 0.2498838476046065238, 0.5001855759278981406 ),
 .UNSPECIFIED. ) 
 CURVE ( )  GEOMETRIC_REPRESENTATION_ITEM ( )  RATIONAL_B_SPLINE_CURVE ( ( 0.5000007283237750677, 0.4995979372591229373, 0.6662643611511979147, 1.000000000000000000 ) ) 
 REPRESENTATION_ITEM ( '' )  );
#3810 = CARTESIAN_POINT ( 'NONE',  ( -5.861642722916909243, 64.54502714855203749, 1.270000000000005347 ) ) ;
#3811 = CARTESIAN_POINT ( 'NONE',  ( -1.039005592983597070, 105.9869000721054846, -5.237171080062087647 ) ) ;
#3813 = ORIENTED_EDGE ( 'NONE', *, *, #24095, .T. ) ;
#3812 = AXIS2_PLACEMENT_3D ( 'NONE', #5101, #8489, #1693 ) ;
#3814 = CARTESIAN_POINT ( 'NONE',  ( 10.78248307147193685, 155.9024031350590462, 2.169211330499416057 ) ) ;
#3815 = CARTESIAN_POINT ( 'NONE',  ( -14.50851225146815437, 78.09971119798315442, 5.392902600000138769 ) ) ;
#3816 = CARTESIAN_POINT ( 'NONE',  ( 9.118174893680169646, 124.1671967267183589, 0.1822028344259500054 ) ) ;
#3817 = CARTESIAN_POINT ( 'NONE',  ( -0.01443894962468954962, 159.4760848062415732, 0.7225840825867287931 ) ) ;
#3818 = ADVANCED_FACE ( 'NONE', ( #4314 ), #10467, .T. ) ;
#3819 = CARTESIAN_POINT ( 'NONE',  ( 0.2322036383927537639, 20.64316925235604216, 8.417729739967510838 ) ) ;
#3820 = CARTESIAN_POINT ( 'NONE',  ( 4.409042980950512280, 120.6578283891288379, 0.6218799582752132515 ) ) ;
#3821 = EDGE_CURVE ( 'NONE', #31300, #40156, #33694, .T. ) ;
#3822 = CARTESIAN_POINT ( 'NONE',  ( 22.54544115201711563, 150.6069110094195764, -0.1392563518891843932 ) ) ;
#3823 = DIRECTION ( 'NONE',  ( 0.9998004120163610509, 5.205824365704083805E-17, 0.01997839162482749689 ) ) ;
#3824 = CARTESIAN_POINT ( 'NONE',  ( -50.84765044967730319, 14.73090700864087488, 4.586134481135779595 ) ) ;
#3825 = CARTESIAN_POINT ( 'NONE',  ( -48.35471193741586404, 22.70554656608007704, 1.835820227619837208 ) ) ;
#3826 = CARTESIAN_POINT ( 'NONE',  ( 1.424304860752266144, 106.0679449480461329, -5.142703936578335799 ) ) ;
#3827 = CARTESIAN_POINT ( 'NONE',  ( -55.60508136934060275, 7.116827924314645060, 3.170888472016278214 ) ) ;
#3828 = CARTESIAN_POINT ( 'NONE',  ( -58.68986611463690650, -0.3143780598132880910, 0.3000052052140327885 ) ) ;
#3829 = CARTESIAN_POINT ( 'NONE',  ( -4.547855832773509910, 118.1104907970478024, 0.5056323322026208267 ) ) ;
#3830 = CARTESIAN_POINT ( 'NONE',  ( -58.15296624161964445, 0.1186235457594081444, -0.2061892363120086946 ) ) ;
#3831 = PRODUCT_DEFINITION_SHAPE ( 'NONE', 'NONE',  #42164 ) ;
#3832 = ORIENTED_EDGE ( 'NONE', *, *, #38059, .F. ) ;
#3833 = CARTESIAN_POINT ( 'NONE',  ( -46.89970385779243855, 22.02655025333852379, 4.237790764466920379 ) ) ;
#3834 = CARTESIAN_POINT ( 'NONE',  ( -6.041464496458629263, 119.4136938840325399, -1.263443438576810518 ) ) ;
#3835 = CARTESIAN_POINT ( 'NONE',  ( -7.424629525399851104, 123.6670498955208473, -0.1830506623709852454 ) ) ;
#3836 = CARTESIAN_POINT ( 'NONE',  ( 4.534800580971761974, 118.0743626807513209, 0.7973481318499234805 ) ) ;
#3837 = CARTESIAN_POINT ( 'NONE',  ( -16.08743688339782807, 147.0533492130506943, -1.289446542218032565 ) ) ;
#3838 = CARTESIAN_POINT ( 'NONE',  ( -15.42835734045148399, 79.74558783746839197, -1.524000000000001576 ) ) ;
#3839 = DIRECTION ( 'NONE',  ( -0.8745520943968240202, 0.4849315768086553402, -6.829619984160650158E-16 ) ) ;
#3840 = CARTESIAN_POINT ( 'NONE',  ( 0.1065646865914872399, 105.8844662015456777, -5.332932678536313809 ) ) ;
#3841 = CARTESIAN_POINT ( 'NONE',  ( -16.56824576912640623, 144.0643239018434940, -1.930375849691871704 ) ) ;
#3842 = CARTESIAN_POINT ( 'NONE',  ( 5.256943553860875973, 116.0444662015457027, 1.293952898321280021 ) ) ;
#3843 = CARTESIAN_POINT ( 'NONE',  ( -0.001640166039862459230, 159.6041700698465036, 0.08208061555506504514 ) ) ;
#3844 = AXIS2_PLACEMENT_3D ( 'NONE', #20970, #5658, #5232 ) ;
#3845 = CARTESIAN_POINT ( 'NONE',  ( 8.026787933082662363, 121.5445110286361086, -0.8405406253987532939 ) ) ;
#3846 = CARTESIAN_POINT ( 'NONE',  ( -2.856921527171903286, 121.0288202834496190, 0.01139528386683224398 ) ) ;
#3847 = CARTESIAN_POINT ( 'NONE',  ( -4.627450822138572839, 2.892058097378844117, -0.1328416527703782657 ) ) ;
#3848 = CARTESIAN_POINT ( 'NONE',  ( 21.51154278844947854, 151.3526640061693342, 1.384567357891493211 ) ) ;
#3849 = DIRECTION ( 'NONE',  ( -0.8745520943968937422, 0.4849315768085294409, -5.691349986800560698E-16 ) ) ;
#3850 = CARTESIAN_POINT ( 'NONE',  ( 3.375754317642519098, -15.02680299829225952, 2.760009546110721246 ) ) ;
#3851 = CARTESIAN_POINT ( 'NONE',  ( -16.64003893621130459, 151.1890201267100906, 1.733044620493700894 ) ) ;
#3852 = CARTESIAN_POINT ( 'NONE',  ( 0.9680108232324700079, 2.729151709021603978, 0.1071397942825247085 ) ) ;
#3853 = CARTESIAN_POINT ( 'NONE',  ( -21.11962238282699644, 132.3956117394162106, -1.087766252141818102 ) ) ;
#3854 = CARTESIAN_POINT ( 'NONE',  ( -0.6834205802178441314, -7.050398998296187436, -0.6963091382628930903 ) ) ;
#3855 = VERTEX_POINT ( 'NONE', #30064 ) ;
#3856 = CARTESIAN_POINT ( 'NONE',  ( -41.36952270831616119, 22.75442529069328401, 0.6632742133606186474 ) ) ;
#3857 = CARTESIAN_POINT ( 'NONE',  ( 3.394470486402062281, 108.6891572770382624, 4.119616105806038320 ) ) ;
#3858 = CONTEXT_DEPENDENT_SHAPE_REPRESENTATION ( #41787, #23887 ) ;
#3859 = CARTESIAN_POINT ( 'NONE',  ( -8.995803412248951858, 123.1852847016406685, 0.4677080646552715382 ) ) ;
#3860 = CARTESIAN_POINT ( 'NONE',  ( 1.930977371672661924, -15.05712096081325591, 5.742647184725750087 ) ) ;
#3861 = CARTESIAN_POINT ( 'NONE',  ( 0.009513407573606913470, 119.7614543879625586, -0.4760898169610157660 ) ) ;
#3862 = CARTESIAN_POINT ( 'NONE',  ( -3.256054338613478816, 118.9727644790723531, -0.9029027703446362851 ) ) ;
#3863 = CARTESIAN_POINT ( 'NONE',  ( 3.260699289283686131, 104.6144662015457669, 3.570726652107954813 ) ) ;
#3864 = CARTESIAN_POINT ( 'NONE',  ( 3.187143392547471255, -14.52651900126690876, 3.212499789951002604 ) ) ;
#3865 = CARTESIAN_POINT ( 'NONE',  ( -6.313817790419506082, 30.81489375714620138, 1.175039937232976062 ) ) ;
#3866 = CARTESIAN_POINT ( 'NONE',  ( 15.40211203110474969, 147.8297367799732456, 0.07919316026241145223 ) ) ;
#3867 = ORIENTED_EDGE ( 'NONE', *, *, #24853, .T. ) ;
#3868 = CARTESIAN_POINT ( 'NONE',  ( -2.633132161630451940, 107.2195770060342284, 4.632131451278267420 ) ) ;
#3870 = EDGE_CURVE ( 'NONE', #6455, #3855, #29194, .T. ) ;
#3869 = FACE_OUTER_BOUND ( 'NONE', #12428, .T. ) ;
#3871 = DIRECTION ( 'NONE',  ( 0.1469470846586743706, 9.335746474409589170E-17, 0.9891443546370348727 ) ) ;
#3872 = EDGE_CURVE ( 'NONE', #1116, #38897, #4101, .T. ) ;
#3873 = CIRCLE ( 'NONE', #28321, 5.588000000000006295 ) ;
#3874 = DIRECTION ( 'NONE',  ( 5.188838149069472160E-16, -1.699382548006136559E-16, -1.000000000000000000 ) ) ;
#3875 = CARTESIAN_POINT ( 'NONE',  ( 3.739900805225205183, 116.6566025657135413, -0.03821340562556407167 ) ) ;
#3876 = CARTESIAN_POINT ( 'NONE',  ( -5.793465281260614219, 118.4310156723767307, 0.4331262667984490666 ) ) ;
#3877 = CARTESIAN_POINT ( 'NONE',  ( -0.01822531903872333034, 118.1564764849152738, 0.9120692297075591037 ) ) ;
#3878 = CARTESIAN_POINT ( 'NONE',  ( 12.16475753114682767, 55.74362973025085211, 5.016499999999999737 ) ) ;
#3879 = CARTESIAN_POINT ( 'NONE',  ( -4.061900884676539647, 32.22309257017796824, 0.8408443696299722214 ) ) ;
#3880 = CARTESIAN_POINT ( 'NONE',  ( 1.134298505455532569, 158.7113841514841681, 1.516915449716996989 ) ) ;
#3881 = CARTESIAN_POINT ( 'NONE',  ( 2.838909340336904563, 21.51804255560577772, 3.663749385350952181 ) ) ;
#3882 = CARTESIAN_POINT ( 'NONE',  ( 2.985612812371020386, 19.08565862607713370, -7.890306666671915714 ) ) ;
#3883 = CARTESIAN_POINT ( 'NONE',  ( 8.618216296094656670, 118.6576028950189823, -0.8123356437107368544 ) ) ;
#3884 = CARTESIAN_POINT ( 'NONE',  ( -1.682799138809848882, 120.1914007830323214, -0.5335993566373051777 ) ) ;
#3885 = FACE_OUTER_BOUND ( 'NONE', #35928, .T. ) ;
#3886 = CARTESIAN_POINT ( 'NONE',  ( -0.9117815773467171647, 106.1653671795302074, -5.214745729516177875 ) ) ;
#3887 = CARTESIAN_POINT ( 'NONE',  ( -3.698849545476382783, 105.1233800755782255, 3.857623938754290105 ) ) ;
#3888 = AXIS2_PLACEMENT_3D ( 'NONE', #31131, #1968, #18334 ) ;
#3889 = CARTESIAN_POINT ( 'NONE',  ( -2.614655561276646889, 23.60746518810343986, 3.812863311767609620 ) ) ;
#3890 = FACE_OUTER_BOUND ( 'NONE', #12202, .T. ) ;
#3891 = CARTESIAN_POINT ( 'NONE',  ( -9.925711944554160837, 78.55658865046541450, -5.016499999999999737 ) ) ;
#3892 = CARTESIAN_POINT ( 'NONE',  ( 3.243601939617143159, -13.81697766888033385, 2.329280267808830907 ) ) ;
#3893 = CARTESIAN_POINT ( 'NONE',  ( 1.702772465368721511, 120.1914007830323214, -0.4659475787731966467 ) ) ;
#3894 = CARTESIAN_POINT ( 'NONE',  ( -1.955870317219649213, 116.9162416783649689, 0.3393494064863860626 ) ) ;
#3895 = CARTESIAN_POINT ( 'NONE',  ( 5.008289758173663841, 117.3984635900009295, -0.7758770640922041384 ) ) ;
#3896 = VERTEX_POINT ( 'NONE', #20040 ) ;
#3897 = CARTESIAN_POINT ( 'NONE',  ( 5.177913976931216133, 53.58606249999999704, 5.372100000000000541 ) ) ;
#3898 = AXIS2_PLACEMENT_3D ( 'NONE', #7215, #36601, #20801 ) ;
#3899 = VERTEX_POINT ( 'NONE', #37293 ) ;
#3900 = CARTESIAN_POINT ( 'NONE',  ( -7.213960532363675959, 86.35999999999998522, 1.904999999999995364 ) ) ;
#3901 = CARTESIAN_POINT ( 'NONE',  ( 4.914263517198875775, -15.39432152949170352, 0.3857354017804055513 ) ) ;
#3902 = CARTESIAN_POINT ( 'NONE',  ( -20.30545318303849456, 145.4934252350392114, 1.680122328351855820 ) ) ;
#3903 = CARTESIAN_POINT ( 'NONE',  ( 14.28818831795921440, 121.8555783441548073, -1.022170725131337665 ) ) ;
#3904 = CARTESIAN_POINT ( 'NONE',  ( 0.4343283552818534288, -9.202337043772711667, -4.603842121470758997 ) ) ;
#3905 = CARTESIAN_POINT ( 'NONE',  ( 3.174366308151880922, 104.6144662015457243, 0.06343139340882769650 ) ) ;
#3906 = ORIENTED_EDGE ( 'NONE', *, *, #23278, .T. ) ;
#3907 = DIRECTION ( 'NONE',  ( -0.3256999990547876367, -0.9454731675810326141, -8.328397965208553695E-18 ) ) ;
#3908 = VECTOR ( 'NONE', #38448, 1000.000000000000114 ) ;
#3909 = CARTESIAN_POINT ( 'NONE',  ( 0.7127221660106257684, 117.6736730875354766, 1.182500608623780813 ) ) ;
#3910 = CARTESIAN_POINT ( 'NONE',  ( 4.856046737116808565, 117.4074955614782851, 1.171143430823223808 ) ) ;
#3911 = CARTESIAN_POINT ( 'NONE',  ( -16.84814155439281080, 148.3581316477378493, 1.364645798843572955 ) ) ;
#3912 = CARTESIAN_POINT ( 'NONE',  ( -7.961576494521615643, 72.55615504727386167, 1.524000000000003130 ) ) ;
#3913 = CARTESIAN_POINT ( 'NONE',  ( 18.09605103972940654, 148.5173242358814321, -1.660853775707743285 ) ) ;
#3914 = CARTESIAN_POINT ( 'NONE',  ( -7.739031927415108036, 119.2688035297948659, -1.343379870322972236 ) ) ;
#3915 = CARTESIAN_POINT ( 'NONE',  ( 10.28897677580358128, 56.51500000000000057, 4.381499999999999950 ) ) ;
#3916 = ORIENTED_EDGE ( 'NONE', *, *, #34254, .T. ) ;
#3917 = CARTESIAN_POINT ( 'NONE',  ( 4.447414120290241080, 118.1635491156278448, -0.4464743765249865604 ) ) ;
#3918 = CARTESIAN_POINT ( 'NONE',  ( 9.519849589794681322, 124.0643708016488063, -0.3285928725474104861 ) ) ;
#3919 = ORIENTED_EDGE ( 'NONE', *, *, #34423, .F. ) ;
#3920 = CARTESIAN_POINT ( 'NONE',  ( 3.259035188333455846, -14.62011735832338744, 2.262668647611313588 ) ) ;
#3921 = DIRECTION ( 'NONE',  ( 0.9998004120163608288, 0.000000000000000000, 0.01997839162482760791 ) ) ;
#3922 = VECTOR ( 'NONE', #24190, 1000.000000000000000 ) ;
#3923 = DIRECTION ( 'NONE',  ( 0.01997839162482749689, 1.040247600000945640E-18, -0.9998004120163610509 ) ) ;
#3924 = EDGE_CURVE ( 'NONE', #38171, #39389, #41472, .T. ) ;
#3925 = CARTESIAN_POINT ( 'NONE',  ( -2.426139246716550346, 10.07336736126799437, 3.943011612146583023 ) ) ;
#3926 = CARTESIAN_POINT ( 'NONE',  ( 2.024284171598446314, 156.9412006218898057, 1.489060257140892407 ) ) ;
#3927 = CARTESIAN_POINT ( 'NONE',  ( -2.880736501481948153, 31.22451072257329585, 0.7774695130801791976 ) ) ;
#3928 = CARTESIAN_POINT ( 'NONE',  ( -0.9211762648548540433, 10.43857344512876040, -4.529598961101950927 ) ) ;
#3929 = CARTESIAN_POINT ( 'NONE',  ( 15.74517894787269867, 145.7063497038720925, 0.5455200375299577020 ) ) ;
#3930 = CARTESIAN_POINT ( 'NONE',  ( -16.60960244842765476, 9.026346327358517385, 2.034089647357696543E-15 ) ) ;
#3931 = AXIS2_PLACEMENT_3D ( 'NONE', #29157, #12969, #25962 ) ;
#3932 = CARTESIAN_POINT ( 'NONE',  ( -54.85284047870325708, 7.073525668766899699, -2.945785012852154772 ) ) ;
#3933 = CARTESIAN_POINT ( 'NONE',  ( 2.175103472038542929, 116.2667018202340898, -0.1328812213640993556 ) ) ;
#3934 = CARTESIAN_POINT ( 'NONE',  ( 10.83330528665002923, 157.8980211815716928, 0.2164752214609689529 ) ) ;
#3935 = CYLINDRICAL_SURFACE ( 'NONE', #11146, 0.2539999999999992819 ) ;
#3936 = CARTESIAN_POINT ( 'NONE',  ( -12.21488373879589240, 17.14500000000000313, -5.016499999999999737 ) ) ;
#3937 = CARTESIAN_POINT ( 'NONE',  ( -28.99046981646804966, 65.28995187596837013, -1.524000000000005572 ) ) ;
#3938 = DIRECTION ( 'NONE',  ( -0.8745520943968240202, 0.4849315768086551737, -5.361993529360572958E-16 ) ) ;
#3939 = CARTESIAN_POINT ( 'NONE',  ( -5.706177858045075268, 56.51500000000000057, 5.041924731713889329 ) ) ;
#3940 = CARTESIAN_POINT ( 'NONE',  ( -14.50851225146815615, 78.09971119798315442, -1.904999999999999583 ) ) ;
#3941 = CARTESIAN_POINT ( 'NONE',  ( -58.77954282417582732, 0.05649391281087323691, 0.1080441935232383244 ) ) ;
#3942 = CARTESIAN_POINT ( 'NONE',  ( -58.20820809768403592, 1.420579653404085985, 1.355822160094593443 ) ) ;
#3943 = CARTESIAN_POINT ( 'NONE',  ( -1.881116149107413760, 116.6503132507590124, 0.1904188032791132856 ) ) ;
#3944 = ORIENTED_EDGE ( 'NONE', *, *, #10274, .F. ) ;
#3945 = CARTESIAN_POINT ( 'NONE',  ( -57.78461401849437351, 2.885363594410703225, -1.068429527248437518E-14 ) ) ;
#3946 = CARTESIAN_POINT ( 'NONE',  ( -6.980741664752802222, 121.9496248960778786, -0.1878529747284405360 ) ) ;
#3947 = ORIENTED_EDGE ( 'NONE', *, *, #19933, .T. ) ;
#3948 = DIRECTION ( 'NONE',  ( -1.000000000000000000, 0.000000000000000000, 0.000000000000000000 ) ) ;
#3949 = CARTESIAN_POINT ( 'NONE',  ( -3.750075860242207071, 121.0949217282140182, -0.1016972523499029696 ) ) ;
#3950 = CARTESIAN_POINT ( 'NONE',  ( 6.004855586296256931, -14.40561964533282335, 2.074926179989267094 ) ) ;
#3951 = CARTESIAN_POINT ( 'NONE',  ( -9.525696296010787378, 157.4068808874136209, 1.471446521238429561 ) ) ;
#3952 = CARTESIAN_POINT ( 'NONE',  ( 4.496586626007489151, 27.28078351817337222, -1.068494511273165193 ) ) ;
#3953 = CARTESIAN_POINT ( 'NONE',  ( 0.9228193675733716850, 116.5712332538976455, 0.1866785551396779874 ) ) ;
#3954 = AXIS2_PLACEMENT_3D ( 'NONE', #6987, #22924, #39574 ) ;
#3955 = CARTESIAN_POINT ( 'NONE',  ( 2.121138329832424230, -15.54773473020022756, 5.902882008759894106 ) ) ;
#3956 = CARTESIAN_POINT ( 'NONE',  ( -0.9950013725589796909, 29.65466048987409309, -4.513790593961638287 ) ) ;
#3957 = CARTESIAN_POINT ( 'NONE',  ( -0.006055453635351584415, 1.369653838947524349, -0.9756124606672940125 ) ) ;
#3958 = CARTESIAN_POINT ( 'NONE',  ( -23.06561215160527567, 149.8841935741895384, -0.7910477959972078699 ) ) ;
#3959 = CARTESIAN_POINT ( 'NONE',  ( -6.654617103318593247E-14, 104.6144662015457243, 1.534725424433578570E-31 ) ) ;
#3960 = CARTESIAN_POINT ( 'NONE',  ( 4.962376320764782633, 117.4036719250501335, 1.029954939118661095 ) ) ;
#3961 = EDGE_LOOP ( 'NONE', ( #36008, #12328, #25567, #20981 ) ) ;
#3962 = CARTESIAN_POINT ( 'NONE',  ( -5.552612348590429292, 116.8946703468410675, 0.3109655406019063983 ) ) ;
#3963 = CARTESIAN_POINT ( 'NONE',  ( -11.09075344257221474, 123.0430266451958232, 1.157373622111985467 ) ) ;
#3964 = CARTESIAN_POINT ( 'NONE',  ( -58.07329405781845111, 0.3456141243580676536, -0.7578522352846541743 ) ) ;
#3965 = CARTESIAN_POINT ( 'NONE',  ( 21.29237892510558439, 148.2102652567764380, 2.313897094871049553 ) ) ;
#3966 = CARTESIAN_POINT ( 'NONE',  ( 13.91587783890476793, 154.2684476645699760, -1.737230819368874135 ) ) ;
#3967 = CARTESIAN_POINT ( 'NONE',  ( 0.5230511744754561265, -14.76557578359995837, -0.8217837604668620788 ) ) ;
#3968 = CARTESIAN_POINT ( 'NONE',  ( -14.13476661394985179, 155.9232964860746620, -1.730687652093988449 ) ) ;
#3969 = CARTESIAN_POINT ( 'NONE',  ( 4.725354652796848853, 117.9692588958336046, -0.6261570487145760033 ) ) ;
#3970 = CARTESIAN_POINT ( 'NONE',  ( 4.833220906894529101, 105.1215657678094573, 2.265336830653343458 ) ) ;
#3971 = EDGE_CURVE ( 'NONE', #11659, #38242, #34652, .T. ) ;
#3972 = CARTESIAN_POINT ( 'NONE',  ( 9.956456675072738349, 154.0333045108203009, -1.106646445589350103 ) ) ;
#3973 = CARTESIAN_POINT ( 'NONE',  ( -7.045353508903627215, 122.0728772437221323, -0.1110369332536842307 ) ) ;
#3974 = VERTEX_POINT ( 'NONE', #20670 ) ;
#3975 = CARTESIAN_POINT ( 'NONE',  ( -5.029336563147013273, 119.5555251685854330, -1.067692183578045073 ) ) ;
#3976 = CARTESIAN_POINT ( 'NONE',  ( 4.883858777703569132, -15.45279978240890451, 0.9440085714135780792 ) ) ;
#3977 = FACE_OUTER_BOUND ( 'NONE', #33584, .T. ) ;
#3978 = CARTESIAN_POINT ( 'NONE',  ( -4.695219223534134123, 117.9582964687422617, -0.8613277202148715839 ) ) ;
#3979 = ADVANCED_FACE ( 'NONE', ( #14488 ), #20877, .F. ) ;
#3980 = CARTESIAN_POINT ( 'NONE',  ( -50.82551848962686591, 16.13924203555649228, -4.804203053272171786 ) ) ;
#3981 = B_SPLINE_CURVE_WITH_KNOTS ( 'NONE', 1,
 ( #39860, #10656 ),
 .UNSPECIFIED., .F., .F.,
 ( 2, 2 ),
 ( 0.000000000000000000, 1.000000000000000000 ),
 .UNSPECIFIED. ) ;
#3982 = CARTESIAN_POINT ( 'NONE',  ( 4.065926199369043204, 118.2429491485453354, 0.3080910687088499467 ) ) ;
#3983 = CARTESIAN_POINT ( 'NONE',  ( 0.8917109795614704959, 157.3234082283764792, 1.558336142952464032 ) ) ;
#3984 = CARTESIAN_POINT ( 'NONE',  ( -6.517733866319332394E-14, 78.32546620154573702, 2.848871684924056535E-29 ) ) ;
#3985 = CARTESIAN_POINT ( 'NONE',  ( 2.736438259132175865, 116.5290148844309357, 0.04129949523434448683 ) ) ;
#3986 = CARTESIAN_POINT ( 'NONE',  ( 7.891363246779867779, 17.78247237326412034, -2.951631208061117562 ) ) ;
#3987 = CARTESIAN_POINT ( 'NONE',  ( 0.6142257358152197755, 120.7813932625355307, 0.2072529566615757823 ) ) ;
#3988 = EDGE_CURVE ( 'NONE', #31840, #37219, #33988, .T. ) ;
#3989 = CARTESIAN_POINT ( 'NONE',  ( 22.27630879610695658, 150.1947564971097222, -0.7286472789443331211 ) ) ;
#3990 = CARTESIAN_POINT ( 'NONE',  ( -41.09670346151854403, 23.04688172093030829, -1.270085369932534958 ) ) ;
#3991 = ORIENTED_EDGE ( 'NONE', *, *, #32280, .F. ) ;
#3992 = DIRECTION ( 'NONE',  ( -0.9998004120163608288, 0.000000000000000000, -0.01997839162482749342 ) ) ;
#3993 = CARTESIAN_POINT ( 'NONE',  ( -22.69744207413532067, 137.3157656003441787, -0.3098006952201957098 ) ) ;
#3994 = EDGE_LOOP ( 'NONE', ( #26849, #22411, #31121, #13999 ) ) ;
#3995 = ADVANCED_FACE ( 'NONE', ( #27501 ), #30477, .F. ) ;
#3996 = CARTESIAN_POINT ( 'NONE',  ( -5.716351369186457809, 121.0728109688119787, -0.5777774213903609235 ) ) ;
#3997 = CARTESIAN_POINT ( 'NONE',  ( -17.14500000000466784, 71.11999999999886768, -1.524000000000000909 ) ) ;
#3998 = CARTESIAN_POINT ( 'NONE',  ( -7.609804580617608671, 122.3831840716419066, -0.4262428003126359499 ) ) ;
#3999 = CARTESIAN_POINT ( 'NONE',  ( 3.811713748825880543, -11.77916328849872052, 0.6977653098966205558 ) ) ;
#4000 = CARTESIAN_POINT ( 'NONE',  ( -22.14298845881056366, 148.3267584643486146, 1.148356825654135660 ) ) ;
#4001 = CARTESIAN_POINT ( 'NONE',  ( -7.126949251439574695, 78.78385021288468693, -2.234499184491881785 ) ) ;
#4002 = CARTESIAN_POINT ( 'NONE',  ( 23.33940156856670711, 149.0646716566344026, 0.5435133253920599872 ) ) ;
#4003 = ORIENTED_EDGE ( 'NONE', *, *, #9224, .T. ) ;
#4004 = CARTESIAN_POINT ( 'NONE',  ( -4.637963820743935983, -6.603494994175692412, 0.1710436084038768345 ) ) ;
#4005 = ADVANCED_FACE ( 'NONE', ( #3890 ), #11096, .T. ) ;
#4006 = CARTESIAN_POINT ( 'NONE',  ( 1.830559115875370457, 105.1242114329274671, 5.019440104649677714 ) ) ;
#4007 = DIRECTION ( 'NONE',  ( -0.9998004120163608288, 0.000000000000000000, -0.01997839162482750383 ) ) ;
#4008 = CARTESIAN_POINT ( 'NONE',  ( 3.174366308151880478, 101.6934662015457320, 0.06343139340882768262 ) ) ;
#4009 = CARTESIAN_POINT ( 'NONE',  ( 4.462489588987306632, 118.6703996354438289, 1.056833130132613929 ) ) ;
#4010 = EDGE_CURVE ( 'NONE', #19701, #34211, #29900, .T. ) ;
#4011 = CARTESIAN_POINT ( 'NONE',  ( 3.857898856315107761, -6.768822978661375167, 2.551181839177400601 ) ) ;
#4012 = CARTESIAN_POINT ( 'NONE',  ( 22.13959287704968304, 149.5167998366165989, 1.884152790553834889 ) ) ;
#4013 = CARTESIAN_POINT ( 'NONE',  ( -57.94306413390934551, 1.184802614100144424, -1.419326152557812248 ) ) ;
#4015 = CARTESIAN_POINT ( 'NONE',  ( 20.98992760039521954, 147.8517002469272370, -1.565498118541299055 ) ) ;
#4014 = DIRECTION ( 'NONE',  ( 5.188838149069472160E-16, -1.699382548006136559E-16, -1.000000000000000000 ) ) ;
#4016 = CARTESIAN_POINT ( 'NONE',  ( -4.027482788729651375, -0.2968512080594384317, 2.264360808822050597 ) ) ;
#4017 = CARTESIAN_POINT ( 'NONE',  ( -22.70140800483401833, 148.7873826295267747, -1.635989027091524939 ) ) ;
#4018 = ADVANCED_FACE ( 'NONE', ( #1945 ), #11720, .T. ) ;
#4019 = ORIENTED_EDGE ( 'NONE', *, *, #6327, .F. ) ;
#4020 = CARTESIAN_POINT ( 'NONE',  ( -15.72482880707722686, 147.2451778420852406, 0.1375710997406975333 ) ) ;
#4022 = CARTESIAN_POINT ( 'NONE',  ( 5.611355841363750763, -14.32207541480874724, 3.167021961541031327 ) ) ;
#4021 = CIRCLE ( 'NONE', #8781, 8.794749999999993406 ) ;
#4023 = DIRECTION ( 'NONE',  ( -0.8745520943968225769, 0.4849315768086578382, -5.691349986800571545E-16 ) ) ;
#4024 = VERTEX_POINT ( 'NONE', #34730 ) ;
#4025 = CARTESIAN_POINT ( 'NONE',  ( 18.85674122909604833, 149.4003703399637288, 2.492295690319127122 ) ) ;
#4026 = FACE_BOUND ( 'NONE', #29457, .T. ) ;
#4027 = CARTESIAN_POINT ( 'NONE',  ( -17.97610982144389524, 83.97333317030323485, -1.524000000000003130 ) ) ;
#4028 = CARTESIAN_POINT ( 'NONE',  ( -1.339128788961420069, 159.4185946040361728, 0.8255809207588795662 ) ) ;
#4029 = CARTESIAN_POINT ( 'NONE',  ( 4.614102091175348086, 5.327238342305563812, -7.074968232746598140 ) ) ;
#4030 = CARTESIAN_POINT ( 'NONE',  ( 16.45678414710221205, 146.8700648836752691, 1.605370559133788122 ) ) ;
#4031 = CARTESIAN_POINT ( 'NONE',  ( 5.842267051812621403, 117.1711376449269721, -0.3073735213368161689 ) ) ;
#4032 = CARTESIAN_POINT ( 'NONE',  ( 3.009276887026297587, 50.13146620154573441, -1.210121013456480599 ) ) ;
#4033 = CARTESIAN_POINT ( 'NONE',  ( -53.63336534079370921, 9.545430312881217461, 3.611512385389820334 ) ) ;
#4034 = CARTESIAN_POINT ( 'NONE',  ( -47.30609498763488574, 23.90227454495589399, 2.251708124038033443 ) ) ;
#4035 = CARTESIAN_POINT ( 'NONE',  ( 4.755545234561889600, 111.7581959907442268, -2.489084640299535245 ) ) ;
#4036 = CARTESIAN_POINT ( 'NONE',  ( -56.22331024217277928, 5.808995339285999648, 2.850545730341239814 ) ) ;
#4037 = CARTESIAN_POINT ( 'NONE',  ( -56.69685687618531489, 3.834144682062132770, 2.383935162208182579 ) ) ;
#4038 = CARTESIAN_POINT ( 'NONE',  ( -4.515032206727305208, 118.1273750342149640, 0.5013739007068812592 ) ) ;
#4039 = CARTESIAN_POINT ( 'NONE',  ( -58.33591949829837375, -0.2304704932390572170, -0.1444701089452840037 ) ) ;
#4040 = EDGE_CURVE ( 'NONE', #34334, #26787, #18292, .T. ) ;
#4041 = ORIENTED_EDGE ( 'NONE', *, *, #28465, .F. ) ;
#4042 = CARTESIAN_POINT ( 'NONE',  ( -46.91604881613255174, 25.30076613767161220, 1.786867259277511666 ) ) ;
#4043 = AXIS2_PLACEMENT_3D ( 'NONE', #34153, #21332, #10922 ) ;
#4045 = EDGE_CURVE ( 'NONE', #14016, #31005, #4752, .T. ) ;
#4044 = CARTESIAN_POINT ( 'NONE',  ( -6.117143830817480143, 119.5759206346389334, -1.252900237863971089 ) ) ;
#4046 = CARTESIAN_POINT ( 'NONE',  ( -6.914225208283879098, 121.8192184429722005, -0.2944576502256238126 ) ) ;
#4047 = CARTESIAN_POINT ( 'NONE',  ( 4.528603410297228571, 118.1085942879815036, 0.6812181296683174070 ) ) ;
#4048 = CARTESIAN_POINT ( 'NONE',  ( -9.559621201325507300, 153.9312916436033447, -1.179784447169990758 ) ) ;
#4049 = DIRECTION ( 'NONE',  ( -0.9998004120163608288, 0.000000000000000000, -0.01997839162482749342 ) ) ;
#4050 = CARTESIAN_POINT ( 'NONE',  ( 1.584774673591883065, 118.1651004081050473, -0.7984633640959337697 ) ) ;
#4051 = CARTESIAN_POINT ( 'NONE',  ( 7.694720906311244057, 124.7202454748262710, 0.1538800020430352300 ) ) ;
#4052 = CARTESIAN_POINT ( 'NONE',  ( -5.120605266512877840, 120.5246234221128248, -0.8194923670329070653 ) ) ;
#4053 = CARTESIAN_POINT ( 'NONE',  ( 14.39766717389552220, 60.02151067229126369, 1.904999999999990923 ) ) ;
#4054 = DIRECTION ( 'NONE',  ( -5.188838149069472160E-16, 1.699382548006136559E-16, 1.000000000000000000 ) ) ;
#4055 = B_SPLINE_CURVE_WITH_KNOTS ( 'NONE', 3,
 ( #36196, #16146, #22737, #7017, #12191, #29148, #3396, #16362, #29368, #3614, #35562, #10191, #39388, #19985, #33002, #29795 ),
 .UNSPECIFIED., .F., .F.,
 ( 4, 2, 2, 2, 2, 2, 2, 4 ),
 ( 0.000000000000000000, 0.2499999999999863998, 0.3749999999999810152, 0.4374999999999812372, 0.4687499999999821809, 0.4999999999999831246, 0.7499999999999915623, 1.000000000000000000 ),
 .UNSPECIFIED. ) ;
#4056 = CARTESIAN_POINT ( 'NONE',  ( 8.798071512540863282, 117.6842349196870572, 0.1758064070670784795 ) ) ;
#4057 = CARTESIAN_POINT ( 'NONE',  ( -5.939622480684505490, 155.4177107962312903, 0.03793785350558757236 ) ) ;
#4058 = EDGE_CURVE ( 'NONE', #11710, #42131, #8132, .T. ) ;
#4059 = CARTESIAN_POINT ( 'NONE',  ( 4.611808778022512989, -11.57686662695173929, 0.3579861242195471194 ) ) ;
#4060 = CARTESIAN_POINT ( 'NONE',  ( 3.829241263245279026, 116.9593488885201538, 0.4901781634895739370 ) ) ;
#4061 = CARTESIAN_POINT ( 'NONE',  ( -4.085839532347240066, 71.06758511999679229, 1.524000000000005350 ) ) ;
#4062 = CARTESIAN_POINT ( 'NONE',  ( 2.709380901426776678, -15.26748983718428931, 4.527680251005613776 ) ) ;
#4063 = CARTESIAN_POINT ( 'NONE',  ( -15.01676740740995797, 152.9649416503947634, 1.747251348416148042 ) ) ;
#4064 = CARTESIAN_POINT ( 'NONE',  ( -0.2316695588195925026, 0.1309245165040176240, 0.9467938775014126396 ) ) ;
#4065 = CARTESIAN_POINT ( 'NONE',  ( -23.06466230714223897, 149.5685596498530288, -1.055262110361126826 ) ) ;
#4066 = EDGE_CURVE ( 'NONE', #28056, #38820, #24844, .T. ) ;
#4067 = CARTESIAN_POINT ( 'NONE',  ( 0.4358653558703468045, -2.730035452555519271, 0.8728101606764442355 ) ) ;
#4068 = ORIENTED_EDGE ( 'NONE', *, *, #14121, .F. ) ;
#4069 = CARTESIAN_POINT ( 'NONE',  ( -44.16391282238571847, 20.57229585060895616, 1.749602973179248844 ) ) ;
#4070 = CARTESIAN_POINT ( 'NONE',  ( 4.351830713014955165, 111.2795884869231173, 3.127581853150075197 ) ) ;
#4071 = CARTESIAN_POINT ( 'NONE',  ( -9.867693216206411932, 124.1914461168675530, 0.5013480754756758362 ) ) ;
#4072 = CARTESIAN_POINT ( 'NONE',  ( 3.920414950246539298, -14.18668476855415506, 4.724392046630619291 ) ) ;
#4073 = CARTESIAN_POINT ( 'NONE',  ( 13.59099248324865883, 128.5255724691869830, -1.296117023882648933 ) ) ;
#4074 = CARTESIAN_POINT ( 'NONE',  ( -12.00151653869066770, 122.4500365997666336, -1.784698555944021159 ) ) ;
#4075 = EDGE_CURVE ( 'NONE', #23556, #12215, #10162, .T. ) ;
#4076 = CARTESIAN_POINT ( 'NONE',  ( 4.076263842723025554, 104.6144662015457527, 2.604289233363719980 ) ) ;
#4077 = CARTESIAN_POINT ( 'NONE',  ( 2.660183686505937839, -13.21883649654037640, 0.1900507390742080804 ) ) ;
#4078 = CARTESIAN_POINT ( 'NONE',  ( -4.761227440037233194, 117.5395613512557986, -1.175773913404245308 ) ) ;
#4079 = B_SPLINE_CURVE_WITH_KNOTS ( 'NONE', 3,
 ( #8429, #21387, #28009, #27593, #5246, #17580, #41018, #11827, #24815, #27181, #24180, #20982, #1634, #34003, #4833, #30784, #40602, #18841, #41446, #31845, #38667, #22437, #28859, #19048, #35467, #31635, #28226, #21813, #34839, #38457, #6492, #41232, #6085, #6290, #22029, #15437, #9474, #19261, #19470, #35058, #15853, #38871, #41658, #5879, #25460, #12035, #32053, #9064, #2685, #12251, #15642, #2891, #28647, #25864, #18630, #22233, #32269, #2262, #12466, #8849, #28440, #12876, #3099, #5673, #2476, #25244, #38247, #9275, #35261, #41872, #42082, #12671, #25660, #16060, #15225, #29062, #9683, #22649, #35683, #25026, #38029, #19676, #9887, #23283, #30119, #13723, #23709, #26717, #32691, #3526, #121, #36320 ),
 .UNSPECIFIED., .F., .F.,
 ( 4, 2, 2, 2, 2, 2, 1, 1, 2, 2, 2, 2, 2, 2, 2, 2, 2, 1, 1, 2, 2, 2, 2, 1, 1, 2, 2, 2, 1, 2, 2, 1, 1, 2, 2, 2, 1, 1, 1, 2, 2, 2, 2, 2, 2, 2, 1, 1, 1, 1, 2, 2, 2, 4 ),
 ( 0.000000000000000000, 0.03124999999996325856, 0.04687499999994489130, 0.06249999999992653099, 0.09374999999988976873, 0.1093749999998713668, 0.1171874999998621797, 0.1210937499998576000, 0.1230468749998553379, 0.1249999999998530897, 0.1406249999998358813, 0.1484374999998272771, 0.1523437499998230027, 0.1562499999998187006, 0.1718749999998016864, 0.1874999999997846722, 0.2187499999997506162, 0.2343749999997334910, 0.2421874999997249422, 0.2460937499997206401, 0.2499999999997163935, 0.3124999999996500577, 0.3437499999996169175, 0.3593749999996002642, 0.3671874999995919375, 0.3710937499995877187, 0.3749999999995834998, 0.4062499999995490829, 0.4140624999995403122, 0.4160156249995382582, 0.4169921874995372035, 0.4179687499995361488, 0.4218749999995391464, 0.4374999999995509148, 0.4687499999995748956, 0.4843749999995868860, 0.4921874999995928257, 0.4960937499995958788, 0.4980468749995973221, 0.4990234374995980993, 0.4999999999995988764, 0.5624999999996533884, 0.5937499999996804778, 0.6093749999996941336, 0.6249999999997076783, 0.6874999999997625233, 0.7187499999997897238, 0.7343749999998032685, 0.7421874999998098188, 0.7460937499998131495, 0.7480468749998148148, 0.7499999999998164801, 0.8749999999999082956, 1.000000000000000000 ),
 .UNSPECIFIED. ) ;
#4080 = CARTESIAN_POINT ( 'NONE',  ( 1.594039003485483441, 156.2604006213118453, -0.1692965565027964581 ) ) ;
#4081 = AXIS2_PLACEMENT_3D ( 'NONE', #25688, #38693, #9501 ) ;
#4082 = VERTEX_POINT ( 'NONE', #31309 ) ;
#4083 = CARTESIAN_POINT ( 'NONE',  ( -3.070716065586290622, 107.8343606798839573, 4.352802841326662175 ) ) ;
#4084 = CARTESIAN_POINT ( 'NONE',  ( 1.808844889178175208, 106.7498038803831975, 4.947659371736781608 ) ) ;
#4085 = CARTESIAN_POINT ( 'NONE',  ( 1.569820930545707149, 117.3993836205989680, 1.461711849568192889 ) ) ;
#4086 = CARTESIAN_POINT ( 'NONE',  ( -4.394136353581306054, 70.68697878297604120, -1.269999999999994023 ) ) ;
#4087 = CARTESIAN_POINT ( 'NONE',  ( 20.69264154312380555, 152.5691845998198346, 0.2640292844866434230 ) ) ;
#4088 = CARTESIAN_POINT ( 'NONE',  ( -1.586608521453102272, 106.2379067940291293, 5.113598281387616851 ) ) ;
#4089 = CARTESIAN_POINT ( 'NONE',  ( 1.938612655782578242, -15.67376786758054052, 5.527897971745494132 ) ) ;
#4090 = DIRECTION ( 'NONE',  ( -0.8745520943968235761, 0.4849315768086558398, -4.268512490100410909E-16 ) ) ;
#4091 = B_SPLINE_CURVE_WITH_KNOTS ( 'NONE', 3,
 ( #15674, #12908, #29528, #28678, #19084, #32087 ),
 .UNSPECIFIED., .F., .F.,
 ( 4, 2, 4 ),
 ( 0.07978617534960311120, 0.5398930876748015972, 1.000000000000000000 ),
 .UNSPECIFIED. ) ;
#4092 = CARTESIAN_POINT ( 'NONE',  ( 20.26628159282160269, 149.4216517587604756, 2.427422966980313568 ) ) ;
#4093 = ORIENTED_EDGE ( 'NONE', *, *, #29178, .T. ) ;
#4094 = CARTESIAN_POINT ( 'NONE',  ( 6.774419413954826830, 18.20997082500984376, -5.007560425318187569 ) ) ;
#4095 = CARTESIAN_POINT ( 'NONE',  ( 2.286771429912684006, 117.0703292719262691, -0.5337017719177589159 ) ) ;
#4096 = CARTESIAN_POINT ( 'NONE',  ( -0.02009831008155203366, 106.6745790697264056, -5.014625686322316866 ) ) ;
#4097 = CARTESIAN_POINT ( 'NONE',  ( 14.73199999999999754, 12.70000000000000107, 0.000000000000000000 ) ) ;
#4098 = CARTESIAN_POINT ( 'NONE',  ( -10.79307885933853761, 57.10041794475097277, -5.016499999999999737 ) ) ;
#4099 = CARTESIAN_POINT ( 'NONE',  ( -4.383638697405572771, 105.1218378623483858, 3.059989124871295818 ) ) ;
#4100 = CARTESIAN_POINT ( 'NONE',  ( 2.829288187452689396, 6.340478445469713620, 3.655570690059357197 ) ) ;
#4101 = LINE ( 'NONE', #26868, #38056 ) ;
#4102 = CARTESIAN_POINT ( 'NONE',  ( -4.832057687079985620, 118.5264896598256854, 0.7487645382029636254 ) ) ;
#4103 = CARTESIAN_POINT ( 'NONE',  ( 1.848046085800040483, -15.12359198595263088, 5.521975501593071378 ) ) ;
#4104 = CARTESIAN_POINT ( 'NONE',  ( 4.298926901474557916, 118.7880935209305591, -0.4986311761637901574 ) ) ;
#4105 = CARTESIAN_POINT ( 'NONE',  ( -3.184986510633185830, 159.3937097445585778, 0.5650791069852594273 ) ) ;
#4106 = VECTOR ( 'NONE', #12594, 1000.000000000000000 ) ;
#4107 = CARTESIAN_POINT ( 'NONE',  ( 4.923031700297470614, 117.4076359181580216, -0.9493066511862697787 ) ) ;
#4108 = CARTESIAN_POINT ( 'NONE',  ( -36.65473259702431363, 28.27472347546386544, 1.269999999999995577 ) ) ;
#4109 = ORIENTED_EDGE ( 'NONE', *, *, #37792, .T. ) ;
#4110 = CARTESIAN_POINT ( 'NONE',  ( -2.960856320778833872, 31.17411798999470918, 0.6378382452821288462 ) ) ;
#4111 = CARTESIAN_POINT ( 'NONE',  ( 4.858843758304779215, -15.48047902945742749, 1.209346601706016378 ) ) ;
#4112 = CARTESIAN_POINT ( 'NONE',  ( -12.87447296688135090, 155.3440856034525837, 1.681555337288024976 ) ) ;
#4113 = EDGE_CURVE ( 'NONE', #1544, #29870, #2153, .T. ) ;
#4114 = CARTESIAN_POINT ( 'NONE',  ( -3.974385726840726107, -7.478117039488521023, -2.359557994316856533 ) ) ;
#4115 = CARTESIAN_POINT ( 'NONE',  ( -58.61869681968132539, -0.2701152165257065252, -0.4082390686273099090 ) ) ;
#4116 = VERTEX_POINT ( 'NONE', #31524 ) ;
#4117 = DIRECTION ( 'NONE',  ( 4.017660918040594346E-17, -1.000000000000000000, -2.376309959284834438E-19 ) ) ;
#4118 = CARTESIAN_POINT ( 'NONE',  ( -0.06390210066022013191, 106.1446358501009826, 5.228158908302722452 ) ) ;
#4119 = SURFACE_STYLE_USAGE ( .BOTH. , #33289 ) ;
#4120 = CARTESIAN_POINT ( 'NONE',  ( -5.149255372874281811, 120.5246234221128248, 0.6142761105479900285 ) ) ;
#4121 = CARTESIAN_POINT ( 'NONE',  ( -47.85244527695896011, 19.39403540832957518, 5.219971639306693056 ) ) ;
#4122 = CARTESIAN_POINT ( 'NONE',  ( 0.03153862713803012863, 157.4657262375360176, -1.578321868909182246 ) ) ;
#4123 = CARTESIAN_POINT ( 'NONE',  ( -4.699679879531093007, 158.1906701298835856, -1.765476639684187887 ) ) ;
#4124 = DIRECTION ( 'NONE',  ( -0.8745520943968249084, 0.4849315768086534528, -5.361993529360573944E-16 ) ) ;
#4125 = VERTEX_POINT ( 'NONE', #41125 ) ;
#4126 = CARTESIAN_POINT ( 'NONE',  ( 4.162481684639020685, 118.2393836468389594, -0.2285641109998220177 ) ) ;
#4127 = CARTESIAN_POINT ( 'NONE',  ( 7.092669859378088582, 121.9239394581621809, -0.2697480494961534969 ) ) ;
#4128 = VERTEX_POINT ( 'NONE', #11931 ) ;
#4129 = CARTESIAN_POINT ( 'NONE',  ( 3.231433726605559276, -14.53588044659766254, 1.883291753459793716 ) ) ;
#4130 = AXIS2_PLACEMENT_3D ( 'NONE', #20440, #3874, #33467 ) ;
#4131 = CARTESIAN_POINT ( 'NONE',  ( -6.507153519498132566E-14, 76.29346620154572634, 3.067795752821199360E-29 ) ) ;
#4132 = CARTESIAN_POINT ( 'NONE',  ( -50.01754050905309867, 16.20622680600125420, 4.878148848498067736 ) ) ;
#4133 = CARTESIAN_POINT ( 'NONE',  ( 4.506137822554599381, 3.376467715207942533, 1.027655576270160243 ) ) ;
#4134 = CARTESIAN_POINT ( 'NONE',  ( 10.79132569999976177, 123.6843197456346672, 1.443847663909934464 ) ) ;
#4135 = CARTESIAN_POINT ( 'NONE',  ( -2.677528989280510086, 30.35663814294097307, 0.2735905739161426098 ) ) ;
#4136 = CARTESIAN_POINT ( 'NONE',  ( -1.932895124392534303, 20.38400505531995321, -4.219463811995566083 ) ) ;
#4137 = CARTESIAN_POINT ( 'NONE',  ( 15.65552799280926699, 147.2250547476223801, 0.5422809309331375616 ) ) ;
#4138 = DIRECTION ( 'NONE',  ( -0.9876665170007969952, 0.1565721916417935344, -5.390917751951444915E-16 ) ) ;
#4139 = CARTESIAN_POINT ( 'NONE',  ( -51.42025106686629243, 13.11195823927271320, -3.453838694686346855 ) ) ;
#4140 = CARTESIAN_POINT ( 'NONE',  ( -8.792159704875166071, 117.7003605453419084, -0.3061736163580975334 ) ) ;
#4141 = LINE ( 'NONE', #23480, #39367 ) ;
#4142 = CARTESIAN_POINT ( 'NONE',  ( -4.476425760464393555, 71.61790547347303004, -1.269999999999994245 ) ) ;
#4143 = CARTESIAN_POINT ( 'NONE',  ( -31.37023363772181028, 53.64958092169537451, -1.270000000000005125 ) ) ;
#4144 = CARTESIAN_POINT ( 'NONE',  ( -30.60466991297690242, 55.37784481745784149, -1.524000000000004906 ) ) ;
#4145 = VECTOR ( 'NONE', #25826, 1000.000000000000114 ) ;
#4146 = CARTESIAN_POINT ( 'NONE',  ( -6.059261036834497460, 77.01756250000002524, 5.016499999999999737 ) ) ;
#4147 = DIRECTION ( 'NONE',  ( -0.9998004120163609398, 0.000000000000000000, -0.01997839162482749689 ) ) ;
#4148 = CARTESIAN_POINT ( 'NONE',  ( -57.78461401849435930, 2.885363594410716992, 0.1114619696582708486 ) ) ;
#4149 = CARTESIAN_POINT ( 'NONE',  ( -58.43690671596436914, -0.4125963578781866037, -1.035377653829272970E-14 ) ) ;
#4150 = CARTESIAN_POINT ( 'NONE',  ( -16.05353943441306441, 121.3766923467913585, 0.004207837007976961835 ) ) ;
#4151 = EDGE_LOOP ( 'NONE', ( #15825, #14704, #7546, #13311 ) ) ;
#4152 = CARTESIAN_POINT ( 'NONE',  ( -56.22979136716762838, 7.596919248368375399, -0.4408371032393147426 ) ) ;
#4153 = CARTESIAN_POINT ( 'NONE',  ( -6.060908664785462641, 121.4331619493032832, -0.1231561192607217164 ) ) ;
#4154 = ORIENTED_EDGE ( 'NONE', *, *, #39143, .T. ) ;
#4155 = CARTESIAN_POINT ( 'NONE',  ( 11.58677707360137532, 17.14499999999999957, 4.474811398758258285 ) ) ;
#4157 = CARTESIAN_POINT ( 'NONE',  ( -14.67688973683561571, 148.8424012017631242, -0.4203365054377472543 ) ) ;
#4156 = AXIS2_PLACEMENT_3D ( 'NONE', #20648, #30879, #4712 ) ;
#4158 = CARTESIAN_POINT ( 'NONE',  ( 3.642312988314884592, -15.20939988557298861, 5.384177138096517545 ) ) ;
#4159 = CARTESIAN_POINT ( 'NONE',  ( -16.85638304633373252, 153.6818489539412553, 1.479736204719018122 ) ) ;
#4160 = CARTESIAN_POINT ( 'NONE',  ( 0.4746723515649934888, 24.68197512780947278, 4.609222710213416896 ) ) ;
#4161 = CARTESIAN_POINT ( 'NONE',  ( 15.47334368943519500, 120.8153160915142337, 0.6283931236857892566 ) ) ;
#4162 = CARTESIAN_POINT ( 'NONE',  ( 2.249953683904569957, -15.41150387077881767, 5.858494404600263827 ) ) ;
#4163 = CARTESIAN_POINT ( 'NONE',  ( 1.790774717077139089, 25.13178105314743860, 4.274281468382033822 ) ) ;
#4164 = CARTESIAN_POINT ( 'NONE',  ( -0.7070771686734943495, -4.675651901196332005, 0.6724949525944122763 ) ) ;
#4165 = CARTESIAN_POINT ( 'NONE',  ( -13.39999158873821195, 156.9487217736090940, -0.4592210153261409578 ) ) ;
#4166 = DIRECTION ( 'NONE',  ( -5.206863593109713661E-17, 1.000000000000000000, -1.077750396879097183E-30 ) ) ;
#4167 = CARTESIAN_POINT ( 'NONE',  ( 4.812227470261317919, 117.4055065471341237, 1.197252064078428990 ) ) ;
#4168 = ORIENTED_EDGE ( 'NONE', *, *, #36999, .F. ) ;
#4169 = CARTESIAN_POINT ( 'NONE',  ( -8.791734470649634758, 117.7397621763150966, 0.07689045645447853405 ) ) ;
#4170 = CARTESIAN_POINT ( 'NONE',  ( -9.495682976374393292, 155.1592096034013366, 1.579384785498887167 ) ) ;
#4171 = CARTESIAN_POINT ( 'NONE',  ( -57.85400989612196554, 0.8207036343174740622, -1.039311302907389933 ) ) ;
#4172 = CARTESIAN_POINT ( 'NONE',  ( 5.844449987888563847, 118.2031694463412634, 1.045635565433329583 ) ) ;
#4173 = CARTESIAN_POINT ( 'NONE',  ( 16.79779972313707859, 131.5287050380659082, -1.642352026799754450 ) ) ;
#4174 = CARTESIAN_POINT ( 'NONE',  ( -0.9740112296533943725, -11.51769927068266419, -0.01433540041261589619 ) ) ;
#4175 = CARTESIAN_POINT ( 'NONE',  ( -3.973247942572257330, 117.7793252414215317, -0.8392447889045229203 ) ) ;
#4176 = CARTESIAN_POINT ( 'NONE',  ( -44.40534991575952972, 23.82367036525651116, -1.730788704199199834 ) ) ;
#4177 = CARTESIAN_POINT ( 'NONE',  ( 4.832410959468069755, 104.6144662015479412, 2.264944922177924536 ) ) ;
#4178 = CARTESIAN_POINT ( 'NONE',  ( 16.50777979357271263, 146.8700648836752691, -0.9466601202970253981 ) ) ;
#4179 = DIRECTION ( 'NONE',  ( 1.224646799147353207E-16, -1.179012811983454535E-32, 1.000000000000000000 ) ) ;
#4180 = ORIENTED_EDGE ( 'NONE', *, *, #6820, .F. ) ;
#4181 = CARTESIAN_POINT ( 'NONE',  ( -5.835067757121142229, 120.0568572605186546, -1.100767069290504718 ) ) ;
#4182 = CARTESIAN_POINT ( 'NONE',  ( 5.161689517976459030, -15.45231451347503437, 1.550260198497607877 ) ) ;
#4183 =( BOUNDED_CURVE ( )  B_SPLINE_CURVE ( 3, ( #268, #2834, #22798, #22379 ),
 .UNSPECIFIED., .F., .T. ) 
 B_SPLINE_CURVE_WITH_KNOTS ( ( 4, 4 ),
 ( 1.570796326794897446, 3.141592653589792672 ),
 .UNSPECIFIED. ) 
 CURVE ( )  GEOMETRIC_REPRESENTATION_ITEM ( )  RATIONAL_B_SPLINE_CURVE ( ( 1.000000000000000000, 0.8047378541243652705, 0.8047378541243652705, 1.000000000000000000 ) ) 
 REPRESENTATION_ITEM ( '' )  );
#4184 = CARTESIAN_POINT ( 'NONE',  ( -4.801770124281918406, 117.3993836135855133, 1.016061139389656587 ) ) ;
#4185 = CARTESIAN_POINT ( 'NONE',  ( -4.708247763567237953, 117.9524266585390677, -0.8424022261019792346 ) ) ;
#4186 = VECTOR ( 'NONE', #29664, 1000.000000000000000 ) ;
#4187 = CARTESIAN_POINT ( 'NONE',  ( -48.98489377192316852, 18.65252824715059177, -5.272350768541925525 ) ) ;
#4188 = DIRECTION ( 'NONE',  ( -0.9998004120163608288, 0.000000000000000000, -0.01997839162482749342 ) ) ;
#4189 = B_SPLINE_SURFACE_WITH_KNOTS ( 'NONE', 3, 3, ( 
 ( #28254, #41259, #38058, #8876, #34867 ),
 ( #5699, #15466, #28469, #3125, #29092 ),
 ( #41899, #19080, #42110, #12699, #6522 ),
 ( #9714, #35499, #36138, #26318, #38902 ),
 ( #16728, #16517, #39325, #19497, #29524 ),
 ( #9502, #2919, #12905, #3769, #38694 ),
 ( #6954, #15881, #22263, #16086, #10131 ),
 ( #38484, #26110, #25689, #25894, #32508 ),
 ( #22680, #29732, #13546, #28887, #364 ),
 ( #13119, #13330, #39115, #22468, #572 ),
 ( #23104, #35714, #6318, #151, #19923 ),
 ( #9302, #32939, #35287, #19291, #6115 ),
 ( #32084, #32296, #9920, #3338, #16306 ),
 ( #29308, #6737, #22890, #32725, #35927 ),
 ( #19708, #3558, #4404, #4187, #33356 ),
 ( #17149, #36971, #29939, #36552, #20754 ),
 ( #778, #10555, #30150, #7371, #39967 ),
 ( #23953, #10968, #40174, #14157, #3980 ),
 ( #26537, #30563, #20127, #7168, #30348 ),
 ( #1403, #16940, #7793, #11176, #33779 ),
 ( #37170, #23317, #39760, #33152, #4811 ),
 ( #4606, #27371, #10759, #26750, #1197 ),
 ( #992, #23524, #13956, #24161, #33570 ),
 ( #7579, #17562, #26954, #14359, #20330 ),
 ( #36354, #23740, #40381, #36761, #7993 ),
 ( #20962, #30762, #33983, #17764, #27161 ),
 ( #1613, #20540, #17361, #39542, #13754 ),
 ( #10347, #14570, #30975, #40790, #34393 ),
 ( #27990, #12229, #12012, #41211, #28203 ),
 ( #5650, #34192, #5017, #14989, #27778 ),
 ( #1815, #17978, #31399, #14778, #11590 ),
 ( #18180, #21160, #40997, #35037, #37374 ),
 ( #40583, #15413, #24573, #15200, #8406 ),
 ( #38007, #25220, #37578, #5432, #11802 ),
 ( #5226, #24792, #21366, #8191, #31182 ),
 ( #37788, #2023, #8615, #21577, #38225 ),
 ( #34604, #18389, #5857, #34816, #28417 ),
 ( #18607, #2452, #2241, #25007, #8828 ),
 ( #21789, #31613, #9040, #41423, #11380 ) ),
 .UNSPECIFIED., .F., .F., .F.,
 ( 4, 1, 1, 1, 1, 1, 1, 1, 1, 1, 1, 2, 1, 1, 1, 1, 1, 1, 1, 1, 1, 1, 1, 1, 1, 1, 1, 1, 1, 1, 1, 1, 1, 1, 1, 4 ),
 ( 4, 1, 4 ),
 ( 0.000000000000000000, 0.01653533301974152367, 0.03307066603948304734, 0.04960599905922460223, 0.06614133207896609468, 0.08267666509870763569, 0.09921199811844919059, 0.1322826641579321894, 0.1653533301974152714, 0.1984239962368983812, 0.2314946622763813522, 0.2645653283158643787, 0.3105299952961229071, 0.3335123287862520880, 0.3564946622763812689, 0.4024593292566397418, 0.4484239962368982702, 0.4943886632171566875, 0.5403533301974150493, 0.5863179971776735222, 0.6322826641579321061, 0.6782473311381906900, 0.7242119981184491628, 0.7701766650987074136, 0.8161413320789658865, 0.8621059990592241373, 0.8735971658042887000, 0.8850883325493537068, 0.8965794992944182695, 0.9080706660394826102, 0.9195618327845473949, 0.9310529995296121797, 0.9425441662746769644, 0.9540353330197415271, 0.9770176665098706525, 1.000000000000000000 ),
 ( 0.000000000000000000, 0.5000000000000000000, 1.000000000000000000 ),
 .UNSPECIFIED. ) ;
#4190 = CARTESIAN_POINT ( 'NONE',  ( 13.11083847086517906, 125.9194590699508893, 1.866409529942264944 ) ) ;
#4191 = FACE_OUTER_BOUND ( 'NONE', #25863, .T. ) ;
#4192 = CIRCLE ( 'NONE', #8264, 0.5080000000000002292 ) ;
#4193 = CARTESIAN_POINT ( 'NONE',  ( 16.30362368704338394, 121.4145675751456253, 0.3085868453551565693 ) ) ;
#4194 = CARTESIAN_POINT ( 'NONE',  ( -3.339872139798120809, 10.66371166075841437, -7.743087711851694088 ) ) ;
#4195 = CARTESIAN_POINT ( 'NONE',  ( 7.064669522240043520, 121.9740017686541194, 0.4795729057185784128 ) ) ;
#4196 = CARTESIAN_POINT ( 'NONE',  ( 1.996658253870856381, 117.0827246868714013, -0.4092875891974778746 ) ) ;
#4197 = CARTESIAN_POINT ( 'NONE',  ( -46.76714659696671106, 20.35889133747131652, -4.890039387021453798 ) ) ;
#4198 = FACE_OUTER_BOUND ( 'NONE', #24679, .T. ) ;
#4199 = CARTESIAN_POINT ( 'NONE',  ( -15.69674027099064340, 120.8333755831694702, -0.2629491152481263083 ) ) ;
#4200 = ORIENTED_EDGE ( 'NONE', *, *, #26140, .T. ) ;
#4201 = CARTESIAN_POINT ( 'NONE',  ( -8.075719299406451057, 121.0962356888206983, -1.310857334151179998 ) ) ;
#4202 = DIRECTION ( 'NONE',  ( -5.188838149069471174E-16, 1.699382548006136313E-16, 1.000000000000000000 ) ) ;
#4203 = ORIENTED_EDGE ( 'NONE', *, *, #12647, .F. ) ;
#4204 = DIRECTION ( 'NONE',  ( 0.9998004120163608288, 0.000000000000000000, 0.01997839162482749342 ) ) ;
#4205 = CARTESIAN_POINT ( 'NONE',  ( -15.32065199451917437, 143.5038931315047535, -0.7650733020788531569 ) ) ;
#4206 = CARTESIAN_POINT ( 'NONE',  ( 4.513689648792266418, -13.57929909251434708, 3.776549439516510898 ) ) ;
#4207 = CARTESIAN_POINT ( 'NONE',  ( -14.39601482975368008, 155.9958976045614349, 1.017949466214369325 ) ) ;
#4208 = CARTESIAN_POINT ( 'NONE',  ( -5.177913976931298734, 78.94499979771843812, -5.372100000000003206 ) ) ;
#4209 = AXIS2_PLACEMENT_3D ( 'NONE', #17944, #37548, #39927 ) ;
#4210 = CARTESIAN_POINT ( 'NONE',  ( 1.814945173922627442, 116.4909138135563040, 0.1082358691141157847 ) ) ;
#4211 = EDGE_CURVE ( 'NONE', #1598, #40883, #9091, .T. ) ;
#4212 = VERTEX_POINT ( 'NONE', #19564 ) ;
#4213 = CARTESIAN_POINT ( 'NONE',  ( 0.4343283552818534288, -9.202337043772711667, -4.603842121470758997 ) ) ;
#4214 = ADVANCED_FACE ( 'NONE', ( #31949 ), #32794, .F. ) ;
#4215 = CARTESIAN_POINT ( 'NONE',  ( -23.29064488658028864, 149.3519930085110161, -0.4911336289882582418 ) ) ;
#4216 = CARTESIAN_POINT ( 'NONE',  ( -11.34554992887676228, 77.73165686004496422, -1.269999999999998685 ) ) ;
#4217 = DIRECTION ( 'NONE',  ( 0.1469470846586743984, 9.335746474409589170E-17, 0.9891443546370349837 ) ) ;
#4218 = ORIENTED_EDGE ( 'NONE', *, *, #33196, .T. ) ;
#4219 = CARTESIAN_POINT ( 'NONE',  ( 6.579380666976237357, 119.9434534851795462, 1.241007387725648892 ) ) ;
#4220 = CARTESIAN_POINT ( 'NONE',  ( -0.4757704999385121702, -3.320450887815510121, -4.596079559024887295 ) ) ;
#4221 = CARTESIAN_POINT ( 'NONE',  ( 4.857111322523725683, 117.4312795728108227, 0.7492135168955068592 ) ) ;
#4222 = CARTESIAN_POINT ( 'NONE',  ( -57.79605042197182030, 0.9991760233560177396, -1.356629168144531494 ) ) ;
#4224 = CARTESIAN_POINT ( 'NONE',  ( 20.96550312372659519, 148.3608207065297222, -1.563628808460498565 ) ) ;
#4223 = CARTESIAN_POINT ( 'NONE',  ( -24.24369025645184905, 82.02711331519694227, -1.524000000000006239 ) ) ;
#4225 = AXIS2_PLACEMENT_3D ( 'NONE', #13379, #38740, #25939 ) ;
#4226 = CARTESIAN_POINT ( 'NONE',  ( 0.9983407785579379023, 1.652274601622760741, 4.518288805521794238 ) ) ;
#4227 = CARTESIAN_POINT ( 'NONE',  ( -20.32146383345317275, 132.1502320877631007, -1.598207211936853334 ) ) ;
#4228 = ORIENTED_EDGE ( 'NONE', *, *, #36531, .T. ) ;
#4229 = CARTESIAN_POINT ( 'NONE',  ( -0.6357087519303221690, 120.9405031987692212, 0.07870476970620013391 ) ) ;
#4230 = CARTESIAN_POINT ( 'NONE',  ( 3.642312988314884592, -15.20939988557298861, 5.384177138096517545 ) ) ;
#4231 = DIRECTION ( 'NONE',  ( -5.188838149069471174E-16, 1.699382548006136313E-16, 1.000000000000000000 ) ) ;
#4232 = CARTESIAN_POINT ( 'NONE',  ( -4.258558535336168127, 112.0482830817686590, -2.856570678809109864 ) ) ;
#4233 = VERTEX_POINT ( 'NONE', #16590 ) ;
#4234 = CARTESIAN_POINT ( 'NONE',  ( 4.389113801267265025, 157.7533977378147654, 1.847790720561485633 ) ) ;
#4235 = FACE_OUTER_BOUND ( 'NONE', #12298, .T. ) ;
#4236 = DIRECTION ( 'NONE',  ( 4.017660918040594346E-17, -1.000000000000000000, -2.376309959284834438E-19 ) ) ;
#4237 = AXIS2_PLACEMENT_3D ( 'NONE', #15053, #24862, #37858 ) ;
#4238 = CARTESIAN_POINT ( 'NONE',  ( -1.044861395164040196, 117.1967307433898640, 0.4172573962433457906 ) ) ;
#4240 = EDGE_CURVE ( 'NONE', #23948, #24265, #1340, .T. ) ;
#4239 = CARTESIAN_POINT ( 'NONE',  ( 2.011605530963595623, 11.37297026005182587, 8.215081034461865883 ) ) ;
#4241 = CARTESIAN_POINT ( 'NONE',  ( 4.434842451389386930, 120.7762672505206041, 0.5587804529453967994 ) ) ;
#4242 = DIRECTION ( 'NONE',  ( -0.3256999990547897461, -0.9454731675810318370, 0.000000000000000000 ) ) ;
#4243 = CARTESIAN_POINT ( 'NONE',  ( 16.81386451639889756, 122.6968688451475771, -0.2091777910580984723 ) ) ;
#4244 = CARTESIAN_POINT ( 'NONE',  ( -14.39766717389551864, 60.87500489999898434, -1.904999999999999583 ) ) ;
#4245 = CARTESIAN_POINT ( 'NONE',  ( -52.59820521890329559, 11.53769016215144916, 4.012948236587642548 ) ) ;
#4246 = CARTESIAN_POINT ( 'NONE',  ( -49.18322560636019602, 21.37428572888716616, 2.217132718382739398 ) ) ;
#4247 = CARTESIAN_POINT ( 'NONE',  ( 5.211496251797417933, 114.7155965213235334, -1.248716016855044852 ) ) ;
#4248 = CARTESIAN_POINT ( 'NONE',  ( -54.12303657725384198, 9.464413707472848714, 3.807237671326749506 ) ) ;
#4249 = CARTESIAN_POINT ( 'NONE',  ( -58.48165732182965115, 0.01964004061440082285, 0.7222573681096682296 ) ) ;
#4250 = CARTESIAN_POINT ( 'NONE',  ( -4.525247824673359176, 118.1239580192302157, 0.4884167081844107416 ) ) ;
#4251 = CARTESIAN_POINT ( 'NONE',  ( 2.790246638979534843, 107.7056043231319364, -4.425809011598065723 ) ) ;
#4252 = VERTEX_POINT ( 'NONE', #15745 ) ;
#4253 = CARTESIAN_POINT ( 'NONE',  ( -42.33919149967392315, 22.05006338260229271, 1.842566675324087022 ) ) ;
#4254 = TOROIDAL_SURFACE ( 'NONE', #9666, 0.7620000000000000107, 0.2540000000000000036 ) ;
#4255 = CARTESIAN_POINT ( 'NONE',  ( -3.910367129306138168, 119.0646914673601060, -0.9244502089851933668 ) ) ;
#4256 = CARTESIAN_POINT ( 'NONE',  ( -5.487604538598444215, 117.4962825466697467, -0.8290304003371101738 ) ) ;
#4257 = CARTESIAN_POINT ( 'NONE',  ( 4.563865627759259525, 118.0172877987257891, 0.8781525176551367995 ) ) ;
#4258 = CARTESIAN_POINT ( 'NONE',  ( -16.21957319403762554, 147.1082353761072454, -1.436993664011566807 ) ) ;
#4259 = CARTESIAN_POINT ( 'NONE',  ( -0.5747239345953479850, 115.7029522507744446, -1.760667902980975086 ) ) ;
#4260 = CARTESIAN_POINT ( 'NONE',  ( 0.5167143258659047111, 118.1651003012477048, -0.8730464947480743865 ) ) ;
#4261 = CARTESIAN_POINT ( 'NONE',  ( 6.150459292200123329, 119.5049778551863682, -0.2724401547530461709 ) ) ;
#4262 = CARTESIAN_POINT ( 'NONE',  ( -1.860601238663146084, 156.5995568990359175, -1.190227115183317474 ) ) ;
#4263 = DIRECTION ( 'NONE',  ( 1.000000000000000000, 0.000000000000000000, 1.224646799147353454E-16 ) ) ;
#4264 = DIRECTION ( 'NONE',  ( -0.01731298258488073172, 0.9998501190848634312, -1.788962107505278366E-16 ) ) ;
#4265 = CARTESIAN_POINT ( 'NONE',  ( 8.378245210821091860, 119.8566484287663343, -1.107698278211587617 ) ) ;
#4266 = FACE_OUTER_BOUND ( 'NONE', #1434, .T. ) ;
#4267 = DIRECTION ( 'NONE',  ( 0.01997839162482749689, 1.040247600000945640E-18, -0.9998004120163610509 ) ) ;
#4268 = CARTESIAN_POINT ( 'NONE',  ( 22.87667167544107372, 149.1739538623130272, 1.428090254611251719 ) ) ;
#4269 = FACE_OUTER_BOUND ( 'NONE', #40486, .T. ) ;
#4270 = CARTESIAN_POINT ( 'NONE',  ( 2.484037338616324142, -15.29988040857715959, 4.804498879097399033 ) ) ;
#4271 = CARTESIAN_POINT ( 'NONE',  ( -0.03153862713815891450, 157.4657262375360176, 1.578321868909182690 ) ) ;
#4272 = CARTESIAN_POINT ( 'NONE',  ( -0.6899137464274212039, -3.097154947502566813, -0.6881565663087282347 ) ) ;
#4273 = CARTESIAN_POINT ( 'NONE',  ( -23.25105004451273416, 146.7258352529021863, -1.066525923017375588 ) ) ;
#4274 = AXIS2_PLACEMENT_3D ( 'NONE', #25349, #34731, #41126 ) ;
#4275 = CARTESIAN_POINT ( 'NONE',  ( -0.6564745402265276253, 25.61689014148909393, -0.7196881648562951650 ) ) ;
#4276 = ORIENTED_EDGE ( 'NONE', *, *, #30098, .T. ) ;
#4277 = EDGE_CURVE ( 'NONE', #6546, #33508, #41967, .T. ) ;
#4278 = CARTESIAN_POINT ( 'NONE',  ( -53.95448410595108157, 8.335714161839828051, 2.220323970834196636 ) ) ;
#4279 = CARTESIAN_POINT ( 'NONE',  ( 5.553235467069344011, 117.9513286348681476, 0.7459228754688892460 ) ) ;
#4280 = CARTESIAN_POINT ( 'NONE',  ( -4.488166000884779905, 120.9326014760084007, 0.2785428184686808417 ) ) ;
#4281 = CARTESIAN_POINT ( 'NONE',  ( 4.246535372682106235, -13.89508586689386327, 4.277860383763752772 ) ) ;
#4282 = CARTESIAN_POINT ( 'NONE',  ( 0.5497817020642016272, 119.7690751942239729, -0.4902208388216631740 ) ) ;
#4283 = VERTEX_POINT ( 'NONE', #29598 ) ;
#4284 = CARTESIAN_POINT ( 'NONE',  ( -4.155191945500765094, 119.0775769483117870, -1.003333751211267666 ) ) ;
#4285 = CARTESIAN_POINT ( 'NONE',  ( 3.782349093391025541, 115.7032132741988590, 1.604868649576247641 ) ) ;
#4286 = CARTESIAN_POINT ( 'NONE',  ( 3.187349844189338199, -14.38168857376666310, 3.261415970826748278 ) ) ;
#4287 = CARTESIAN_POINT ( 'NONE',  ( -4.973571103949897321, 117.3993852294894822, -0.9750599430652935329 ) ) ;
#4288 = CARTESIAN_POINT ( 'NONE',  ( 0.6357087519301933831, 120.9405031987692212, -0.07870476970620002288 ) ) ;
#4289 = AXIS2_PLACEMENT_3D ( 'NONE', #28583, #41, #12185 ) ;
#4290 = ORIENTED_EDGE ( 'NONE', *, *, #17204, .T. ) ;
#4291 = EDGE_CURVE ( 'NONE', #2129, #6380, #3405, .T. ) ;
#4292 = DIRECTION ( 'NONE',  ( -5.206863593109713661E-17, 1.000000000000000000, -1.077750396879097183E-30 ) ) ;
#4293 = CARTESIAN_POINT ( 'NONE',  ( 4.730923123951279230, 114.9758604107125848, 1.767004453122148711 ) ) ;
#4294 = DIRECTION ( 'NONE',  ( 0.000000000000000000, 1.000000000000000000, 0.000000000000000000 ) ) ;
#4295 = CARTESIAN_POINT ( 'NONE',  ( -6.135835944515187101, 77.40800365160224317, -1.269999999999996243 ) ) ;
#4296 = CARTESIAN_POINT ( 'NONE',  ( 11.68775717287289773, 118.7263634577040676, 0.08842886322950112288 ) ) ;
#4297 = EDGE_CURVE ( 'NONE', #5344, #4652, #5545, .T. ) ;
#4298 = DIRECTION ( 'NONE',  ( -5.188838149069471174E-16, 1.699382548006136313E-16, 1.000000000000000000 ) ) ;
#4299 = CIRCLE ( 'NONE', #6998, 0.5080000000000002292 ) ;
#4300 = ADVANCED_FACE ( 'NONE', ( #28750 ), #41763, .T. ) ;
#4301 = CARTESIAN_POINT ( 'NONE',  ( 1.981454933681730202, -15.19403129753971271, 5.950052743700623203 ) ) ;
#4302 = CARTESIAN_POINT ( 'NONE',  ( 11.47253659098475076, 56.76836532675937974, 5.016499999999999737 ) ) ;
#4303 = CARTESIAN_POINT ( 'NONE',  ( -2.317791448294674428, 31.60761946039689718, 1.124105164688197211 ) ) ;
#4304 = CARTESIAN_POINT ( 'NONE',  ( 11.41340492329610434, 156.2473422840488979, 2.091747920666957139 ) ) ;
#4305 = VERTEX_POINT ( 'NONE', #16156 ) ;
#4306 = CARTESIAN_POINT ( 'NONE',  ( 8.244768260990875675, 16.90678017261275556, 1.796629206788997513 ) ) ;
#4307 = CARTESIAN_POINT ( 'NONE',  ( 2.257211396292739369, 116.9995425702703926, -0.5090954389876272135 ) ) ;
#4308 = CARTESIAN_POINT ( 'NONE',  ( -0.05023876518796718121, 106.0087397856094356, -5.285590276201098447 ) ) ;
#4309 = CARTESIAN_POINT ( 'NONE',  ( -5.600204413207901410, 78.91171765783740000, 5.075433163388495039 ) ) ;
#4310 = CARTESIAN_POINT ( 'NONE',  ( -2.116593079194864835, 107.0582647851741882, -4.811305763238920008 ) ) ;
#4311 = CARTESIAN_POINT ( 'NONE',  ( -5.284023326239697838, 104.6144662015015143, 0.8090710649176173774 ) ) ;
#4312 = CIRCLE ( 'NONE', #28090, 0.5080000000000004512 ) ;
#4313 = CARTESIAN_POINT ( 'NONE',  ( -2.406711483539481389, 4.503775517365914638, 3.979180414515509412 ) ) ;
#4314 = FACE_OUTER_BOUND ( 'NONE', #38588, .T. ) ;
#4315 = CARTESIAN_POINT ( 'NONE',  ( -4.402866250424960270, 110.7917892407665050, -3.073120133393222098 ) ) ;
#4316 = CARTESIAN_POINT ( 'NONE',  ( 3.089232434235547942, -13.39873834325867819, 1.372807258641574935 ) ) ;
#4317 = CARTESIAN_POINT ( 'NONE',  ( 3.258544586981714453, 118.6786177306206014, -0.6136036933997358611 ) ) ;
#4318 = CARTESIAN_POINT ( 'NONE',  ( -14.85158921512566721, 156.1223461918646933, 0.5575614454322269653 ) ) ;
#4319 = EDGE_CURVE ( 'NONE', #21156, #35348, #38351, .T. ) ;
#4320 = CARTESIAN_POINT ( 'NONE',  ( -3.933769473788126803, 27.98561731294367050, 0.4889718192695882149 ) ) ;
#4321 = CARTESIAN_POINT ( 'NONE',  ( -5.348924234571056147, 56.51499999999999346, 4.492130288940740179 ) ) ;
#4322 = ORIENTED_EDGE ( 'NONE', *, *, #35707, .F. ) ;
#4323 = CARTESIAN_POINT ( 'NONE',  ( -4.779485535544667485, 104.6144662015457811, -0.6866870093448155243 ) ) ;
#4324 = CARTESIAN_POINT ( 'NONE',  ( 3.609959606426583978, -15.77075149864894144, 4.467226954163184161 ) ) ;
#4325 = CARTESIAN_POINT ( 'NONE',  ( -0.01133701039344079536, 118.4098733054621277, 0.5673503590873754110 ) ) ;
#4326 = CARTESIAN_POINT ( 'NONE',  ( -0.4908008364610317309, 30.95719094559541418, -0.8433761395939078920 ) ) ;
#4327 = ORIENTED_EDGE ( 'NONE', *, *, #19041, .F. ) ;
#4328 = CARTESIAN_POINT ( 'NONE',  ( -25.80936006922821591, 73.72935646344811289, -1.524000000000005794 ) ) ;
#4329 = CARTESIAN_POINT ( 'NONE',  ( 0.8061429914041100542, 121.2007779179981384, 0.4207382890248005936 ) ) ;
#4330 = CARTESIAN_POINT ( 'NONE',  ( -4.378102236263193170, 120.3584862571861436, 0.5730137456143139518 ) ) ;
#4331 = FACE_OUTER_BOUND ( 'NONE', #8085, .T. ) ;
#4332 = CARTESIAN_POINT ( 'NONE',  ( 13.41341228195535784, 125.8771108566470502, -1.381187796596252459 ) ) ;
#4333 = AXIS2_PLACEMENT_3D ( 'NONE', #2314, #27644, #40863 ) ;
#4334 = CARTESIAN_POINT ( 'NONE',  ( -5.842949248259256656, 118.5625182843610617, -1.130067629703343624 ) ) ;
#4335 = CARTESIAN_POINT ( 'NONE',  ( -26.37263903973852663, 72.23735686029533554, 1.269999999999993356 ) ) ;
#4336 = EDGE_LOOP ( 'NONE', ( #26135, #10096, #5482, #24627 ) ) ;
#4337 = CARTESIAN_POINT ( 'NONE',  ( 4.244956071762963745, 118.2245432729572627, -0.3158671543450045638 ) ) ;
#4338 = EDGE_CURVE ( 'NONE', #39389, #42027, #14224, .T. ) ;
#4339 = AXIS2_PLACEMENT_3D ( 'NONE', #3810, #616, #7210 ) ;
#4340 = CARTESIAN_POINT ( 'NONE',  ( 6.495086324197963279, 121.6155390319085683, -0.2579311815284315856 ) ) ;
#4341 = EDGE_CURVE ( 'NONE', #37188, #3374, #27167, .T. ) ;
#4342 = EDGE_LOOP ( 'NONE', ( #33538, #12154, #24889, #37628 ) ) ;
#4343 = CARTESIAN_POINT ( 'NONE',  ( 3.351397644842732948, -15.05179984492975542, 2.935234935891222641 ) ) ;
#4344 = CARTESIAN_POINT ( 'NONE',  ( 10.28897677580358128, 56.51500000000000057, -4.381500000000000838 ) ) ;
#4345 = VECTOR ( 'NONE', #40855, 1000.000000000000227 ) ;
#4346 = DIRECTION ( 'NONE',  ( -0.9998004120163608288, 0.000000000000000000, -0.01997839162482747608 ) ) ;
#4347 = CARTESIAN_POINT ( 'NONE',  ( 0.7003524534433175353, 11.14785949628657669, 4.567531960304466843 ) ) ;
#4348 = CARTESIAN_POINT ( 'NONE',  ( 11.67499187284218820, 153.3684197651487580, 1.838730530730912083 ) ) ;
#4349 = CARTESIAN_POINT ( 'NONE',  ( -2.644846971204092068, 29.87439188816612656, 0.9757876149222759476 ) ) ;
#4350 = EDGE_CURVE ( 'NONE', #38485, #39783, #9168, .T. ) ;
#4351 = CARTESIAN_POINT ( 'NONE',  ( -3.854280124997887746, 21.23357344512866973, -2.551540157904111261 ) ) ;
#4352 = CARTESIAN_POINT ( 'NONE',  ( 9.006184665392719779, 123.9742709865185191, 0.2138692079817592906 ) ) ;
#4353 = CARTESIAN_POINT ( 'NONE',  ( -3.372034046726852807, 108.0377789575252194, 4.123912905361212466 ) ) ;
#4354 = CARTESIAN_POINT ( 'NONE',  ( -51.32320689156235005, 13.70825103427969438, -4.126761985266684363 ) ) ;
#4355 = CARTESIAN_POINT ( 'NONE',  ( 2.181655109597531617, 116.2239731218073615, -0.08111321244062891234 ) ) ;
#4356 = DIRECTION ( 'NONE',  ( -0.8745520943968241312, 0.4849315768086548406, -5.691349986800536046E-16 ) ) ;
#4357 = AXIS2_PLACEMENT_3D ( 'NONE', #35062, #29914, #23077 ) ;
#4358 = CARTESIAN_POINT ( 'NONE',  ( -46.84023172327227513, 25.61286091221859351, -1.557636486551099875 ) ) ;
#4359 = CARTESIAN_POINT ( 'NONE',  ( -0.1065207248106255222, 105.8844037013956125, 5.332933549509750293 ) ) ;
#4360 = CARTESIAN_POINT ( 'NONE',  ( -33.20758249455312239, 49.81222039523557044, -1.524000000000005350 ) ) ;
#4361 = CARTESIAN_POINT ( 'NONE',  ( 4.698174212119619497, 9.136213905105968536, -7.004248122051734526 ) ) ;
#4362 = CARTESIAN_POINT ( 'NONE',  ( -5.115576404396798615, 56.51500000000000767, 4.603576161448844850 ) ) ;
#4363 = DIRECTION ( 'NONE',  ( -5.188838149069471174E-16, 1.699382548006136313E-16, 1.000000000000000000 ) ) ;
#4364 = CARTESIAN_POINT ( 'NONE',  ( -58.66661043166477896, 0.3408866871785626307, 0.5032371457779101220 ) ) ;
#4365 = CARTESIAN_POINT ( 'NONE',  ( -58.73801720703743001, -0.4998429216807459552, 0.2437502737749395465 ) ) ;
#4366 = CARTESIAN_POINT ( 'NONE',  ( -23.22389216488258867, 148.7951734159264561, 0.1326450332456386438 ) ) ;
#4367 = EDGE_LOOP ( 'NONE', ( #33395, #40194, #15655, #31299 ) ) ;
#4368 = CARTESIAN_POINT ( 'NONE',  ( -57.90853684698413417, 2.514838786807874094, -0.1030880274589022344 ) ) ;
#4369 = CARTESIAN_POINT ( 'NONE',  ( 7.785084361432049072, 122.6279490200930695, 0.1367715089808400897 ) ) ;
#4370 = EDGE_LOOP ( 'NONE', ( #28632, #8684, #18738, #17872 ) ) ;
#4371 = LINE ( 'NONE', #23927, #16491 ) ;
#4372 = CARTESIAN_POINT ( 'NONE',  ( -7.787205264484130751, 154.6472212274131550, -0.1983306932048339022 ) ) ;
#4373 = CARTESIAN_POINT ( 'NONE',  ( 3.039728791924208195, -15.34324946256290723, 5.681930179901951483 ) ) ;
#4374 = CARTESIAN_POINT ( 'NONE',  ( -7.892561109811933484, 118.8455990504009492, 0.9355921144164882630 ) ) ;
#4375 = CARTESIAN_POINT ( 'NONE',  ( 2.332027132427558769, 25.33165720878049498, 3.998286310156994983 ) ) ;
#4376 = AXIS2_PLACEMENT_3D ( 'NONE', #29722, #16931, #16718 ) ;
#4377 = CARTESIAN_POINT ( 'NONE',  ( 6.906622810364680731, 117.2343425291504104, 0.3847307661620061325 ) ) ;
#4378 = DIRECTION ( 'NONE',  ( -0.9998004120163609398, 0.000000000000000000, -0.01997839162482749689 ) ) ;
#4379 = CARTESIAN_POINT ( 'NONE',  ( -29.20126717796659577, 63.92883165588695960, 1.269999999999993578 ) ) ;
#4380 = CARTESIAN_POINT ( 'NONE',  ( -0.09873697212813982438, -3.591044343564580910, 0.9733856795103970061 ) ) ;
#4381 = CARTESIAN_POINT ( 'NONE',  ( -17.10498822929456253, 122.7072422303320707, -0.5849822763170866580 ) ) ;
#4382 = CARTESIAN_POINT ( 'NONE',  ( 6.059261036834406866, 57.14999999999999858, 5.016499999999999737 ) ) ;
#4383 = DIRECTION ( 'NONE',  ( 1.000000000000000000, 6.353134868986659519E-16, 0.000000000000000000 ) ) ;
#4384 = EDGE_LOOP ( 'NONE', ( #34868, #37574, #30317, #22681 ) ) ;
#4385 = CARTESIAN_POINT ( 'NONE',  ( 5.535474336661085459, 116.8955343539433045, 0.5335339445610354225 ) ) ;
#4386 = CARTESIAN_POINT ( 'NONE',  ( -11.17823620286587349, 123.1247571232444784, 1.162497134544157928 ) ) ;
#4387 = CARTESIAN_POINT ( 'NONE',  ( -57.96913128882820132, 0.5713783965472770676, -0.8987469434438276616 ) ) ;
#4388 = CARTESIAN_POINT ( 'NONE',  ( 5.844153588741368921, 118.3130479344264501, 1.074361049658993927 ) ) ;
#4389 = CARTESIAN_POINT ( 'NONE',  ( 6.324931890614029051, 157.3995435888475072, -1.705594245970836420 ) ) ;
#4390 = AXIS2_PLACEMENT_3D ( 'NONE', #10087, #23482, #23696 ) ;
#4391 = TOROIDAL_SURFACE ( 'NONE', #26123, 0.7620000000000000107, 0.2540000000000000036 ) ;
#4392 = CARTESIAN_POINT ( 'NONE',  ( 0.2395577018624739096, -8.716993574909102094, 0.9436776969787653568 ) ) ;
#4393 = CARTESIAN_POINT ( 'NONE',  ( -20.92851329017044293, 150.0074445146613584, -2.223361304733721955 ) ) ;
#4394 = CARTESIAN_POINT ( 'NONE',  ( -47.11704014324645584, 20.18577099567727373, -5.127035723291441194 ) ) ;
#4395 = CARTESIAN_POINT ( 'NONE',  ( 5.344249437077539966, 105.1225132350959939, -0.1103424742704069983 ) ) ;
#4396 = CARTESIAN_POINT ( 'NONE',  ( 5.880513813086725605, 121.0368588677253143, -0.5043468530174898268 ) ) ;
#4397 = CARTESIAN_POINT ( 'NONE',  ( -9.104209967888042598, 153.9432936505793066, -0.1819237819739442652 ) ) ;
#4398 = ORIENTED_EDGE ( 'NONE', *, *, #16689, .T. ) ;
#4399 = CARTESIAN_POINT ( 'NONE',  ( -18.01525633490682665, 148.5173242358814321, -2.382443637188214502 ) ) ;
#4400 = CARTESIAN_POINT ( 'NONE',  ( 2.867278011408870064, -15.71882806570827640, 4.918777663456151750 ) ) ;
#4401 = AXIS2_PLACEMENT_3D ( 'NONE', #38679, #39306, #32281 ) ;
#4402 = CARTESIAN_POINT ( 'NONE',  ( -30.20416046766209917, 71.17241488000101413, -1.524000000000007571 ) ) ;
#4403 = CARTESIAN_POINT ( 'NONE',  ( -4.392784016475978603, 118.1805867164427184, -0.5718452568440313133 ) ) ;
#4404 = CARTESIAN_POINT ( 'NONE',  ( -48.82738941085167284, 18.57305038084609095, -5.399437279161923620 ) ) ;
#4405 = CARTESIAN_POINT ( 'NONE',  ( 4.109713352107567275, 118.2429491485453354, 0.3484632730576381343 ) ) ;
#4406 = CARTESIAN_POINT ( 'NONE',  ( 17.50950237657569986, 148.8653046532945723, 2.321071487785774767 ) ) ;
#4407 = DIRECTION ( 'NONE',  ( -0.1728608224830406603, -1.098208118798718614E-16, -0.9849462604886047856 ) ) ;
#4408 = CARTESIAN_POINT ( 'NONE',  ( 23.45208337669170007, 146.8499405026647651, 0.4686284387228156212 ) ) ;
#4409 = CARTESIAN_POINT ( 'NONE',  ( -5.330747076954383878, 11.08732641057851964, -6.519097198751918398 ) ) ;
#4410 = CARTESIAN_POINT ( 'NONE',  ( 15.89665129872314431, 146.6311637152522565, 0.9120559015848338502 ) ) ;
#4411 = CARTESIAN_POINT ( 'NONE',  ( 0.01443894962456075334, 159.4760848062415732, -0.7225840825867285711 ) ) ;
#4412 = CARTESIAN_POINT ( 'NONE',  ( -42.63057730194584849, 21.82620848986230300, -1.774738817929691237 ) ) ;
#4413 = CARTESIAN_POINT ( 'NONE',  ( 0.4699976290979421267, 115.6909491485452719, 1.765048339911096553 ) ) ;
#4414 = CARTESIAN_POINT ( 'NONE',  ( -57.50808096206083775, 1.366199858870195794, 0.4699486091021412570 ) ) ;
#4415 = CARTESIAN_POINT ( 'NONE',  ( -3.728135546147876678, 116.6403000632267464, 0.003128093132697681595 ) ) ;
#4416 = ORIENTED_EDGE ( 'NONE', *, *, #6379, .F. ) ;
#4417 = CARTESIAN_POINT ( 'NONE',  ( -47.62964748377234514, 25.45032632311202647, -0.1281092358103206041 ) ) ;
#4418 = CARTESIAN_POINT ( 'NONE',  ( -6.784182173561120521, 121.2536750021979799, -0.8970767929546700215 ) ) ;
#4419 = DIRECTION ( 'NONE',  ( 5.188838149069471174E-16, -1.699382548006136313E-16, -1.000000000000000000 ) ) ;
#4420 = ORIENTED_EDGE ( 'NONE', *, *, #27782, .F. ) ;
#4421 = CARTESIAN_POINT ( 'NONE',  ( -4.611806494114576438, 117.9324678712513759, -0.9633187536371230486 ) ) ;
#4422 = CARTESIAN_POINT ( 'NONE',  ( -7.055095707297289742, 122.0164807696326790, -0.4009610655988181671 ) ) ;
#4423 = CARTESIAN_POINT ( 'NONE',  ( 4.673344545167823938, -12.29283961637177214, 1.688191869143181201 ) ) ;
#4424 = CARTESIAN_POINT ( 'NONE',  ( -3.058359628041920963, 159.2229145144301867, 0.9584471420995394064 ) ) ;
#4425 = DIRECTION ( 'NONE',  ( -1.000000000000000000, -6.353134868986659519E-16, 0.000000000000000000 ) ) ;
#4426 = CARTESIAN_POINT ( 'NONE',  ( 23.44243449907606092, 146.8400249081559537, 0.5456528120549732908 ) ) ;
#4427 = VERTEX_POINT ( 'NONE', #30219 ) ;
#4428 = CARTESIAN_POINT ( 'NONE',  ( 4.440276399826426967, -1.430929408009915083, -1.287880193523989636 ) ) ;
#4429 = CARTESIAN_POINT ( 'NONE',  ( -1.421603664355800101, 159.6054662015457666, -0.02840702444251828190 ) ) ;
#4430 = CARTESIAN_POINT ( 'NONE',  ( -17.99070523305417169, 61.93444992276926797, 1.523999999999999799 ) ) ;
#4431 = DIRECTION ( 'NONE',  ( -4.017660918040594346E-17, 1.000000000000000000, 2.376309959284834438E-19 ) ) ;
#4432 = VERTEX_POINT ( 'NONE', #40039 ) ;
#4433 = CARTESIAN_POINT ( 'NONE',  ( 6.506277007714310834, 119.7857196899097119, 1.251456028858768610 ) ) ;
#4434 = CARTESIAN_POINT ( 'NONE',  ( 2.459658384930404118, -7.418532284756778949, 3.912982838641719141 ) ) ;
#4435 = CARTESIAN_POINT ( 'NONE',  ( 8.039955067132906308, 118.1206512225135015, 0.9611422114813542583 ) ) ;
#4436 = CARTESIAN_POINT ( 'NONE',  ( -58.68789525397659190, -0.3143212917568471987, -0.3020521592213566975 ) ) ;
#4437 = CARTESIAN_POINT ( 'NONE',  ( 2.760819571866365951, 158.5977336698458089, -1.488126253378572184 ) ) ;
#4438 = CARTESIAN_POINT ( 'NONE',  ( -1.146732334619779969, -3.095543821355960734, -4.488006035213349953 ) ) ;
#4439 = CARTESIAN_POINT ( 'NONE',  ( -9.505306604063539666, 118.4542681464805298, -0.9615324788044602444 ) ) ;
#4440 = ORIENTED_EDGE ( 'NONE', *, *, #30050, .F. ) ;
#4441 = CARTESIAN_POINT ( 'NONE',  ( -11.88810549871057454, 151.9737369308441544, 0.07145411264644083160 ) ) ;
#4442 = CARTESIAN_POINT ( 'NONE',  ( 3.231152580208111580, -15.43077800403741584, 5.551260886339890455 ) ) ;
#4443 = CARTESIAN_POINT ( 'NONE',  ( -45.90302585792925782, 20.78970012321182992, 4.334318749026192741 ) ) ;
#4444 = B_SPLINE_CURVE_WITH_KNOTS ( 'NONE', 3,
 ( #20833, #33231, #33857, #30644 ),
 .UNSPECIFIED., .F., .F.,
 ( 4, 4 ),
 ( 0.0001481480970339296298, 0.0005781902081302999060 ),
 .UNSPECIFIED. ) ;
#4445 = CARTESIAN_POINT ( 'NONE',  ( -0.3864694276889155677, 117.9496048067635456, -1.408072416706073415 ) ) ;
#4446 = ORIENTED_EDGE ( 'NONE', *, *, #7122, .T. ) ;
#4447 = CARTESIAN_POINT ( 'NONE',  ( 12.16261443152838773, 122.9664497093790629, 1.797897170200384753 ) ) ;
#4448 = CARTESIAN_POINT ( 'NONE',  ( -26.42106975583004314, 72.48669692073261217, -1.270000000000005791 ) ) ;
#4449 = CARTESIAN_POINT ( 'NONE',  ( -29.81952093677235993, 58.81079514833387378, -1.270000000000005125 ) ) ;
#4450 = CARTESIAN_POINT ( 'NONE',  ( -6.890728787288654900, 117.8105958006179890, 0.6119090536800846358 ) ) ;
#4451 = CARTESIAN_POINT ( 'NONE',  ( -8.422295717417405569, 8.547183656736235591, -0.3195422701574849311 ) ) ;
#4452 = CARTESIAN_POINT ( 'NONE',  ( 10.26858343235344861, 124.8461398015159745, 0.9314245544334066595 ) ) ;
#4453 = FACE_OUTER_BOUND ( 'NONE', #29240, .T. ) ;
#4454 = CIRCLE ( 'NONE', #26199, 0.5079999999999963434 ) ;
#4455 = CARTESIAN_POINT ( 'NONE',  ( 19.95587765737794683, 128.8226523212408949, -0.2284701554834993320 ) ) ;
#4456 = CARTESIAN_POINT ( 'NONE',  ( -5.486567272856878414E-14, 86.35999999999998522, 0.000000000000000000 ) ) ;
#4457 = CARTESIAN_POINT ( 'NONE',  ( -56.65145866349825354, 3.394461374620260763, 2.057387993278029015 ) ) ;
#4458 = CARTESIAN_POINT ( 'NONE',  ( -48.87999295267864142, 23.89022491863793718, 0.5351834272454346619 ) ) ;
#4459 = CARTESIAN_POINT ( 'NONE',  ( -57.78858274104275949, 1.044662872677112997, 1.355440516197746303 ) ) ;
#4460 = CARTESIAN_POINT ( 'NONE',  ( -58.13496148655324447, 0.7694742097100807365, 1.214799913285357302 ) ) ;
#4461 = CARTESIAN_POINT ( 'NONE',  ( -4.478724048142634473, 118.1112337407861048, 0.5787802498093359560 ) ) ;
#4462 = CARTESIAN_POINT ( 'NONE',  ( 2.507403849662985795, 107.3040393085582167, -4.608059665216667433 ) ) ;
#4463 = EDGE_LOOP ( 'NONE', ( #4041, #9223, #31844, #1633 ) ) ;
#4464 = CARTESIAN_POINT ( 'NONE',  ( -46.30033180095409762, 21.65562830348028456, 4.292083522273594909 ) ) ;
#4465 = CARTESIAN_POINT ( 'NONE',  ( 6.052716142014698875, 119.3318794080258129, -1.025634881525736786 ) ) ;
#4466 = CARTESIAN_POINT ( 'NONE',  ( -6.308735553862911516, 120.0717973201777511, -0.4535485300176084755 ) ) ;
#4467 = CARTESIAN_POINT ( 'NONE',  ( 4.448170622692431131, 118.1283731037481601, 0.7238786398437021541 ) ) ;
#4468 = CARTESIAN_POINT ( 'NONE',  ( -16.13275712328133693, 147.4171829256358137, -1.433441054525536051 ) ) ;
#4469 = FILL_AREA_STYLE ('',( #7654 ) ) ;
#4470 = CARTESIAN_POINT ( 'NONE',  ( 2.810880042475876639, 117.3993815990320542, -1.303394573401737810 ) ) ;
#4471 = CARTESIAN_POINT ( 'NONE',  ( -4.050807963365556930, 30.95410787014092335, -2.229501126309402448 ) ) ;
#4472 = CARTESIAN_POINT ( 'NONE',  ( -9.375340687752244051, 122.9055586947561522, -1.148039706409768490 ) ) ;
#4473 = CARTESIAN_POINT ( 'NONE',  ( -10.00099186598785117, 77.19260062651656540, -1.269999999999998019 ) ) ;
#4474 = CYLINDRICAL_SURFACE ( 'NONE', #23055, 0.2540000000000013358 ) ;
#4475 = CARTESIAN_POINT ( 'NONE',  ( 7.845668856638584820, 122.3864107020766596, -0.3364293281536828162 ) ) ;
#4476 = CARTESIAN_POINT ( 'NONE',  ( -2.867346308344148831, 121.0282051601325577, 0.04542865946695314600 ) ) ;
#4477 = CARTESIAN_POINT ( 'NONE',  ( 6.888626713468121388, 117.5201695557886410, 0.7016588733424087287 ) ) ;
#4478 = CARTESIAN_POINT ( 'NONE',  ( 5.305748947172191698, 88.73331249999999670, -5.247078976224250013 ) ) ;
#4479 = CARTESIAN_POINT ( 'NONE',  ( 3.261251233531137217, -14.70027692227136917, 2.623613175195522285 ) ) ;
#4480 = CARTESIAN_POINT ( 'NONE',  ( -11.63135762381498850, 122.7176759045101022, 1.263630383496116005 ) ) ;
#4481 = CARTESIAN_POINT ( 'NONE',  ( 0.3740510792576948185, -8.494654975422754717, 0.8997923438783246297 ) ) ;
#4482 = CARTESIAN_POINT ( 'NONE',  ( -3.185756255432687922, 159.4163042773305676, -0.6073767776667647889 ) ) ;
#4483 = CARTESIAN_POINT ( 'NONE',  ( 0.2014313232957813393, -8.551994341567581870, -0.9548264729560895780 ) ) ;
#4484 = ORIENTED_EDGE ( 'NONE', *, *, #4501, .F. ) ;
#4485 = CARTESIAN_POINT ( 'NONE',  ( -51.86985193027736329, 10.34936321858908492, -8.341425858057926505E-15 ) ) ;
#4486 = CARTESIAN_POINT ( 'NONE',  ( 5.166232791441969674, 115.4535745449993982, 1.513138011745335909 ) ) ;
#4487 = TOROIDAL_SURFACE ( 'NONE', #23506, 0.3809999999999999498, 0.2540000000000000036 ) ;
#4488 = CARTESIAN_POINT ( 'NONE',  ( -0.004350076772786141965, 120.7058980590201429, 0.2176956299261768035 ) ) ;
#4489 = CARTESIAN_POINT ( 'NONE',  ( 4.598504975971844821, -12.83055836278033901, 2.569316529143384820 ) ) ;
#4490 = CARTESIAN_POINT ( 'NONE',  ( 15.09269357795375122, 134.7883251604851580, -1.349233830697067926 ) ) ;
#4491 = ORIENTED_EDGE ( 'NONE', *, *, #2459, .F. ) ;
#4492 = CARTESIAN_POINT ( 'NONE',  ( -12.25516334840921928, 122.6846661264431191, -1.808440497450061413 ) ) ;
#4493 = DIRECTION ( 'NONE',  ( 0.6825627711659331132, 0.7308269722843310223, 2.299753143848214142E-16 ) ) ;
#4494 = CARTESIAN_POINT ( 'NONE',  ( 3.259676495098780880, -13.96886708669151034, 2.676229364769742158 ) ) ;
#4495 = CARTESIAN_POINT ( 'NONE',  ( -4.830560651430104713, 117.5458123619130646, -1.145125986471454027 ) ) ;
#4496 = CARTESIAN_POINT ( 'NONE',  ( 0.001786757842147936167, 120.9379535345006076, -0.08941666878750646752 ) ) ;
#4497 = VERTEX_POINT ( 'NONE', #14229 ) ;
#4498 = CARTESIAN_POINT ( 'NONE',  ( 12.41171712301729713, 121.5863879130357503, 1.717582910027388721 ) ) ;
#4499 = CARTESIAN_POINT ( 'NONE',  ( 2.894556870215603261, 107.8345691432927254, 4.471910717343379638 ) ) ;
#4500 = CARTESIAN_POINT ( 'NONE',  ( 15.21260244842765985, 17.14499999999999957, 1.863006489516811765E-15 ) ) ;
#4501 = EDGE_CURVE ( 'NONE', #39783, #26876, #31229, .T. ) ;
#4502 = CARTESIAN_POINT ( 'NONE',  ( 17.17894352244471534, 122.7237354506536491, 0.1767255469942458634 ) ) ;
#4503 = DIRECTION ( 'NONE',  ( 0.000000000000000000, 0.000000000000000000, 1.000000000000000000 ) ) ;
#4504 = CARTESIAN_POINT ( 'NONE',  ( 2.153962292805264855, -15.42765719885048981, 5.938214566648465365 ) ) ;
#4505 = CARTESIAN_POINT ( 'NONE',  ( 1.222676017494593648E-15, 12.70000000000000284, 0.000000000000000000 ) ) ;
#4506 = DIRECTION ( 'NONE',  ( 5.188838149069472160E-16, -1.699382548006136559E-16, -1.000000000000000000 ) ) ;
#4507 = EDGE_CURVE ( 'NONE', #5717, #25039, #6768, .T. ) ;
#4508 = CARTESIAN_POINT ( 'NONE',  ( -0.01081828485868089468, 118.1092738308834669, 0.5413912121690739321 ) ) ;
#4509 = CIRCLE ( 'NONE', #14686, 9.048749999999998295 ) ;
#4510 = VERTEX_POINT ( 'NONE', #7026 ) ;
#4511 = CARTESIAN_POINT ( 'NONE',  ( 7.891363246779867779, 17.78247237326412034, -2.951631208061117562 ) ) ;
#4512 = CARTESIAN_POINT ( 'NONE',  ( -2.209815719917325616, 116.9321326171075413, -0.5724128154462628792 ) ) ;
#4513 = CARTESIAN_POINT ( 'NONE',  ( -0.007549346801299551199, 106.0530876078258586, -5.266739608401566741 ) ) ;
#4514 = DIRECTION ( 'NONE',  ( -1.000000000000000000, 0.000000000000000000, 0.000000000000000000 ) ) ;
#4515 = FACE_OUTER_BOUND ( 'NONE', #30146, .T. ) ;
#4516 = CARTESIAN_POINT ( 'NONE',  ( -4.591961393772478139, 104.6144662015457811, 1.495199714113508049 ) ) ;
#4517 = CARTESIAN_POINT ( 'NONE',  ( -0.2480930319908794535, 10.21371511114847053, -4.635561276548324727 ) ) ;
#4518 = DIRECTION ( 'NONE',  ( -5.188838149069471174E-16, 1.699382548006136313E-16, 1.000000000000000000 ) ) ;
#4519 = CARTESIAN_POINT ( 'NONE',  ( -2.293106875121391663, 106.8185943591930993, -4.820918091293040497 ) ) ;
#4520 = CARTESIAN_POINT ( 'NONE',  ( 3.361318737587208005, -13.21634134694392415, 1.934622048986600840 ) ) ;
#4521 = CARTESIAN_POINT ( 'NONE',  ( 3.175984444280615104, 117.6701293611589278, -0.8859276027576483692 ) ) ;
#4522 = CARTESIAN_POINT ( 'NONE',  ( -5.005498311287589708, 28.16151697905833373, 1.324705785854183748 ) ) ;
#4523 = CARTESIAN_POINT ( 'NONE',  ( -28.36525985791271154, 77.02308833105713859, -1.270000000000007345 ) ) ;
#4524 = ORIENTED_EDGE ( 'NONE', *, *, #41616, .T. ) ;
#4525 = CARTESIAN_POINT ( 'NONE',  ( -5.339850745321377268, 104.6144662015545066, -0.2412019823091631210 ) ) ;
#4526 = CARTESIAN_POINT ( 'NONE',  ( 4.357275237516622823, -15.68314232965556343, 3.240836981083619062 ) ) ;
#4527 = CARTESIAN_POINT ( 'NONE',  ( -18.20160870511337592, 135.6759721228443425, 1.705493676697015015 ) ) ;
#4528 = CARTESIAN_POINT ( 'NONE',  ( -2.646443841375008432, -8.127818987380491578, -3.789199236247322133 ) ) ;
#4529 = EDGE_CURVE ( 'NONE', #37319, #13530, #32097, .T. ) ;
#4530 = VERTEX_POINT ( 'NONE', #23170 ) ;
#4531 = ORIENTED_EDGE ( 'NONE', *, *, #40973, .T. ) ;
#4532 = FACE_OUTER_BOUND ( 'NONE', #27252, .T. ) ;
#4533 = CARTESIAN_POINT ( 'NONE',  ( 0.5479319383245284669, 107.0594419416054848, 4.854436055212457468 ) ) ;
#4534 = PRODUCT ( 'Pivot Pins', 'Pivot Pins', '', ( #27049 ) ) ;
#4535 = CARTESIAN_POINT ( 'NONE',  ( -6.676265340062506048, 155.5185402614932570, 1.076558685701347384 ) ) ;
#4536 = CARTESIAN_POINT ( 'NONE',  ( -45.77009227191969387, 21.09669921233918544, 4.287731683635674251 ) ) ;
#4537 = ADVANCED_FACE ( 'NONE', ( #1479 ), #22537, .T. ) ;
#4538 = CARTESIAN_POINT ( 'NONE',  ( 3.394752741017162290, 119.5845705363850442, -0.6980748167159183115 ) ) ;
#4539 = CARTESIAN_POINT ( 'NONE',  ( -13.38228307180527565, 122.0388263298542739, -1.742221313037096264 ) ) ;
#4540 = CARTESIAN_POINT ( 'NONE',  ( 13.85159022459153988, 12.96416000000000146, 5.016499999999999737 ) ) ;
#4541 = ADVANCED_FACE ( 'NONE', ( #17843, #14644 ), #37662, .F. ) ;
#4542 = ORIENTED_EDGE ( 'NONE', *, *, #6317, .F. ) ;
#4543 = CIRCLE ( 'NONE', #27646, 7.461249999999999716 ) ;
#4544 = CARTESIAN_POINT ( 'NONE',  ( 4.313720991269348382, 118.2128926607351929, -0.3282634486935400164 ) ) ;
#4545 = CARTESIAN_POINT ( 'NONE',  ( 14.56142545302297364, 139.1552669279217298, -0.4455586761712629906 ) ) ;
#4546 = CIRCLE ( 'NONE', #29021, 0.5080000000000002292 ) ;
#4547 = EDGE_LOOP ( 'NONE', ( #7311, #36567, #14602, #25830 ) ) ;
#4548 = CARTESIAN_POINT ( 'NONE',  ( 3.235674727752381852, -14.79813088844142399, -0.3705354414145333730 ) ) ;
#4549 = CARTESIAN_POINT ( 'NONE',  ( -5.684927786827005392, 65.51297084251929448, 1.270000000000005347 ) ) ;
#4550 = CARTESIAN_POINT ( 'NONE',  ( -48.44329217233245544, 18.62907245612966634, 5.187175938574861256 ) ) ;
#4551 = CARTESIAN_POINT ( 'NONE',  ( -3.469956624915944587, 9.623539240006554252, 3.074419811715999984 ) ) ;
#4552 = CARTESIAN_POINT ( 'NONE',  ( 10.46581596931669722, 123.6668265419868646, 1.337773356492248711 ) ) ;
#4553 = CARTESIAN_POINT ( 'NONE',  ( -1.659418339086100591, 31.10872648155390507, 2.656305225562720196 ) ) ;
#4554 = CARTESIAN_POINT ( 'NONE',  ( -6.476067766296674577, 120.6581566633936404, 0.1355830077277816459 ) ) ;
#4555 = CARTESIAN_POINT ( 'NONE',  ( -3.640175008984333882, 11.51306413504884318, -2.862805987297033727 ) ) ;
#4556 = CARTESIAN_POINT ( 'NONE',  ( 9.106973723525536357, 153.9337724597031070, 0.2264262902970469726 ) ) ;
#4557 = LINE ( 'NONE', #26699, #35144 ) ;
#4558 = CARTESIAN_POINT ( 'NONE',  ( -56.91016477577836952, 2.896953902749091370, -2.060321699029003195 ) ) ;
#4559 = CARTESIAN_POINT ( 'NONE',  ( 5.556563611783038148, 116.7705472551883901, -0.1784112738407624132 ) ) ;
#4560 = AXIS2_PLACEMENT_3D ( 'NONE', #32547, #22517, #9346 ) ;
#4561 = CARTESIAN_POINT ( 'NONE',  ( -7.842268484490568348, 73.30875693322846587, 1.524000000000003130 ) ) ;
#4562 = CARTESIAN_POINT ( 'NONE',  ( -46.83538438062986842, 25.62937243838004520, -1.546882883115203500 ) ) ;
#4563 = CARTESIAN_POINT ( 'NONE',  ( -1.969665360195132608, 106.3924174363482678, 4.957232547992387772 ) ) ;
#4564 = CARTESIAN_POINT ( 'NONE',  ( -11.53797084252497385, 82.58007221317646440, -1.524000000000000021 ) ) ;
#4565 = CARTESIAN_POINT ( 'NONE',  ( 8.428375251627102216, -1.854023157342211903, -0.5381045032988257537 ) ) ;
#4566 = DIRECTION ( 'NONE',  ( 5.188838149069472160E-16, -1.699382548006136559E-16, -1.000000000000000000 ) ) ;
#4567 = CARTESIAN_POINT ( 'NONE',  ( 3.174366308151881810, 78.32546620154573702, 0.06343139340882768262 ) ) ;
#4568 = CARTESIAN_POINT ( 'NONE',  ( -58.73915225836899623, 0.1638436772961326948, 0.01855759196810149655 ) ) ;
#4569 = CARTESIAN_POINT ( 'NONE',  ( 0.002462548248794847305, 123.7646714092002611, -0.1232359841711013482 ) ) ;
#4570 = CARTESIAN_POINT ( 'NONE',  ( -17.03046551078694293, 122.6950552906510694, -0.003367075177501115558 ) ) ;
#4571 = CIRCLE ( 'NONE', #1198, 0.5080000000000000071 ) ;
#4572 = ORIENTED_EDGE ( 'NONE', *, *, #12305, .F. ) ;
#4573 = CARTESIAN_POINT ( 'NONE',  ( -57.37345908981379949, 3.796002467274087078, -0.9053535129859066055 ) ) ;
#4574 = CARTESIAN_POINT ( 'NONE',  ( 7.788904351887272703, 122.6147082451171713, 0.08148216547788392217 ) ) ;
#4575 = EDGE_CURVE ( 'NONE', #30491, #10192, #11249, .T. ) ;
#4576 = ORIENTED_EDGE ( 'NONE', *, *, #28731, .T. ) ;
#4577 = CARTESIAN_POINT ( 'NONE',  ( -47.20932677516409370, 20.06242161047478234, -5.120036295481038557 ) ) ;
#4578 = CARTESIAN_POINT ( 'NONE',  ( -9.128616289401854544, 124.2274432543504332, -0.1375126816698667986 ) ) ;
#4579 = CARTESIAN_POINT ( 'NONE',  ( 5.121635214396401459, -14.94813357331645243, 3.889196783476005059 ) ) ;
#4580 = CARTESIAN_POINT ( 'NONE',  ( -4.850700283611360852, 158.3075559295907055, 1.526604748539100997 ) ) ;
#4581 = CARTESIAN_POINT ( 'NONE',  ( 23.06197264524083579, 149.2510847660714148, 1.189562549516614665 ) ) ;
#4582 = CARTESIAN_POINT ( 'NONE',  ( 1.339128788961291283, 159.4185946040361728, -0.8255809207588793441 ) ) ;
#4583 = CARTESIAN_POINT ( 'NONE',  ( 0.9564925537785137211, 29.00497265395555857, -4.523030980006896407 ) ) ;
#4584 = CARTESIAN_POINT ( 'NONE',  ( -18.63890302240357144, 125.2334963081946313, -0.6306532867605572079 ) ) ;
#4585 = CARTESIAN_POINT ( 'NONE',  ( -53.23100645945389431, 10.70077955446924456, -4.015069180613662247 ) ) ;
#4586 = ORIENTED_EDGE ( 'NONE', *, *, #25846, .T. ) ;
#4587 = B_SPLINE_CURVE_WITH_KNOTS ( 'NONE', 3,
 ( #3349, #16315, #26121, #39125, #1413, #17159, #4197, #33994, #13556, #37180, #24169, #7379, #17571, #787, #30159, #16949, #7179, #4412, #20139, #29948, #26545, #10355, #33364, #3990 ),
 .UNSPECIFIED., .F., .F.,
 ( 4, 2, 2, 2, 2, 2, 2, 2, 2, 2, 2, 4 ),
 ( 0.000000000000000000, 0.0005646226568491961037, 0.001129245313698392207, 0.001693867970547588203, 0.002258490627396784415, 0.003387735941095171635, 0.004516981254793559289, 0.005646226568491947810, 0.006775471882190335464, 0.007340094539039522352, 0.007904717195888708373, 0.009033962509587089088 ),
 .UNSPECIFIED. ) ;
#4588 = CARTESIAN_POINT ( 'NONE',  ( -8.786270220348933790, 117.7728096769080679, 0.1425748814448410673 ) ) ;
#4589 = CARTESIAN_POINT ( 'NONE',  ( -11.48915734413155398, 123.4929228318607386, 1.183242792625787576 ) ) ;
#4590 = CARTESIAN_POINT ( 'NONE',  ( -57.65211917320155521, 1.256797420531753584, -1.252854774673126670 ) ) ;
#4591 = CARTESIAN_POINT ( 'NONE',  ( 9.920314382278954568, 120.7895603300898699, -1.200622369358214758 ) ) ;
#4592 = CARTESIAN_POINT ( 'NONE',  ( -0.9396370176409497565, -11.09013235204027659, 0.2555656002325920051 ) ) ;
#4593 = CARTESIAN_POINT ( 'NONE',  ( -2.121516847112316917, 117.7847241295267651, -0.6923378844829269907 ) ) ;
#4594 = CARTESIAN_POINT ( 'NONE',  ( -47.04837031381860157, 23.61299024743492581, -3.054033755318078303 ) ) ;
#4595 = VECTOR ( 'NONE', #25304, 1000.000000000000114 ) ;
#4596 = EDGE_CURVE ( 'NONE', #5970, #33026, #37867, .T. ) ;
#4597 = CARTESIAN_POINT ( 'NONE',  ( 5.339689988358259143, 105.1224923508004707, 0.2456598103791063359 ) ) ;
#4598 = CARTESIAN_POINT ( 'NONE',  ( 0.006810764310266656518, 120.3493709785083183, -0.3408384964863780398 ) ) ;
#4599 = CARTESIAN_POINT ( 'NONE',  ( -4.883848590450072358, 117.7607009110569862, 0.7127853619805604168 ) ) ;
#4600 = VERTEX_POINT ( 'NONE', #12091 ) ;
#4601 = CARTESIAN_POINT ( 'NONE',  ( -12.17039870458273043, 124.2599011343719155, -1.750469281869918792 ) ) ;
#4602 = CARTESIAN_POINT ( 'NONE',  ( 2.341541575351651083, -15.74615379138004378, 5.495207524874286875 ) ) ;
#4603 = EDGE_CURVE ( 'NONE', #24258, #10259, #8293, .T. ) ;
#4604 = DIRECTION ( 'NONE',  ( -4.017660918040594346E-17, 1.000000000000000000, 2.376309959284834438E-19 ) ) ;
#4605 = CARTESIAN_POINT ( 'NONE',  ( -4.301501440665757237, 118.2120994191875099, -0.4958915692504695105 ) ) ;
#4606 = CARTESIAN_POINT ( 'NONE',  ( -53.09398923718962493, 10.65108322687173548, -3.938325876039776574 ) ) ;
#4607 = CIRCLE ( 'NONE', #12749, 0.2539999999999967839 ) ;
#4608 = CARTESIAN_POINT ( 'NONE',  ( 4.151427346349458425, 118.2394115087963371, 0.3932352160703678767 ) ) ;
#4609 = CARTESIAN_POINT ( 'NONE',  ( 7.499533598998342043, 156.0351187175861867, 1.911400249181836264 ) ) ;
#4610 = DIRECTION ( 'NONE',  ( 0.4849315768086533973, 0.8745520943968251304, 1.030032898892973955E-16 ) ) ;
#4611 = CARTESIAN_POINT ( 'NONE',  ( 16.18905205736044906, 121.2598130428683447, 0.3234957879086920451 ) ) ;
#4612 = CARTESIAN_POINT ( 'NONE',  ( 8.244768260990875675, 16.90678017261275556, 1.796629206788997513 ) ) ;
#4613 = CARTESIAN_POINT ( 'NONE',  ( 15.86281397719557162, 145.7686330500600036, 0.9137093302325698385 ) ) ;
#4614 = CARTESIAN_POINT ( 'NONE',  ( 22.74864191258929935, 148.7873826295267747, -0.7277888646341178491 ) ) ;
#4615 = DIRECTION ( 'NONE',  ( -0.6825627711659328911, -0.7308269722843309113, -2.299753143848213649E-16 ) ) ;
#4616 = CARTESIAN_POINT ( 'NONE',  ( 1.984410438080367767, 115.6909491485452719, 1.718756010027771230 ) ) ;
#4617 = CIRCLE ( 'NONE', #31137, 9.048749999999998295 ) ;
#4618 = CARTESIAN_POINT ( 'NONE',  ( -57.74348367832291018, 0.8661236967133778553, 0.1780388485286100997 ) ) ;
#4619 = CARTESIAN_POINT ( 'NONE',  ( -22.73457742531305925, 137.3553536570635742, -0.3842032436244983695 ) ) ;
#4620 = EDGE_LOOP ( 'NONE', ( #37823, #14152, #10989, #35771, #65 ) ) ;
#4621 = CARTESIAN_POINT ( 'NONE',  ( -46.94769949131580233, 25.36820868695422604, -1.370102228390909005 ) ) ;
#4622 = CARTESIAN_POINT ( 'NONE',  ( 7.870661077993043264, 122.2665614860925416, -0.4372302326949743523 ) ) ;
#4623 = DIRECTION ( 'NONE',  ( 0.8745520943968249084, -0.4849315768086533418, 5.271987356194193006E-16 ) ) ;
#4624 = EDGE_LOOP ( 'NONE', ( #40451, #32785, #13588, #1752 ) ) ;
#4625 = DIRECTION ( 'NONE',  ( 5.188838149069472160E-16, -1.699382548006136559E-16, -1.000000000000000000 ) ) ;
#4626 = CARTESIAN_POINT ( 'NONE',  ( -15.32629999177647662, 148.0267799683202554, -0.7554886701871539323 ) ) ;
#4627 = CARTESIAN_POINT ( 'NONE',  ( 3.665585082022325025, -14.37195162699216056, 4.995470683262428935 ) ) ;
#4628 = CARTESIAN_POINT ( 'NONE',  ( -18.33177592110340370, 128.6097515361309149, 1.108544906447614720 ) ) ;
#4629 = DIRECTION ( 'NONE',  ( -1.000000000000000000, -6.353134868986659519E-16, 0.000000000000000000 ) ) ;
#4630 = CARTESIAN_POINT ( 'NONE',  ( 18.61947985292891872, 154.1412379532633850, 0.5163013828871976241 ) ) ;
#4631 = ORIENTED_EDGE ( 'NONE', *, *, #24776, .F. ) ;
#4632 = CARTESIAN_POINT ( 'NONE',  ( 1.968029828064305153, -3.592386099649644837, 4.203610184747879508 ) ) ;
#4633 = CARTESIAN_POINT ( 'NONE',  ( -23.41829197008364360, 142.8308675865925181, -0.4933589455792335432 ) ) ;
#4634 = CARTESIAN_POINT ( 'NONE',  ( -41.81365047723964068, 22.72037957756173654, -1.583806717505435335 ) ) ;
#4635 = FACE_OUTER_BOUND ( 'NONE', #37201, .T. ) ;
#4636 = ORIENTED_EDGE ( 'NONE', *, *, #22473, .F. ) ;
#4637 = CARTESIAN_POINT ( 'NONE',  ( -8.259150402946779934, 120.4370358907085716, 1.103988885813925958 ) ) ;
#4638 = CARTESIAN_POINT ( 'NONE',  ( -0.6580430243309095539, -8.493043821084315326, 4.585212396833119541 ) ) ;
#4639 = CARTESIAN_POINT ( 'NONE',  ( 7.493104803958843263, 158.4854300789945398, 1.293057490532128373 ) ) ;
#4640 = CARTESIAN_POINT ( 'NONE',  ( -51.96382246822415851, 12.83266463568538285, -4.369925997638347326 ) ) ;
#4641 = CARTESIAN_POINT ( 'NONE',  ( 20.61281631175392093, 145.6130255286810495, -1.629730044589046578 ) ) ;
#4642 = CARTESIAN_POINT ( 'NONE',  ( -4.227217475240903077, -11.31673468295422147, -1.889206449475258509 ) ) ;
#4643 = CARTESIAN_POINT ( 'NONE',  ( -14.55652921886118811, 120.9595740141730289, -1.205336527378881195 ) ) ;
#4644 = ADVANCED_FACE ( 'NONE', ( #14853 ), #19824, .T. ) ;
#4645 = ORIENTED_EDGE ( 'NONE', *, *, #41983, .F. ) ;
#4646 = ORIENTED_EDGE ( 'NONE', *, *, #13888, .F. ) ;
#4647 = CARTESIAN_POINT ( 'NONE',  ( -14.72002613302119656, 148.8393470518043955, 0.03138755845351943324 ) ) ;
#4648 = CARTESIAN_POINT ( 'NONE',  ( 3.844517683078125803, -15.15487594273597161, 5.256808347261554104 ) ) ;
#4649 = DIRECTION ( 'NONE',  ( -0.000000000000000000, -0.000000000000000000, 1.000000000000000000 ) ) ;
#4650 = STYLED_ITEM ( 'NONE', ( #13892 ), #38189 ) ;
#4651 = CARTESIAN_POINT ( 'NONE',  ( -5.167152973807009886, 114.8006916078235378, -1.419485145312306962 ) ) ;
#4652 = VERTEX_POINT ( 'NONE', #11450 ) ;
#4653 = CARTESIAN_POINT ( 'NONE',  ( 18.41451321397395802, 140.7300538122508726, 2.503121031321716483 ) ) ;
#4654 = PLANE ( 'NONE',  #33813 ) ;
#4655 = LINE ( 'NONE', #39588, #19137 ) ;
#4656 = CIRCLE ( 'NONE', #30386, 0.5080000000000000071 ) ;
#4657 = CARTESIAN_POINT ( 'NONE',  ( -16.19941014871838547, 155.1612327564137388, 0.8792224148362003389 ) ) ;
#4658 = CARTESIAN_POINT ( 'NONE',  ( -1.148743315670426535, 1.199490873200159013, 8.378133985588048560 ) ) ;
#4659 = CARTESIAN_POINT ( 'NONE',  ( 9.839787852217051878, 124.1914461168675530, 0.8951504484210820456 ) ) ;
#4660 = CYLINDRICAL_SURFACE ( 'NONE', #21938, 16.60960244842765832 ) ;
#4661 = CARTESIAN_POINT ( 'NONE',  ( 3.828842504638720445, 116.8938343318378088, -0.2916468201809273020 ) ) ;
#4662 = DIRECTION ( 'NONE',  ( 0.000000000000000000, 0.000000000000000000, 1.000000000000000000 ) ) ;
#4663 = CARTESIAN_POINT ( 'NONE',  ( -55.74547202057183881, 5.289068369273755010, 2.605933947425615571 ) ) ;
#4664 = CYLINDRICAL_SURFACE ( 'NONE', #23469, 5.588000000000006295 ) ;
#4665 = CARTESIAN_POINT ( 'NONE',  ( -57.15088083682995546, 2.378576142695001838, 1.865916551128045553 ) ) ;
#4666 = CARTESIAN_POINT ( 'NONE',  ( -56.86472485052055248, 3.482560045344686994, 2.276423594962388997 ) ) ;
#4667 = CARTESIAN_POINT ( 'NONE',  ( -4.261598188410213872, 118.2248179704908182, 0.2974968183558716062 ) ) ;
#4668 = CARTESIAN_POINT ( 'NONE',  ( 0.4041248631678749925, 105.7854974534225221, -5.326937287149722700 ) ) ;
#4669 = ORIENTED_EDGE ( 'NONE', *, *, #32717, .T. ) ;
#4670 = LINE ( 'NONE', #7231, #13818 ) ;
#4671 =( BOUNDED_CURVE ( )  B_SPLINE_CURVE ( 3, ( #10896, #21100, #11739, #14292 ),
 .UNSPECIFIED., .F., .F. ) 
 B_SPLINE_CURVE_WITH_KNOTS ( ( 4, 4 ),
 ( 0.4253411113690419576, 0.4854033284062813647 ),
 .UNSPECIFIED. ) 
 CURVE ( )  GEOMETRIC_REPRESENTATION_ITEM ( )  RATIONAL_B_SPLINE_CURVE ( ( 0.7459560426888018903, 0.8021233807506140678, 0.8679106385868964324, 0.9433178161976487619 ) ) 
 REPRESENTATION_ITEM ( '' )  );
#4672 = CARTESIAN_POINT ( 'NONE',  ( 6.222678124517797116, 119.6959855836942523, -0.9950030739501369847 ) ) ;
#4673 = CARTESIAN_POINT ( 'NONE',  ( -5.045732318125732085, 114.3381464724725447, -1.964647476694348027 ) ) ;
#4674 = CARTESIAN_POINT ( 'NONE',  ( 4.444225408500467545, 118.1580887933540254, 0.6034175566067268015 ) ) ;
#4675 = CARTESIAN_POINT ( 'NONE',  ( -10.26858343235357829, 124.8461398015159745, -0.9314245544334064375 ) ) ;
#4676 = PRESENTATION_STYLE_ASSIGNMENT (( #33848 ) ) ;
#4677 = CARTESIAN_POINT ( 'NONE',  ( 2.017207601148263141, 117.3993839199529390, -1.370552602517844276 ) ) ;
#4678 = ORIENTED_EDGE ( 'NONE', *, *, #38324, .F. ) ;
#4679 = CARTESIAN_POINT ( 'NONE',  ( 7.694663930960251363, 124.9344662015457317, 0.1537576976229973746 ) ) ;
#4680 = CARTESIAN_POINT ( 'NONE',  ( -16.72040787068460332, 146.6545634508490821, -1.779279871595183637 ) ) ;
#4681 = CARTESIAN_POINT ( 'NONE',  ( 5.336610043934060243, 104.6144662015457527, -0.07732958313162717479 ) ) ;
#4682 = CARTESIAN_POINT ( 'NONE',  ( -44.26155013454228992, 21.23036713626273553, 2.970720547513075793 ) ) ;
#4683 = LINE ( 'NONE', #17640, #17428 ) ;
#4684 = CARTESIAN_POINT ( 'NONE',  ( -6.518479118499084457, 121.7796321915099469, -0.01654800507752220151 ) ) ;
#4685 = CIRCLE ( 'NONE', #5385, 6.349999999999999645 ) ;
#4686 = DIRECTION ( 'NONE',  ( 0.000000000000000000, 0.000000000000000000, -1.000000000000000000 ) ) ;
#4687 = CARTESIAN_POINT ( 'NONE',  ( 3.843811238687773191, 117.0275016673472663, 0.5328274117395520593 ) ) ;
#4688 = CARTESIAN_POINT ( 'NONE',  ( -28.92060043785469503, 77.33101988233063651, -1.270000000000007789 ) ) ;
#4690 = CARTESIAN_POINT ( 'NONE',  ( 21.77700140173205057, 149.0176745010074342, -1.274060564799276651 ) ) ;
#4689 = CARTESIAN_POINT ( 'NONE',  ( 3.205191379615736746, -14.47393913169138102, 3.051678166811226500 ) ) ;
#4691 = CARTESIAN_POINT ( 'NONE',  ( -4.236690124160904070, 119.4047208153655646, 0.8054972593864423436 ) ) ;
#4692 = CIRCLE ( 'NONE', #7415, 3.175000000000001155 ) ;
#4693 = CARTESIAN_POINT ( 'NONE',  ( -0.9740112296533943725, -11.51769927068266419, -0.01433540041261589619 ) ) ;
#4694 = CARTESIAN_POINT ( 'NONE',  ( -22.53452490051039803, 150.3096427868838987, -1.298398843693310045 ) ) ;
#4695 = CARTESIAN_POINT ( 'NONE',  ( 0.8462494346447723137, 11.68649857616015275, 0.4938625092760188795 ) ) ;
#4696 = ORIENTED_EDGE ( 'NONE', *, *, #2710, .F. ) ;
#4697 = ADVANCED_FACE ( 'NONE', ( #2315 ), #15275, .T. ) ;
#4698 = CARTESIAN_POINT ( 'NONE',  ( -48.84381969468221030, 17.12102923570560975, 3.921819500614938558 ) ) ;
#4699 = SHAPE_DEFINITION_REPRESENTATION ( #16363, #19076 ) ;
#4700 = CARTESIAN_POINT ( 'NONE',  ( -3.658657848224285747, 120.8687762150871379, 0.2216941123881817910 ) ) ;
#4701 = CARTESIAN_POINT ( 'NONE',  ( 4.980517673276738222, -11.70649569897110709, 0.6972323075040541829 ) ) ;
#4702 = CARTESIAN_POINT ( 'NONE',  ( 0.008308630153144203057, 120.0570981805881559, -0.4157978282972240591 ) ) ;
#4703 = ORIENTED_EDGE ( 'NONE', *, *, #22711, .F. ) ;
#4704 = EDGE_CURVE ( 'NONE', #10936, #33175, #39589, .T. ) ;
#4705 = CYLINDRICAL_SURFACE ( 'NONE', #30196, 0.2540000000000028901 ) ;
#4706 = CARTESIAN_POINT ( 'NONE',  ( 3.402052537932679588, -13.50846463298115196, 2.481730329246660371 ) ) ;
#4707 = CARTESIAN_POINT ( 'NONE',  ( -4.881263862402589027, 117.4111615705287477, -1.144645852924967455 ) ) ;
#4708 = CARTESIAN_POINT ( 'NONE',  ( 2.899431565053843141, 156.0891579660883508, -0.02704053119243710751 ) ) ;
#4709 = ORIENTED_EDGE ( 'NONE', *, *, #31004, .F. ) ;
#4710 = CARTESIAN_POINT ( 'NONE',  ( -0.01111639779270567722, 118.2594330468507593, 0.5563100024230162033 ) ) ;
#4711 = CARTESIAN_POINT ( 'NONE',  ( 4.304948217593230098, 111.0465000999332830, 3.212748056633830895 ) ) ;
#4712 = DIRECTION ( 'NONE',  ( -0.8745520943968126959, 0.4849315768086755463, -5.691349986800565628E-16 ) ) ;
#4713 = CARTESIAN_POINT ( 'NONE',  ( -5.348924234571052594, 56.51499999999999346, -4.492130288940743732 ) ) ;
#4714 = CARTESIAN_POINT ( 'NONE',  ( 15.38960455597340626, 120.6961994932685798, 0.07768288530491213040 ) ) ;
#4715 = AXIS2_PLACEMENT_3D ( 'NONE', #25289, #37440, #5925 ) ;
#4716 = DIRECTION ( 'NONE',  ( -0.8745520943968232430, 0.4849315768086567280, -4.878299988686192207E-16 ) ) ;
#4717 = TOROIDAL_SURFACE ( 'NONE', #35987, 0.7620000000000000107, 0.2540000000000000036 ) ;
#4718 = CARTESIAN_POINT ( 'NONE',  ( 1.705331049022388745, -15.56171815815048021, 5.564216269553816652 ) ) ;
#4719 = CARTESIAN_POINT ( 'NONE',  ( -11.24191166894635430, 82.34025985790688651, 1.523999999999999799 ) ) ;
#4720 = CARTESIAN_POINT ( 'NONE',  ( -4.881326591836633533, 117.7576924424856486, -0.7323402894751116499 ) ) ;
#4721 = CARTESIAN_POINT ( 'NONE',  ( 2.184917017309174536, 118.1205262787358663, 0.7523320384000313776 ) ) ;
#4722 = ORIENTED_EDGE ( 'NONE', *, *, #18578, .F. ) ;
#4723 = CARTESIAN_POINT ( 'NONE',  ( 4.095665791538102063, 15.60827804425945331, 7.401523448874606892 ) ) ;
#4724 = ADVANCED_FACE ( 'NONE', ( #34893 ), #31665, .F. ) ;
#4725 = CARTESIAN_POINT ( 'NONE',  ( -5.507127385143735232, 117.8102281818942458, -1.047516571110145511 ) ) ;
#4726 = CARTESIAN_POINT ( 'NONE',  ( -4.014846287426898641, 122.0441497943765370, -0.2789485273175660307 ) ) ;
#4727 = CARTESIAN_POINT ( 'NONE',  ( 4.844604166567388681, 117.7309004960029171, 0.9915350356305726587 ) ) ;
#4728 = CARTESIAN_POINT ( 'NONE',  ( -19.86616884172038766, 72.62886460123898758, -1.524000000000002242 ) ) ;
#4729 = CARTESIAN_POINT ( 'NONE',  ( -4.780815387031786656, 104.6144662015457527, 0.7323460767296593454 ) ) ;
#4730 = CARTESIAN_POINT ( 'NONE',  ( -4.274281473441157608, 3.541781053574249327, 1.790774723582081451 ) ) ;
#4731 = DIRECTION ( 'NONE',  ( 0.000000000000000000, 0.000000000000000000, -1.000000000000000000 ) ) ;
#4732 = CARTESIAN_POINT ( 'NONE',  ( -2.928647764479141102, 107.6119852313951526, -4.449003297184745520 ) ) ;
#4733 = CARTESIAN_POINT ( 'NONE',  ( 3.297440819997984107, -14.19009280176566890, 4.446257544676719853 ) ) ;
#4734 = CARTESIAN_POINT ( 'NONE',  ( 3.145827930497913538, 117.0475107411037641, -1.097865318250619726 ) ) ;
#4735 = CARTESIAN_POINT ( 'NONE',  ( 0.9281906404964566093, 34.59732502943162302, 2.863135987906454183 ) ) ;
#4736 = CARTESIAN_POINT ( 'NONE',  ( -2.052054811892178421, 115.7029480924404226, 1.635839580152672390 ) ) ;
#4737 = ORIENTED_EDGE ( 'NONE', *, *, #1368, .T. ) ;
#4738 = CARTESIAN_POINT ( 'NONE',  ( -4.506737449472459467, 104.6144662015545350, -2.874441546340825049 ) ) ;
#4739 = CARTESIAN_POINT ( 'NONE',  ( 2.422525963563016749, -15.70080278133445617, 5.253054914258033392 ) ) ;
#4740 = CARTESIAN_POINT ( 'NONE',  ( -10.86053312202636079, 155.9024031350590462, 1.736732359437422879 ) ) ;
#4741 = CARTESIAN_POINT ( 'NONE',  ( 0.1338929724787690234, 25.55936205620983515, 0.9658879472844225100 ) ) ;
#4742 = EDGE_CURVE ( 'NONE', #19837, #2010, #28587, .T. ) ;
#4743 = EDGE_LOOP ( 'NONE', ( #34011, #26760, #15171, #23379, #37037, #37261 ) ) ;
#4744 = ORIENTED_EDGE ( 'NONE', *, *, #13947, .T. ) ;
#4745 = CARTESIAN_POINT ( 'NONE',  ( -22.98045850745951313, 78.35500052582088415, 1.269999999999994245 ) ) ;
#4746 = CARTESIAN_POINT ( 'NONE',  ( 4.584725329087942391, 124.7699485019152945, 0.09621079440654298209 ) ) ;
#4747 = CARTESIAN_POINT ( 'NONE',  ( -14.42666092703575664, 134.5679602169015254, 1.107736707283931032 ) ) ;
#4748 = LINE ( 'NONE', #1551, #15031 ) ;
#4749 = AXIS2_PLACEMENT_3D ( 'NONE', #38301, #9325, #2105 ) ;
#4750 = CARTESIAN_POINT ( 'NONE',  ( 4.541578696478873134, 118.0696556320928181, -0.6340941426453600149 ) ) ;
#4751 = CARTESIAN_POINT ( 'NONE',  ( 11.32523555543259697, 123.0403929720162495, -1.197004354367267931 ) ) ;
#4752 = CIRCLE ( 'NONE', #28528, 12.69999999999999751 ) ;
#4753 = CARTESIAN_POINT ( 'NONE',  ( -14.56794066961899148, 154.5799843816573684, -2.217559120334770650 ) ) ;
#4754 = DIRECTION ( 'NONE',  ( 0.8745520943968243532, -0.4849315768086547296, 6.829619984160642269E-16 ) ) ;
#4755 = EDGE_LOOP ( 'NONE', ( #40689, #38715, #8803, #166, #26044, #3509 ) ) ;
#4756 = CARTESIAN_POINT ( 'NONE',  ( 4.316099701937201161, 118.2124166868408111, -0.3255499669043997457 ) ) ;
#4757 = ADVANCED_FACE ( 'NONE', ( #9407 ), #32017, .T. ) ;
#4758 = CARTESIAN_POINT ( 'NONE',  ( 14.45325548908953728, 139.0941462050048187, -0.3122831254358888198 ) ) ;
#4759 = EDGE_LOOP ( 'NONE', ( #9421, #36492, #4631, #5176 ) ) ;
#4760 = CARTESIAN_POINT ( 'NONE',  ( 3.092642723064080279, -14.67800799544728285, 3.675123631970977911 ) ) ;
#4761 = CARTESIAN_POINT ( 'NONE',  ( 11.48503488083538926, 55.92196062030127024, -5.016500000000110759 ) ) ;
#4762 = CARTESIAN_POINT ( 'NONE',  ( -51.96382246819224093, 12.83266463571058580, 4.369925997604237722 ) ) ;
#4763 = CARTESIAN_POINT ( 'NONE',  ( -0.7749869142727341398, -12.81603963768374044, -4.556214072895795830 ) ) ;
#4764 = CARTESIAN_POINT ( 'NONE',  ( 10.50156301541547244, 123.3532649940754027, 1.413946074136436692 ) ) ;
#4765 = CARTESIAN_POINT ( 'NONE',  ( -2.808975559516362797, 29.02362447754844865, 0.3931306422602618977 ) ) ;
#4766 = CARTESIAN_POINT ( 'NONE',  ( -4.883585300477498947, 117.2937442104795593, 0.7242188414070882541 ) ) ;
#4767 = CARTESIAN_POINT ( 'NONE',  ( 3.102408547967445696, -0.5812848888516047863, -3.453265078539196509 ) ) ;
#4768 = CARTESIAN_POINT ( 'NONE',  ( -0.0005023639978857188547, 120.9974662015457056, 0.02514034870427548501 ) ) ;
#4769 = CARTESIAN_POINT ( 'NONE',  ( -46.91947222136995066, 25.25986047197467599, 1.801467191766157327 ) ) ;
#4770 = EDGE_CURVE ( 'NONE', #35416, #37188, #30059, .T. ) ;
#4771 = AXIS2_PLACEMENT_3D ( 'NONE', #25997, #3229, #6216 ) ;
#4772 = AXIS2_PLACEMENT_3D ( 'NONE', #12478, #5465, #1848 ) ;
#4773 = CARTESIAN_POINT ( 'NONE',  ( -57.35932467317038430, 1.578336987915054834, -0.2403330148844060599 ) ) ;
#4774 = CARTESIAN_POINT ( 'NONE',  ( 8.794618831136583381, 117.7206556621920299, -0.02516188889388990338 ) ) ;
#4775 = CARTESIAN_POINT ( 'NONE',  ( 0.004379098345483538150, 122.8649044353672934, -0.2191479880733794572 ) ) ;
#4776 = CARTESIAN_POINT ( 'NONE',  ( -17.14500000000466784, 71.11999999999886768, -1.270000000000000684 ) ) ;
#4777 = FACE_OUTER_BOUND ( 'NONE', #41919, .T. ) ;
#4778 = CARTESIAN_POINT ( 'NONE',  ( -5.591489108514605455, 77.73497692594764885, -1.523999999999996025 ) ) ;
#4779 = CARTESIAN_POINT ( 'NONE',  ( -2.166771814436331045, 10.43868160547798674, -8.139002505017437272 ) ) ;
#4780 = ADVANCED_FACE ( 'NONE', ( #33684 ), #34100, .T. ) ;
#4781 = CARTESIAN_POINT ( 'NONE',  ( -5.322311914403968558, 56.51500000000043400, 5.239113282919425352 ) ) ;
#4782 = DIRECTION ( 'NONE',  ( -0.9998004120163608288, 0.000000000000000000, -0.01997839162482747608 ) ) ;
#4783 = CARTESIAN_POINT ( 'NONE',  ( -58.16194989728257525, 1.772972946764567181, 0.08436090182516464697 ) ) ;
#4784 = CARTESIAN_POINT ( 'NONE',  ( 0.01386859376319274882, 119.8383472832138779, -0.6940411431075989013 ) ) ;
#4785 = CARTESIAN_POINT ( 'NONE',  ( -22.77159426375468243, 150.3871190066015799, -0.004147128915567659807 ) ) ;
#4786 = ORIENTED_EDGE ( 'NONE', *, *, #4211, .F. ) ;
#4787 = CARTESIAN_POINT ( 'NONE',  ( -57.80205714066466527, 2.371715784325115095, -1.753227392946310026 ) ) ;
#4788 = ORIENTED_EDGE ( 'NONE', *, *, #19029, .F. ) ;
#4789 = CARTESIAN_POINT ( 'NONE',  ( -44.81960200543956319, 21.09415034429482461, -3.442746975522120945 ) ) ;
#4790 = CARTESIAN_POINT ( 'NONE',  ( -14.16569067496518564, 138.8670163227233161, -0.2830642121559646673 ) ) ;
#4791 = CARTESIAN_POINT ( 'NONE',  ( 3.639791848495840476, -15.36872039720094207, 5.326864320309495859 ) ) ;
#4792 = CARTESIAN_POINT ( 'NONE',  ( -20.46179744412678758, 141.4490678312372722, 1.579512522682919418 ) ) ;
#4793 = CARTESIAN_POINT ( 'NONE',  ( 14.96856157597580150, 121.5307057168427605, -0.7335553340177136672 ) ) ;
#4794 = CARTESIAN_POINT ( 'NONE',  ( 1.111903444298625754, 15.29877551736591812, 4.515507465039587665 ) ) ;
#4795 = CARTESIAN_POINT ( 'NONE',  ( -10.79372094067549526, 157.9251727141802633, -0.3940533352873706874 ) ) ;
#4796 = CARTESIAN_POINT ( 'NONE',  ( -49.70193759272228107, 16.76737306193518151, -4.987092963739070406 ) ) ;
#4797 = ORIENTED_EDGE ( 'NONE', *, *, #35842, .F. ) ;
#4798 = CARTESIAN_POINT ( 'NONE',  ( 8.793348182195531493, 117.6962994879057334, 0.2883727696902242954 ) ) ;
#4799 = CARTESIAN_POINT ( 'NONE',  ( -11.03120429849349193, 123.2082810311540300, 1.124825114493487543 ) ) ;
#4800 = CARTESIAN_POINT ( 'NONE',  ( -56.17224506125053551, 4.400912353714958591, -2.358402907739791221 ) ) ;
#4801 = CARTESIAN_POINT ( 'NONE',  ( 18.78250995143891089, 149.1225091032880528, -1.736135053443003784 ) ) ;
#4802 = CARTESIAN_POINT ( 'NONE',  ( -20.19347568108163671, 136.2683111393718320, -2.155148867324337303 ) ) ;
#4803 = CARTESIAN_POINT ( 'NONE',  ( -44.90991502375803890, 23.16658271142636139, -2.247441098035906748 ) ) ;
#4804 = EDGE_CURVE ( 'NONE', #28149, #21592, #10993, .T. ) ;
#4805 = CARTESIAN_POINT ( 'NONE',  ( 9.788763933236980463, 123.8372022493589100, -0.5907035020478675902 ) ) ;
#4806 = DIRECTION ( 'NONE',  ( -0.8745520943968235761, 0.4849315768086558398, -8.537024980200821818E-16 ) ) ;
#4807 = EDGE_LOOP ( 'NONE', ( #6821, #24873, #35145, #39081 ) ) ;
#4808 = CARTESIAN_POINT ( 'NONE',  ( -0.8917109795615992818, 157.3234082283764792, -1.558336142952463810 ) ) ;
#4809 = CARTESIAN_POINT ( 'NONE',  ( 4.514867502249738429, -15.46117574218924773, 1.158286244139274279 ) ) ;
#4810 = CARTESIAN_POINT ( 'NONE',  ( -4.491279449957480630, 118.0838085148757841, -0.7971429151108968547 ) ) ;
#4811 = CARTESIAN_POINT ( 'NONE',  ( -53.00789483126595769, 12.40033530745290236, -4.180047681284821515 ) ) ;
#4812 = DIRECTION ( 'NONE',  ( -5.188838149069472160E-16, 1.699382548006136559E-16, 1.000000000000000000 ) ) ;
#4813 = CARTESIAN_POINT ( 'NONE',  ( 5.835695000730356519, 120.1673030736515955, 1.074193948046630709 ) ) ;
#4814 = ADVANCED_FACE ( 'NONE', ( #8101 ), #32652, .T. ) ;
#4815 = LINE ( 'NONE', #31185, #6312 ) ;
#4816 = CARTESIAN_POINT ( 'NONE',  ( 20.69815783549627497, 152.5608647341385335, 0.3383848979192933260 ) ) ;
#4817 = AXIS2_PLACEMENT_3D ( 'NONE', #13260, #32862, #30078 ) ;
#4818 = CARTESIAN_POINT ( 'NONE',  ( -6.605212570472872358, 13.46189590645272460, 5.224192399652773489 ) ) ;
#4819 = CARTESIAN_POINT ( 'NONE',  ( 2.769557799161845857, 120.9068798055765370, 0.2367794989410801354 ) ) ;
#4820 = CARTESIAN_POINT ( 'NONE',  ( 4.801338745261147345, 117.3993836135855275, -1.016148444996444189 ) ) ;
#4821 = EDGE_CURVE ( 'NONE', #4600, #39773, #30674, .T. ) ;
#4822 = CARTESIAN_POINT ( 'NONE',  ( -15.37877921309976870, 79.99470228764801050, -1.270000000000001350 ) ) ;
#4823 = AXIS2_PLACEMENT_3D ( 'NONE', #40329, #27316, #34139 ) ;
#4824 = CARTESIAN_POINT ( 'NONE',  ( -15.27962295839633811, 80.49293118800726177, 1.269999999999997797 ) ) ;
#4825 = EDGE_CURVE ( 'NONE', #4233, #5241, #11691, .T. ) ;
#4826 = CARTESIAN_POINT ( 'NONE',  ( -57.61542428582638564, 1.103772655929896596, 0.1998674755708474138 ) ) ;
#4827 = CARTESIAN_POINT ( 'NONE',  ( -21.64725176087522840, 132.7051459832101443, -0.3678724904816468300 ) ) ;
#4828 = ORIENTED_EDGE ( 'NONE', *, *, #30807, .F. ) ;
#4829 = CARTESIAN_POINT ( 'NONE',  ( -46.60530155212501313, 26.17382724835480445, -0.9172222222222309318 ) ) ;
#4830 = CARTESIAN_POINT ( 'NONE',  ( -6.848981279076908457, 121.5714736848644861, -0.7266479796884791620 ) ) ;
#4831 = DIRECTION ( 'NONE',  ( 0.9998004120163609398, 0.000000000000000000, 0.01997839162482749689 ) ) ;
#4832 = ORIENTED_EDGE ( 'NONE', *, *, #30047, .F. ) ;
#4833 = CARTESIAN_POINT ( 'NONE',  ( 0.6269658669242333948, 115.7029626408947536, -1.737418004581801290 ) ) ;
#4834 = CARTESIAN_POINT ( 'NONE',  ( -15.80138807371441523, 145.9351319680867221, -0.6472794460535241656 ) ) ;
#4835 = CARTESIAN_POINT ( 'NONE',  ( 3.288375567735513094, -14.78372392556953585, 5.458595067156710279 ) ) ;
#4836 = CARTESIAN_POINT ( 'NONE',  ( -0.3953301572312742929, 117.5049145548240972, 0.4632619789290193246 ) ) ;
#4837 = CARTESIAN_POINT ( 'NONE',  ( -3.841520934845505941, 71.62889921741444255, -1.269999999999994023 ) ) ;
#4838 = CARTESIAN_POINT ( 'NONE',  ( 8.055701656131518007, 158.6724238832827609, 0.2706798611393589904 ) ) ;
#4839 = CARTESIAN_POINT ( 'NONE',  ( 8.901366582544378403, 123.9008345302928120, 0.2219616208084491948 ) ) ;
#4840 = ORIENTED_EDGE ( 'NONE', *, *, #29765, .F. ) ;
#4841 = CARTESIAN_POINT ( 'NONE',  ( 0.9475510003767251277, 17.78785052102138664, 0.2306771022979090535 ) ) ;
#4842 = CARTESIAN_POINT ( 'NONE',  ( -5.755000932441543426, 159.1151184437813981, -0.1316611545253205395 ) ) ;
#4843 = CARTESIAN_POINT ( 'NONE',  ( -41.95243232931379396, 22.60620181788836192, -1.619729722610462552 ) ) ;
#4844 = FACE_OUTER_BOUND ( 'NONE', #16542, .T. ) ;
#4845 = ORIENTED_EDGE ( 'NONE', *, *, #10234, .T. ) ;
#4846 = CARTESIAN_POINT ( 'NONE',  ( 3.037128892075650288, 117.4034716445605540, 0.7578594852576387986 ) ) ;
#4847 = CARTESIAN_POINT ( 'NONE',  ( 3.440871586586784492, -6.993729544307833557, 3.087053954803492317 ) ) ;
#4848 = CARTESIAN_POINT ( 'NONE',  ( 3.949038439882183837, 117.6225627337916393, 0.7921763187007300200 ) ) ;
#4849 = CARTESIAN_POINT ( 'NONE',  ( -58.27365357892946918, 0.4699239364167467903, -1.042275140646608422 ) ) ;
#4850 = CARTESIAN_POINT ( 'NONE',  ( 4.664640489119654454, 158.0471523224993859, -1.621167461353164585 ) ) ;
#4851 = CARTESIAN_POINT ( 'NONE',  ( -3.263082884110522386, 19.99377609092593389, 7.766292582686701529 ) ) ;
#4852 = CARTESIAN_POINT ( 'NONE',  ( -22.54389841724633570, 148.7221180073953235, -1.757920738659724647 ) ) ;
#4853 = CARTESIAN_POINT ( 'NONE',  ( 4.945934694223368844, 117.6258612243657637, -0.7624269308906101994 ) ) ;
#4854 = CIRCLE ( 'NONE', #10926, 7.461249999999999716 ) ;
#4855 = ORIENTED_EDGE ( 'NONE', *, *, #738, .T. ) ;
#4856 = CARTESIAN_POINT ( 'NONE',  ( -9.310784039460543227, 124.2035065715909496, 0.04725383350292546719 ) ) ;
#4857 = CARTESIAN_POINT ( 'NONE',  ( 2.079616623477898329, -15.54617723206731839, 5.925385729176050553 ) ) ;
#4858 = AXIS2_PLACEMENT_3D ( 'NONE', #41737, #21273, #2561 ) ;
#4859 = CYLINDRICAL_SURFACE ( 'NONE', #39009, 0.5080000000000007843 ) ;
#4860 = EDGE_CURVE ( 'NONE', #22153, #4943, #11292, .T. ) ;
#4861 = CARTESIAN_POINT ( 'NONE',  ( -3.610648906290234716, 109.1680670511277498, -3.931663264847707673 ) ) ;
#4862 = VERTEX_POINT ( 'NONE', #2141 ) ;
#4863 = CARTESIAN_POINT ( 'NONE',  ( 12.10717961583465652, 122.5392882283422864, 1.794329550371804194 ) ) ;
#4864 = CARTESIAN_POINT ( 'NONE',  ( -26.51793118801306548, 72.98537704160715123, 1.269999999999993134 ) ) ;
#4865 = DIRECTION ( 'NONE',  ( -0.6559537821943239866, 0.7548010569845283735, -4.686333752532408853E-16 ) ) ;
#4866 = CARTESIAN_POINT ( 'NONE',  ( -2.437154581274205256, 119.8248006784163380, 0.4733635836876309289 ) ) ;
#4867 = CARTESIAN_POINT ( 'NONE',  ( 8.368836169178564433, 3.587476746713724740, 1.217019533931793074 ) ) ;
#4868 = CARTESIAN_POINT ( 'NONE',  ( 11.15578272721372421, 126.1638007343821641, 1.112962985253807657 ) ) ;
#4869 = CARTESIAN_POINT ( 'NONE',  ( -27.97106122948731510, 77.87043919753004673, 1.269999999999991802 ) ) ;
#4870 = CARTESIAN_POINT ( 'NONE',  ( 0.3352962839983787968, 116.7787044104018861, -0.2500268678974714720 ) ) ;
#4871 = CARTESIAN_POINT ( 'NONE',  ( -5.332935397695336199, 105.1224662015457199, -0.1065647409268299373 ) ) ;
#4872 = CARTESIAN_POINT ( 'NONE',  ( -52.74846150007513046, 11.25334410283610254, 3.958079477545757729 ) ) ;
#4873 = CARTESIAN_POINT ( 'NONE',  ( -29.42319995517901887, 68.34872547562956413, -1.524000000000006239 ) ) ;
#4874 = AXIS2_PLACEMENT_3D ( 'NONE', #24102, #18330, #1964 ) ;
#4875 = EDGE_CURVE ( 'NONE', #32761, #22572, #32771, .T. ) ;
#4876 = CARTESIAN_POINT ( 'NONE',  ( -58.73801720703743001, -0.4998429216807459552, -1.049519136981926467E-14 ) ) ;
#4877 = CARTESIAN_POINT ( 'NONE',  ( -57.60796681880061243, 1.905299612284082400, 1.725903007441225601 ) ) ;
#4878 = LINE ( 'NONE', #8476, #18456 ) ;
#4879 = CARTESIAN_POINT ( 'NONE',  ( -4.316210094789089347, 118.2124209707147742, 0.3254998515997128417 ) ) ;
#4880 = CARTESIAN_POINT ( 'NONE',  ( 4.077454352797809989, 109.5187069194699632, -3.449181840922602049 ) ) ;
#4881 = ORIENTED_EDGE ( 'NONE', *, *, #36327, .F. ) ;
#4882 = CARTESIAN_POINT ( 'NONE',  ( -54.98111839650035648, 8.542840639972862249, 3.427624633821322320 ) ) ;
#4883 = CARTESIAN_POINT ( 'NONE',  ( -8.274239857666382036, 120.1145857019959209, -1.449899955590871592 ) ) ;
#4884 = CARTESIAN_POINT ( 'NONE',  ( -1.980401745281053172, 106.6864334246082961, -4.967395836420048560 ) ) ;
#4886 = CARTESIAN_POINT ( 'NONE',  ( 4.255616016246193567, 118.2236154135255930, 0.4577608436404123071 ) ) ;
#4885 = CIRCLE ( 'NONE', #4225, 0.2540000000000000036 ) ;
#4887 = CARTESIAN_POINT ( 'NONE',  ( 0.01133107913638299775, 156.3792106723807649, -0.5670535347366656431 ) ) ;
#4888 = CARTESIAN_POINT ( 'NONE',  ( 0.02983097934372052479, 117.3993836135855418, -1.492864285909942579 ) ) ;
#4889 = ORIENTED_EDGE ( 'NONE', *, *, #25853, .F. ) ;
#4890 = CARTESIAN_POINT ( 'NONE',  ( 1.893578447776079754, 19.08455809737888487, -4.224370802633358402 ) ) ;
#4891 = CARTESIAN_POINT ( 'NONE',  ( -7.898163624196860688, 121.8456834504061845, -1.011533665549599004 ) ) ;
#4892 = CARTESIAN_POINT ( 'NONE',  ( -4.466782427718574588, 71.06098887363195615, -1.523999999999994248 ) ) ;
#4893 = CARTESIAN_POINT ( 'NONE',  ( -47.73297240351937631, 19.53746995445935042, 5.217258361112828702 ) ) ;
#4894 = CARTESIAN_POINT ( 'NONE',  ( -41.05192305526440322, 23.09448250258610713, 1.270000000023969067 ) ) ;
#4895 = CARTESIAN_POINT ( 'NONE',  ( -9.014953340893313793, 124.1466903544668838, -0.04592658822908208399 ) ) ;
#4896 = CARTESIAN_POINT ( 'NONE',  ( 4.941652259254307289, 117.6448581155076880, -0.7476730690041486493 ) ) ;
#4897 = CARTESIAN_POINT ( 'NONE',  ( 10.42794149288025984, 157.8855781193960297, 1.079236549925195465 ) ) ;
#4898 = CARTESIAN_POINT ( 'NONE',  ( -6.350000000000053824, 83.56599999999998829, 7.776507174585703010E-16 ) ) ;
#4900 = CARTESIAN_POINT ( 'NONE',  ( 21.83857928711794116, 148.7205309135917730, -1.274413580488712006 ) ) ;
#4899 = CARTESIAN_POINT ( 'NONE',  ( 2.994295736468014280, -14.77441112906794984, 3.968895097548184037 ) ) ;
#4901 = CARTESIAN_POINT ( 'NONE',  ( -5.067974813687988522, 119.5555251685854330, 0.8659238720033423098 ) ) ;
#4902 = CIRCLE ( 'NONE', #25273, 0.5080000000000002292 ) ;
#4903 = CARTESIAN_POINT ( 'NONE',  ( -0.6538259107469485132, -10.21753563294075384, 0.7251761174241220242 ) ) ;
#4904 = CARTESIAN_POINT ( 'NONE',  ( -22.97411545401789468, 149.2143936249396461, -1.313106760764511050 ) ) ;
#4905 = CARTESIAN_POINT ( 'NONE',  ( 0.1179719058304127544, 10.27755972103446958, 0.9685762618712100425 ) ) ;
#4906 = EDGE_LOOP ( 'NONE', ( #26892, #32231, #22425, #41155 ) ) ;
#4907 = CARTESIAN_POINT ( 'NONE',  ( -51.86985193027732066, 10.34936321858913999, 0.3560079035464910335 ) ) ;
#4908 = CARTESIAN_POINT ( 'NONE',  ( -9.648208730819588297, 124.2480737032941533, 0.3321887029122945756 ) ) ;
#4909 = CARTESIAN_POINT ( 'NONE',  ( 3.665585082022325025, -14.37195162699216056, 4.995470683262428935 ) ) ;
#4910 = CARTESIAN_POINT ( 'NONE',  ( 10.84039127762408228, 123.6843197456346672, -1.011594478071749625 ) ) ;
#4911 = ORIENTED_EDGE ( 'NONE', *, *, #32619, .F. ) ;
#4912 = CIRCLE ( 'NONE', #19167, 3.175000000000001155 ) ;
#4913 = CARTESIAN_POINT ( 'NONE',  ( 0.5786556323373592825, 115.7029630015946111, 1.760570191192437628 ) ) ;
#4914 = VECTOR ( 'NONE', #23918, 1000.000000000000000 ) ;
#4915 = CARTESIAN_POINT ( 'NONE',  ( 3.387566103704702236, -13.77904243453481570, 2.987699908524332759 ) ) ;
#4916 = CARTESIAN_POINT ( 'NONE',  ( -4.940781816828488715, 117.5342059363709950, -0.9902978256015019243 ) ) ;
#4917 = CARTESIAN_POINT ( 'NONE',  ( 4.236260012103334915, 155.8470599587123502, -0.007037385900262056911 ) ) ;
#4918 = ORIENTED_EDGE ( 'NONE', *, *, #26356, .F. ) ;
#4919 = CARTESIAN_POINT ( 'NONE',  ( 3.146714701748970278, 118.3302933575512412, 0.8734028913305708075 ) ) ;
#4920 = CARTESIAN_POINT ( 'NONE',  ( 5.183445353050514015, 115.9099169135977974, 1.326074002626195680 ) ) ;
#4921 = CARTESIAN_POINT ( 'NONE',  ( -6.604303299200508256E-14, 94.83546620154572793, -1.207165459215201580E-19 ) ) ;
#4922 = CARTESIAN_POINT ( 'NONE',  ( 0.03212618750946916180, 158.2819368290249713, -1.607725792532325393 ) ) ;
#4923 = CARTESIAN_POINT ( 'NONE',  ( 8.215251585939698842, 117.5146787832509858, 0.03113046551775530690 ) ) ;
#4924 = CARTESIAN_POINT ( 'NONE',  ( 13.85159022459153988, 12.96416000000000146, 5.016499999999999737 ) ) ;
#4925 = CARTESIAN_POINT ( 'NONE',  ( 1.920772546426502192, -15.19580626328599671, 5.957450100407664983 ) ) ;
#4926 = CARTESIAN_POINT ( 'NONE',  ( -4.645572480595541620, 117.9340260526530813, 0.7769932229682322555 ) ) ;
#4927 = DIRECTION ( 'NONE',  ( -0.9998004120163608288, 0.000000000000000000, -0.01997839162482749342 ) ) ;
#4928 = CARTESIAN_POINT ( 'NONE',  ( -4.633588795532518567, 117.9522783733740567, 0.7617726623130426367 ) ) ;
#4929 = VERTEX_POINT ( 'NONE', #2571 ) ;
#4930 = CARTESIAN_POINT ( 'NONE',  ( 5.204330674627346554, 115.7029491485453150, -1.024362258486631649 ) ) ;
#4931 = CARTESIAN_POINT ( 'NONE',  ( 3.328596738436636393, 118.4670010328146503, -0.7846298696386536653 ) ) ;
#4932 = CARTESIAN_POINT ( 'NONE',  ( 0.1065646865915094166, 105.8844662015457061, -5.332932678536314697 ) ) ;
#4933 = CARTESIAN_POINT ( 'NONE',  ( 4.748484029138242413, 117.5371517732831421, 1.178549711470926020 ) ) ;
#4934 = CARTESIAN_POINT ( 'NONE',  ( -1.058771226886514372, 124.8229041592835387, -0.01153269281271720494 ) ) ;
#4935 = AXIS2_PLACEMENT_3D ( 'NONE', #41822, #18995, #38193 ) ;
#4936 = CARTESIAN_POINT ( 'NONE',  ( 1.398650104629075797, 0.06838872207683838189, -4.420329592304430122 ) ) ;
#4937 = CARTESIAN_POINT ( 'NONE',  ( 1.406077420118782567E-15, 14.60500000000000220, 0.000000000000000000 ) ) ;
#4938 = DIRECTION ( 'NONE',  ( -0.8745520943968235761, 0.4849315768086558953, -5.361993529360570985E-16 ) ) ;
#4939 = CARTESIAN_POINT ( 'NONE',  ( 3.022112892507086812, -12.39725416092116106, 0.4273193741429963666 ) ) ;
#4940 = CARTESIAN_POINT ( 'NONE',  ( 3.998592866256202694, 116.4303826247378026, -1.177299868075282641 ) ) ;
#4941 = CARTESIAN_POINT ( 'NONE',  ( 0.1238897909883466403, 36.81462384746927086, 2.295035569577275059 ) ) ;
#4942 = CARTESIAN_POINT ( 'NONE',  ( -2.044842387155601848, 115.7029490949802266, 1.636383577350578156 ) ) ;
#4943 = VERTEX_POINT ( 'NONE', #21481 ) ;
#4944 = CARTESIAN_POINT ( 'NONE',  ( -4.979428488236589345, 104.6144662015479412, -1.943962536390259954 ) ) ;
#4945 = CARTESIAN_POINT ( 'NONE',  ( 1.868457900240735103, -15.55086107261449690, 5.421086310357067894 ) ) ;
#4946 = CARTESIAN_POINT ( 'NONE',  ( -0.03245814172817860360, 158.1186941186938952, 1.624338139048501661 ) ) ;
#4947 = CARTESIAN_POINT ( 'NONE',  ( 0.6255416438669687551, 26.40915095058528905, 0.7518939258676016202 ) ) ;
#4948 = VERTEX_POINT ( 'NONE', #18930 ) ;
#4949 = CIRCLE ( 'NONE', #32138, 0.7619999999999969020 ) ;
#4950 = ORIENTED_EDGE ( 'NONE', *, *, #25311, .T. ) ;
#4951 = FACE_OUTER_BOUND ( 'NONE', #13212, .T. ) ;
#4952 = CARTESIAN_POINT ( 'NONE',  ( 4.364892838101803285, 123.4689364668338385, 0.1663115080531035461 ) ) ;
#4953 = CARTESIAN_POINT ( 'NONE',  ( -7.221579903134116130, 121.4526873951801633, 0.6561908252823553944 ) ) ;
#4954 = CARTESIAN_POINT ( 'NONE',  ( -6.096037513970406607, 78.08166987308820239, 1.524000000000003130 ) ) ;
#4955 = CARTESIAN_POINT ( 'NONE',  ( 4.584778834665758751, 118.0135720478281485, -0.7024323280929735125 ) ) ;
#4956 = CARTESIAN_POINT ( 'NONE',  ( 5.099922610523941024, 119.9665122172617231, -0.7872683264543846038 ) ) ;
#4957 = CARTESIAN_POINT ( 'NONE',  ( -4.088037439073751500, 118.5849532427036905, -0.9900007573961080443 ) ) ;
#4958 = DIRECTION ( 'NONE',  ( -0.8745520943968235761, 0.4849315768086558398, -4.268512490100410909E-16 ) ) ;
#4959 = ORIENTED_EDGE ( 'NONE', *, *, #15150, .T. ) ;
#4960 = CARTESIAN_POINT ( 'NONE',  ( 4.257727891021212407, 118.2250048574998829, -0.3017987544622640628 ) ) ;
#4961 = CARTESIAN_POINT ( 'NONE',  ( 2.758537940428885005, 120.8469057251343060, -0.1732774955029139363 ) ) ;
#4962 = ORIENTED_EDGE ( 'NONE', *, *, #26109, .T. ) ;
#4963 = CARTESIAN_POINT ( 'NONE',  ( 2.908198840139253338, -13.99431844974620454, 0.6722015529863232253 ) ) ;
#4964 = CARTESIAN_POINT ( 'NONE',  ( 12.21488373879589240, 55.24500000000000455, -5.016500000000000625 ) ) ;
#4965 = CIRCLE ( 'NONE', #34872, 0.6349999999999984546 ) ;
#4966 = B_SPLINE_CURVE_WITH_KNOTS ( 'NONE', 3,
 ( #27806, #40814, #8433, #12040, #18635, #20986, #11615, #28444, #5251, #37194 ),
 .UNSPECIFIED., .F., .F.,
 ( 4, 2, 2, 2, 4 ),
 ( -5.999999999942070351E-08, 0.0005999509680439210927, 0.001199961936087841612, 0.002399983872175682868, 0.004800027744351364513 ),
 .UNSPECIFIED. ) ;
#4967 = CARTESIAN_POINT ( 'NONE',  ( -57.93805369095628777, 0.6893004133205121731, 1.202053765808312802 ) ) ;
#4968 = CARTESIAN_POINT ( 'NONE',  ( 2.459658384930404118, -7.418532284756778949, 3.912982838641719141 ) ) ;
#4969 = CARTESIAN_POINT ( 'NONE',  ( 14.69551782889044489, 134.6798445586954927, 1.826766161810339462 ) ) ;
#4970 = CARTESIAN_POINT ( 'NONE',  ( 2.878515509655334093, 37.92758169195481344, 1.187197144508459701 ) ) ;
#4971 = CARTESIAN_POINT ( 'NONE',  ( -6.983131083342716927, 124.7321584522365896, -0.1385298619991067737 ) ) ;
#4972 = AXIS2_PLACEMENT_3D ( 'NONE', #8251, #2515, #11437 ) ;
#4973 = CARTESIAN_POINT ( 'NONE',  ( 1.961646697876492373, -0.1315482170498871728, -4.191205975169975950 ) ) ;
#4974 = CARTESIAN_POINT ( 'NONE',  ( 15.76280660274394663, 145.9085485750152316, 0.3664889719343316088 ) ) ;
#4975 = CARTESIAN_POINT ( 'NONE',  ( 5.239248437989107998, 115.6909491485453145, 1.024417804751308614 ) ) ;
#4976 = EDGE_CURVE ( 'NONE', #19939, #6797, #18714, .T. ) ;
#4977 = AXIS2_PLACEMENT_3D ( 'NONE', #37645, #18450, #15046 ) ;
#4978 = CARTESIAN_POINT ( 'NONE',  ( -57.89731077922510849, 0.5615449381113774008, -0.05962325924458922871 ) ) ;
#4979 = CARTESIAN_POINT ( 'NONE',  ( 8.784622439875429123, 117.7823766468853250, -0.1582906694335896591 ) ) ;
#4980 = CARTESIAN_POINT ( 'NONE',  ( 0.008700780993235806074, 121.2597428844645293, -0.4354226598341944809 ) ) ;
#4981 = CARTESIAN_POINT ( 'NONE',  ( -6.059261036834487690, 71.63300248836198136, -5.016499999999999737 ) ) ;
#4982 = DIRECTION ( 'NONE',  ( 5.188838149069472160E-16, -1.699382548006136559E-16, -1.000000000000000000 ) ) ;
#4983 = CARTESIAN_POINT ( 'NONE',  ( -3.044072069279135651, 34.44269722464345307, 3.574075509920750626 ) ) ;
#4984 = CARTESIAN_POINT ( 'NONE',  ( 0.8402904295469701967, 0.2923264105788614398, -8.379105243356319122 ) ) ;
#4985 = FACE_OUTER_BOUND ( 'NONE', #30038, .T. ) ;
#4986 = CARTESIAN_POINT ( 'NONE',  ( -15.23999999999999311, 71.11999999999999034, 5.714999999999998970 ) ) ;
#4987 = DIRECTION ( 'NONE',  ( -1.000000000000000000, 0.000000000000000000, 0.000000000000000000 ) ) ;
#4988 = CARTESIAN_POINT ( 'NONE',  ( 0.09221630143774380006, 107.6766875080336376, -4.614880812453306724 ) ) ;
#4989 = CARTESIAN_POINT ( 'NONE',  ( -20.57623859521469001, 152.5775223076369400, 0.1637982859500254906 ) ) ;
#4990 = VERTEX_POINT ( 'NONE', #18089 ) ;
#4991 = CARTESIAN_POINT ( 'NONE',  ( -58.83227707057483968, -0.08366279997992775996, -0.2458995907045100349 ) ) ;
#4992 = VERTEX_POINT ( 'NONE', #24695 ) ;
#4993 = CARTESIAN_POINT ( 'NONE',  ( -43.90699889932841415, 21.43881162649502770, -2.872437248222870387 ) ) ;
#4994 = AXIS2_PLACEMENT_3D ( 'NONE', #22748, #9988, #19993 ) ;
#4995 = CARTESIAN_POINT ( 'NONE',  ( -4.218275339060285845, 155.8585684991085714, -0.08429118021179402009 ) ) ;
#4996 = CARTESIAN_POINT ( 'NONE',  ( 3.586901592285024698, -15.56753269123677086, 5.192771612050266050 ) ) ;
#4997 = CARTESIAN_POINT ( 'NONE',  ( -1.193991991012630205, 158.7113841514841681, 1.470390664574136252 ) ) ;
#4998 = VECTOR ( 'NONE', #10634, 1000.000000000000000 ) ;
#4999 = CARTESIAN_POINT ( 'NONE',  ( 16.19941014871825402, 155.1612327564137388, -0.8792224148362001168 ) ) ;
#5000 = CARTESIAN_POINT ( 'NONE',  ( -0.8080508600641240768, 24.25718022715097888, 4.550674767031389401 ) ) ;
#5001 = CARTESIAN_POINT ( 'NONE',  ( -16.04055624107204636, 121.3766923467913585, -0.6455242483069041359 ) ) ;
#5002 = CARTESIAN_POINT ( 'NONE',  ( -49.20375664226762069, 17.53306181478205161, -5.082897273857148512 ) ) ;
#5003 = CARTESIAN_POINT ( 'NONE',  ( 8.792199711666244255, 117.7001252806687148, 0.3065861086990905870 ) ) ;
#5004 = CARTESIAN_POINT ( 'NONE',  ( 5.936184715466450434, 56.51500000000000057, 4.381499802638942676 ) ) ;
#5005 = CARTESIAN_POINT ( 'NONE',  ( -2.509025565091423715, 119.7126118883416410, 0.5998098196673843363 ) ) ;
#5006 = CARTESIAN_POINT ( 'NONE',  ( -53.88338131392961827, 9.054548675370849509, -3.507011937191574003 ) ) ;
#5007 = CARTESIAN_POINT ( 'NONE',  ( 0.5002616235672558975, 119.0154928070276412, -0.5875571981567377922 ) ) ;
#5008 = CARTESIAN_POINT ( 'NONE',  ( 0.02399864187730229442, 159.1630378086529731, -1.200990174154242141 ) ) ;
#5009 = CARTESIAN_POINT ( 'NONE',  ( -48.38589991294941939, 19.15920805527091630, -5.452675306770326635 ) ) ;
#5010 = AXIS2_PLACEMENT_3D ( 'NONE', #7418, #7626, #14203 ) ;
#5011 = EDGE_CURVE ( 'NONE', #18746, #4497, #25280, .T. ) ;
#5012 = CARTESIAN_POINT ( 'NONE',  ( 0.5989337510911817430, 120.4790399057546182, -0.3068722873270139928 ) ) ;
#5013 = ORIENTED_EDGE ( 'NONE', *, *, #29167, .F. ) ;
#5014 = CARTESIAN_POINT ( 'NONE',  ( -18.14277298170013708, 148.2327041560005512, -2.387153687107330224 ) ) ;
#5015 = CARTESIAN_POINT ( 'NONE',  ( 4.191701569836151720, -15.46661069841161229, 1.593937231346424843 ) ) ;
#5016 = CARTESIAN_POINT ( 'NONE',  ( -4.486916041353520512, 118.0822494517943966, -0.8002166990800740898 ) ) ;
#5017 = CARTESIAN_POINT ( 'NONE',  ( -57.53497731650991653, 2.247686704661286505, -1.882970859819768306 ) ) ;
#5018 = CARTESIAN_POINT ( 'NONE',  ( -4.852412226131026962, 117.4768382700202238, 0.9922438998348902528 ) ) ;
#5019 = CARTESIAN_POINT ( 'NONE',  ( 11.12287255170432232, 123.1247571232444784, 1.608126361149619044 ) ) ;
#5020 = DIRECTION ( 'NONE',  ( -0.9998004120163610509, -5.205824365704083805E-17, -0.01997839162482749689 ) ) ;
#5021 = VECTOR ( 'NONE', #11832, 1000.000000000000000 ) ;
#5022 = CARTESIAN_POINT ( 'NONE',  ( 0.8920107295035074602, 116.4394364983335493, -0.02072182073814201816 ) ) ;
#5023 = EDGE_CURVE ( 'NONE', #33803, #38620, #16421, .T. ) ;
#5024 = CARTESIAN_POINT ( 'NONE',  ( 8.391957350906555035, -2.082342975431243026, 0.7039615705134369961 ) ) ;
#5025 = CARTESIAN_POINT ( 'NONE',  ( 10.48728279712171663, 126.1106773019354819, 0.5683957799248651188 ) ) ;
#5026 = DIRECTION ( 'NONE',  ( 0.9998501190848640974, 0.01731298258485272981, 8.537024980200786319E-16 ) ) ;
#5027 = CIRCLE ( 'NONE', #20617, 0.2540000000000000036 ) ;
#5028 = CARTESIAN_POINT ( 'NONE',  ( -43.13073682054399427, 20.84535665847942454, -0.1327613832364097080 ) ) ;
#5029 = CARTESIAN_POINT ( 'NONE',  ( -2.601682421829722980, 117.9394517735116210, 1.236607248841048667 ) ) ;
#5030 = CARTESIAN_POINT ( 'NONE',  ( -7.931483696868459887, 121.8266375666164834, -1.035712634723692682 ) ) ;
#5031 = CARTESIAN_POINT ( 'NONE',  ( -57.95665747882670615, 0.5159457608236717174, 0.4254811051331099381 ) ) ;
#5032 = CARTESIAN_POINT ( 'NONE',  ( -51.27035844764527184, 15.91047978596967560, 4.316378984520650164 ) ) ;
#5033 = EDGE_CURVE ( 'NONE', #20535, #40413, #13020, .T. ) ;
#5034 = CARTESIAN_POINT ( 'NONE',  ( -2.769246990705085398, 116.5678055239024644, 0.05256187475617120353 ) ) ;
#5035 = ORIENTED_EDGE ( 'NONE', *, *, #13479, .T. ) ;
#5036 = CARTESIAN_POINT ( 'NONE',  ( -50.06424591225965059, 20.16147316606144813, -2.291703678227673180 ) ) ;
#5037 = CARTESIAN_POINT ( 'NONE',  ( -7.892965638028277553, 122.0249252363302332, -0.9262618160925026878 ) ) ;
#5038 = CARTESIAN_POINT ( 'NONE',  ( -8.026787933082857762, 121.5445110286360801, 0.8405406253987726117 ) ) ;
#5039 = AXIS2_PLACEMENT_3D ( 'NONE', #13503, #36306, #16259 ) ;
#5040 = ORIENTED_EDGE ( 'NONE', *, *, #3988, .F. ) ;
#5041 = CARTESIAN_POINT ( 'NONE',  ( 4.060319184079548727, 115.6909491485452435, -1.425993417255509987 ) ) ;
#5042 = CARTESIAN_POINT ( 'NONE',  ( -9.229262982541685645, 124.0999252189730697, -0.4162339757116149674 ) ) ;
#5043 = CARTESIAN_POINT ( 'NONE',  ( 4.908419482240064191, -12.74103600948764381, 2.406175225133469819 ) ) ;
#5044 = CARTESIAN_POINT ( 'NONE',  ( -2.090077592200571655, 117.5043770775735510, 0.5427014567576284865 ) ) ;
#5045 = DIRECTION ( 'NONE',  ( -4.017660918040594346E-17, 1.000000000000000000, 2.376309959284834438E-19 ) ) ;
#5046 = CARTESIAN_POINT ( 'NONE',  ( 17.17229002331729859, 122.7237354506536491, 0.5096938506424069093 ) ) ;
#5047 = CARTESIAN_POINT ( 'NONE',  ( -6.439798515484507670E-14, 156.3034662015457172, 9.575285601066443938E-17 ) ) ;
#5048 = DIRECTION ( 'NONE',  ( 5.188838149069472160E-16, -1.699382548006136559E-16, -1.000000000000000000 ) ) ;
#5049 = CARTESIAN_POINT ( 'NONE',  ( -0.5455758836206960893, 21.45819190514113117, -0.8097498057291211415 ) ) ;
#5050 = CARTESIAN_POINT ( 'NONE',  ( -23.21373371908098449, 149.6306211361744829, -0.4638656453230912136 ) ) ;
#5051 = CARTESIAN_POINT ( 'NONE',  ( -41.54364448253001285, 22.96340085312751356, -1.538956392779695648 ) ) ;
#5052 = VERTEX_POINT ( 'NONE', #37701 ) ;
#5053 = PLANE ( 'NONE',  #5060 ) ;
#5054 = VERTEX_POINT ( 'NONE', #28103 ) ;
#5055 = CARTESIAN_POINT ( 'NONE',  ( -8.380759076080833481, 119.8444141578249287, 1.108220873400043383 ) ) ;
#5056 = DIRECTION ( 'NONE',  ( 5.188838149069472160E-16, -1.699382548006136559E-16, -1.000000000000000000 ) ) ;
#5057 = CARTESIAN_POINT ( 'NONE',  ( 21.06903215802083906, 150.2702755442954583, 2.120733010085479986 ) ) ;
#5058 = CARTESIAN_POINT ( 'NONE',  ( -57.97024931889890809, 0.5691613924952432235, -0.8993266954183887218 ) ) ;
#5059 = CARTESIAN_POINT ( 'NONE',  ( 20.48420673234485534, 149.1468970683199586, -1.615293151967227558 ) ) ;
#5060 = AXIS2_PLACEMENT_3D ( 'NONE', #27814, #34426, #18212 ) ;
#5061 = CARTESIAN_POINT ( 'NONE',  ( 2.913282581332740762, -14.11548038430587937, -3.586046950971230274 ) ) ;
#5062 = CARTESIAN_POINT ( 'NONE',  ( -22.34249146463940860, 149.5981344557702641, -1.749037778780574204 ) ) ;
#5063 = CARTESIAN_POINT ( 'NONE',  ( 4.794168055694363773, 117.6364379244655680, -0.9473893282713367059 ) ) ;
#5064 = EDGE_CURVE ( 'NONE', #32592, #5970, #30425, .T. ) ;
#5065 = VERTEX_POINT ( 'NONE', #27895 ) ;
#5066 = CARTESIAN_POINT ( 'NONE',  ( -9.238523569214027731, 124.0999252189730697, 0.04720364951821285487 ) ) ;
#5067 = EDGE_CURVE ( 'NONE', #22768, #29525, #23905, .T. ) ;
#5068 = CARTESIAN_POINT ( 'NONE',  ( 6.397261194921658678, -14.09295207620744961, -0.07176229933514734205 ) ) ;
#5069 = CARTESIAN_POINT ( 'NONE',  ( -17.14500000000466784, 71.11999999999886768, 1.269999999999998241 ) ) ;
#5070 = AXIS2_PLACEMENT_3D ( 'NONE', #39164, #39596, #35340 ) ;
#5071 = EDGE_CURVE ( 'NONE', #24980, #17493, #4912, .T. ) ;
#5072 = CARTESIAN_POINT ( 'NONE',  ( 5.348924234570989533, 56.51499999999999346, 4.492130288940735738 ) ) ;
#5073 = VERTEX_POINT ( 'NONE', #24909 ) ;
#5074 = CARTESIAN_POINT ( 'NONE',  ( 5.016192601342504886, 119.3892302351119810, 1.087184205914811574 ) ) ;
#5075 = DIRECTION ( 'NONE',  ( 0.01731298258487879230, -0.9998501190848636533, -9.150538185806814706E-15 ) ) ;
#5076 = TOROIDAL_SURFACE ( 'NONE', #31569, 5.080000000000005400, 0.5080000000000000071 ) ;
#5077 = CARTESIAN_POINT ( 'NONE',  ( 5.078986093043054595, 72.48346620154573827, 0.1014902294541243782 ) ) ;
#5078 = CARTESIAN_POINT ( 'NONE',  ( -2.387353046264593548, 119.4803856251332945, 0.5366433100809054890 ) ) ;
#5079 = CARTESIAN_POINT ( 'NONE',  ( 0.8732425085435751022, -3.549726780817298977, -8.398906084147368389 ) ) ;
#5080 = CARTESIAN_POINT ( 'NONE',  ( 9.787166303541834367, 124.1138826855306831, 0.8907577946409742653 ) ) ;
#5081 = CARTESIAN_POINT ( 'NONE',  ( -4.726681166799090228, 118.5930653697794384, -1.020516978120344476 ) ) ;
#5082 = CARTESIAN_POINT ( 'NONE',  ( 2.881812722985360953, 116.8851979753409580, -0.3221759108904497793 ) ) ;
#5083 = DIRECTION ( 'NONE',  ( -0.4849315768086535083, -0.8745520943968250194, -1.030032898892974695E-16 ) ) ;
#5084 = CARTESIAN_POINT ( 'NONE',  ( -58.36135728304071080, -0.2738979606847323778, 0.1145308973088972754 ) ) ;
#5085 = CARTESIAN_POINT ( 'NONE',  ( -28.99046981630712949, 65.28995187595535299, -1.524000000000006017 ) ) ;
#5086 = CARTESIAN_POINT ( 'NONE',  ( -52.58202682230450620, 11.88959489689803561, 4.235729473019533842 ) ) ;
#5087 = CARTESIAN_POINT ( 'NONE',  ( 1.858891552337616826, -15.10179129218686711, 5.555419934288657657 ) ) ;
#5088 = CARTESIAN_POINT ( 'NONE',  ( -4.266030196957218301, 118.2243171346437407, 0.2924649446876417258 ) ) ;
#5089 = DIRECTION ( 'NONE',  ( -1.000000000000000000, -6.353134868986659519E-16, 0.000000000000000000 ) ) ;
#5090 = EDGE_LOOP ( 'NONE', ( #3682, #11368, #8634, #15558, #23099, #490, #37101, #24090, #37153, #22767, #31433 ) ) ;
#5091 = CARTESIAN_POINT ( 'NONE',  ( -49.72660956849071567, 16.83360665160238412, 5.072308565479690223 ) ) ;
#5092 = CARTESIAN_POINT ( 'NONE',  ( 4.269537782945402427, 119.3621508961521442, -0.7584028417339077066 ) ) ;
#5093 = DIRECTION ( 'NONE',  ( -5.188838149069471174E-16, 1.699382548006136313E-16, 1.000000000000000000 ) ) ;
#5094 = CARTESIAN_POINT ( 'NONE',  ( 4.291477964748057872, 118.2137869882025001, 0.5063463920358112214 ) ) ;
#5095 = CARTESIAN_POINT ( 'NONE',  ( -7.076231864619286327, 121.9239394581621809, -0.5528764260536546127 ) ) ;
#5096 = DIRECTION ( 'NONE',  ( 1.011795553208986377E-16, 1.000000000000000000, -0.000000000000000000 ) ) ;
#5097 = CARTESIAN_POINT ( 'NONE',  ( 14.91134437181069927, 120.3281135998953459, 0.2979641475761143354 ) ) ;
#5098 = VERTEX_POINT ( 'NONE', #31094 ) ;
#5099 = CARTESIAN_POINT ( 'NONE',  ( 4.496586626007489151, 27.28078351817337222, -1.068494511273165193 ) ) ;
#5100 = CARTESIAN_POINT ( 'NONE',  ( -11.65596162629437593, 126.1299551460304542, -1.384704262848757583 ) ) ;
#5101 = CARTESIAN_POINT ( 'NONE',  ( -38.65395868481546415, 29.38327706004843876, 1.269999999999994245 ) ) ;
#5102 = CARTESIAN_POINT ( 'NONE',  ( -47.60342124589670476, 19.66962190512531805, 5.193532021785222774 ) ) ;
#5103 = EDGE_CURVE ( 'NONE', #12049, #35679, #18297, .T. ) ;
#5104 = LINE ( 'NONE', #41505, #9955 ) ;
#5105 = CARTESIAN_POINT ( 'NONE',  ( 6.996049371394188476, 121.9530687059719583, 0.1976249421933106154 ) ) ;
#5106 = CARTESIAN_POINT ( 'NONE',  ( -4.024516124431025688, 26.91537645720152128, -2.298571904627217499 ) ) ;
#5107 = CARTESIAN_POINT ( 'NONE',  ( 20.68355264112275904, 132.2482564273973935, 1.400420337322433983 ) ) ;
#5108 = DIRECTION ( 'NONE',  ( -3.414809992080330305E-15, 0.000000000000000000, 1.000000000000000000 ) ) ;
#5110 = CARTESIAN_POINT ( 'NONE',  ( 13.60293432442217210, 121.5020190402118203, -1.066732574264078526 ) ) ;
#5109 = CARTESIAN_POINT ( 'NONE',  ( 3.213008622916347701, -14.43860267280072662, 2.307402664594705222 ) ) ;
#5111 = CARTESIAN_POINT ( 'NONE',  ( -16.36721571005508835, 151.0861551944122141, 1.708847769304776110 ) ) ;
#5112 = CARTESIAN_POINT ( 'NONE',  ( -1.535301415185580609, 19.99377045568717293, 4.360315235486975638 ) ) ;
#5113 = CARTESIAN_POINT ( 'NONE',  ( -3.210256534570933962, 159.4348965051207756, -0.5208765431038285820 ) ) ;
#5114 = CARTESIAN_POINT ( 'NONE',  ( 0.2465545558977290663, 24.09562519341298170, -0.9435640554424079562 ) ) ;
#5115 = ORIENTED_EDGE ( 'NONE', *, *, #7621, .F. ) ;
#5116 = CARTESIAN_POINT ( 'NONE',  ( -51.60883138897295908, 11.95321700621929040, 1.992363451474690628 ) ) ;
#5117 = B_SPLINE_CURVE_WITH_KNOTS ( 'NONE', 3,
 ( #19722, #380, #35729, #32741, #26129, #35515, #6133, #22907, #10147, #28900, #29324, #6540, #6336, #29108, #39131, #41915, #32105, #9937, #12715, #35941, #25705, #3574, #16535, #6970, #22487, #29545, #41703, #19306, #13346, #26335, #36153, #19941, #12511, #10776, #13562 ),
 .UNSPECIFIED., .F., .F.,
 ( 4, 1, 1, 1, 1, 1, 1, 1, 1, 1, 1, 1, 1, 1, 1, 1, 1, 1, 1, 1, 1, 1, 1, 1, 1, 1, 1, 1, 1, 1, 1, 1, 4 ),
 ( 0.000000000000000000, 0.02711375962671787321, 0.05385523109991235263, 0.08027126036152537614, 0.1064096946071439176, 0.1323192412471900226, 0.1580495177521483718, 0.1882118685537063907, 0.2182788543618764954, 0.2483346178351386324, 0.2784631806910429774, 0.3054937156393619513, 0.3327069032348308197, 0.3601597580799023035, 0.3879077415152338837, 0.4160045136367338525, 0.4445017332217630623, 0.4734489055539064517, 0.5028932750457014711, 0.5328797594123376724, 0.5634509204570880003, 0.5946469669818265080, 0.6265057848166851739, 0.6590629893014032792, 0.6923519956652609553, 0.7264041031822485728, 0.7612485893105871426, 0.7986318966073006065, 0.8369441774603861850, 0.8762126957585177900, 0.9164627945539034481, 0.9577180065289634392, 1.000000000000000000 ),
 .UNSPECIFIED. ) ;
#5118 = CARTESIAN_POINT ( 'NONE',  ( -0.6165924928998587351, 120.7136710450757988, 0.2143668442300581123 ) ) ;
#5119 = CARTESIAN_POINT ( 'NONE',  ( 2.450443274655972559, -15.26395620497007855, 5.889056594049635329 ) ) ;
#5120 = CARTESIAN_POINT ( 'NONE',  ( 7.262759831279620215, 121.2980461901665308, -0.7361999724971874937 ) ) ;
#5121 = ORIENTED_EDGE ( 'NONE', *, *, #37079, .T. ) ;
#5122 = CARTESIAN_POINT ( 'NONE',  ( 1.405512873546346686, 115.7027606773773130, 1.735607224157626360 ) ) ;
#5123 = EDGE_CURVE ( 'NONE', #24344, #9964, #20759, .T. ) ;
#5124 = ORIENTED_EDGE ( 'NONE', *, *, #19889, .T. ) ;
#5125 = CARTESIAN_POINT ( 'NONE',  ( 3.089232434235547942, -13.39873834325867819, 1.372807258641574935 ) ) ;
#5126 = CARTESIAN_POINT ( 'NONE',  ( -4.784569842647550253, 117.8429238250669329, -0.9400432804894900407 ) ) ;
#5127 = CARTESIAN_POINT ( 'NONE',  ( 8.054407255016364786, 122.8529229587361442, 0.1293742239074502920 ) ) ;
#5128 = ADVANCED_FACE ( 'NONE', ( #38338 ), #17788, .T. ) ;
#5129 = ORIENTED_EDGE ( 'NONE', *, *, #13651, .T. ) ;
#5130 = CARTESIAN_POINT ( 'NONE',  ( 5.840405771877526853, 118.8996324090661147, 1.179527747254400349 ) ) ;
#5131 = CARTESIAN_POINT ( 'NONE',  ( -3.682264917456322895, 65.62546620154573418, -0.07358041635423968885 ) ) ;
#5132 = DIRECTION ( 'NONE',  ( 4.017660918040594346E-17, -1.000000000000000000, -2.376309959284834438E-19 ) ) ;
#5133 = CARTESIAN_POINT ( 'NONE',  ( 0.03067001211929198945, 158.6015251912307633, -1.534852821454057770 ) ) ;
#5134 = CARTESIAN_POINT ( 'NONE',  ( 6.912985389844387818, 117.2044255678715814, -0.04371034868568298565 ) ) ;
#5135 = CARTESIAN_POINT ( 'NONE',  ( 6.059261036834394432, 71.63300248836199557, -5.016499999999999737 ) ) ;
#5136 = CARTESIAN_POINT ( 'NONE',  ( 1.939574901179839994, -15.09955500034904041, 5.855824770328826645 ) ) ;
#5137 = CARTESIAN_POINT ( 'NONE',  ( -41.97746338594183868, 23.60773098774231826, 1.523999999999994026 ) ) ;
#5138 = CARTESIAN_POINT ( 'NONE',  ( 8.947566919452587848E-16, 9.293884745518887769, 0.000000000000000000 ) ) ;
#5139 = CARTESIAN_POINT ( 'NONE',  ( -4.713257660251447767, 117.8947922744557815, 0.7957716318157286306 ) ) ;
#5140 = ORIENTED_EDGE ( 'NONE', *, *, #34929, .F. ) ;
#5141 = ORIENTED_EDGE ( 'NONE', *, *, #25593, .T. ) ;
#5142 = CARTESIAN_POINT ( 'NONE',  ( -4.908310932783608749, 117.4079579380719736, 0.9676122992747743234 ) ) ;
#5143 = CARTESIAN_POINT ( 'NONE',  ( 8.499044578041351272, 119.2581920680855774, -1.011821766694761981 ) ) ;
#5144 = CARTESIAN_POINT ( 'NONE',  ( -4.571503503190820439, 114.7252160460498516, -1.874454982749236276 ) ) ;
#5145 = CARTESIAN_POINT ( 'NONE',  ( 4.862967985527940407, 117.6413485483879953, 1.052801483323805298 ) ) ;
#5146 = CARTESIAN_POINT ( 'NONE',  ( -6.517733866319332394E-14, 78.32546620154573702, 2.848871684924056535E-29 ) ) ;
#5147 = CARTESIAN_POINT ( 'NONE',  ( -0.7689147969093301782, 119.5055576915191580, 0.7020325503247997201 ) ) ;
#5148 = CARTESIAN_POINT ( 'NONE',  ( 4.900892916173488878, 117.4105777512120596, -0.9669312268769758578 ) ) ;
#5149 = FACE_OUTER_BOUND ( 'NONE', #4624, .T. ) ;
#5150 = CARTESIAN_POINT ( 'NONE',  ( 3.456814872816273088, -13.76118077623555891, 3.223863823609153023 ) ) ;
#5151 = CARTESIAN_POINT ( 'NONE',  ( 2.817215192600937446, 108.0685014782224442, -4.280041469292686251 ) ) ;
#5152 = CARTESIAN_POINT ( 'NONE',  ( -4.381111989981776311, 28.12932232230255281, 1.300020847918438527 ) ) ;
#5153 = CIRCLE ( 'NONE', #28924, 5.588000000000006295 ) ;
#5154 = CARTESIAN_POINT ( 'NONE',  ( -0.6390711918370651778, 115.7029491485453292, 1.736656509918723668 ) ) ;
#5155 = CARTESIAN_POINT ( 'NONE',  ( -4.247245584637960647, 22.75789413176893206, 1.861891798430825862 ) ) ;
#5156 = ORIENTED_EDGE ( 'NONE', *, *, #18565, .T. ) ;
#5157 = CARTESIAN_POINT ( 'NONE',  ( -3.490548159187448096, 104.6144662015455253, -3.347245557147066286 ) ) ;
#5158 = CARTESIAN_POINT ( 'NONE',  ( 4.167245103190982292, -15.48560191675932352, 1.819225864046467356 ) ) ;
#5159 = CARTESIAN_POINT ( 'NONE',  ( -19.82182223277795075, 148.2167131080949787, 1.724547319354139630 ) ) ;
#5160 = CARTESIAN_POINT ( 'NONE',  ( -0.9201843903949125103, 16.76996313919548598, -0.3265437062991076722 ) ) ;
#5161 = CARTESIAN_POINT ( 'NONE',  ( -0.09387087892865565719, 20.69761720779959902, -0.9769954323643923466 ) ) ;
#5162 = ORIENTED_EDGE ( 'NONE', *, *, #35780, .T. ) ;
#5163 = ORIENTED_EDGE ( 'NONE', *, *, #4297, .F. ) ;
#5164 = DIRECTION ( 'NONE',  ( -0.9998004120163608288, 0.000000000000000000, -0.01997839162482749342 ) ) ;
#5165 = CARTESIAN_POINT ( 'NONE',  ( 2.231675704589601850, 117.6064948828932444, 1.117935386608752024 ) ) ;
#5166 = CARTESIAN_POINT ( 'NONE',  ( -7.857169925943728650, 121.9903164032602518, 0.5981771023335126225 ) ) ;
#5167 = LINE ( 'NONE', #5586, #15722 ) ;
#5168 = ADVANCED_FACE ( 'NONE', ( #37909 ), #1935, .F. ) ;
#5169 = CARTESIAN_POINT ( 'NONE',  ( 4.535580177108445632, 118.0878415417625433, -0.6032448829988410477 ) ) ;
#5170 = CARTESIAN_POINT ( 'NONE',  ( 18.18950303832456328, 147.2296321676236062, -1.619102437044615206 ) ) ;
#5171 = CARTESIAN_POINT ( 'NONE',  ( -20.02396230387753917, 148.3334041379468715, -2.502640320863741330 ) ) ;
#5172 = CARTESIAN_POINT ( 'NONE',  ( 4.801216665947148243, 117.4032681888235459, -1.015537427445656782 ) ) ;
#5173 = EDGE_CURVE ( 'NONE', #117, #4432, #38222, .T. ) ;
#5174 = CARTESIAN_POINT ( 'NONE',  ( -6.398136396394987102, 30.40553754182522539, 1.409394703459281084 ) ) ;
#5175 = CARTESIAN_POINT ( 'NONE',  ( 0.006534791579796636780, 156.3267223255430167, -0.3270276925529294054 ) ) ;
#5176 = ORIENTED_EDGE ( 'NONE', *, *, #34877, .F. ) ;
#5177 = CARTESIAN_POINT ( 'NONE',  ( 3.221942100833175893, -14.53498920702628361, 2.661941298785070575 ) ) ;
#5178 =( BOUNDED_CURVE ( )  B_SPLINE_CURVE ( 3, ( #31995, #22797, #12409, #28591 ),
 .UNSPECIFIED., .F., .T. ) 
 B_SPLINE_CURVE_WITH_KNOTS ( ( 4, 4 ),
 ( 0.5001855759278981406, 0.7498838476046071344 ),
 .UNSPECIFIED. ) 
 CURVE ( )  GEOMETRIC_REPRESENTATION_ITEM ( )  RATIONAL_B_SPLINE_CURVE ( ( 1.000000000000000000, 0.6670689721821350116, 0.5004025482900600341, 0.5000007283237750677 ) ) 
 REPRESENTATION_ITEM ( '' )  );
#5179 = CARTESIAN_POINT ( 'NONE',  ( 10.62867326514809463, 56.48194529650093187, -4.405924061720181584 ) ) ;
#5180 = CARTESIAN_POINT ( 'NONE',  ( -58.58343337229857184, -0.6799398409029571155, 0.1767901212645599796 ) ) ;
#5181 = CIRCLE ( 'NONE', #3134, 0.5080000000000002292 ) ;
#5182 = CARTESIAN_POINT ( 'NONE',  ( -2.587970193024280441, -12.16632112844677494, -3.833404006186521773 ) ) ;
#5183 = CARTESIAN_POINT ( 'NONE',  ( 15.47075146591460104, 139.6011575924185877, 1.761802977227842737 ) ) ;
#5184 = FACE_OUTER_BOUND ( 'NONE', #21824, .T. ) ;
#5185 = CARTESIAN_POINT ( 'NONE',  ( -2.433495328593940243, 107.4436264546101967, 4.557236999380250175 ) ) ;
#5186 = CARTESIAN_POINT ( 'NONE',  ( 2.267534764145236803, 6.115564135048844108, 4.037922524061999141 ) ) ;
#5187 = CARTESIAN_POINT ( 'NONE',  ( 8.770618086120967050, 123.6813396614493712, 0.1752578222716852652 ) ) ;
#5188 = CARTESIAN_POINT ( 'NONE',  ( 8.137580693842743074, 4.222088520697473868, -2.276242723817686997 ) ) ;
#5189 = CARTESIAN_POINT ( 'NONE',  ( -57.37715403173692152, 1.618736692213004869, -0.5106765013061207448 ) ) ;
#5190 = CARTESIAN_POINT ( 'NONE',  ( -2.146602167848374432, 116.4048268131027868, -0.3314024647271391899 ) ) ;
#5191 = DIRECTION ( 'NONE',  ( 5.188838149069472160E-16, -1.699382548006136559E-16, -1.000000000000000000 ) ) ;
#5192 = CARTESIAN_POINT ( 'NONE',  ( -12.21488373879589240, 17.14499999999999957, 4.381499999999999950 ) ) ;
#5193 = LINE ( 'NONE', #8580, #29733 ) ;
#5194 = CARTESIAN_POINT ( 'NONE',  ( -5.224212249200172131, -8.128124378088662283, -6.605211778952579493 ) ) ;
#5195 = CARTESIAN_POINT ( 'NONE',  ( 3.904803215525951554, 118.1588881757245986, 0.7354103002220402363 ) ) ;
#5196 = DIRECTION ( 'NONE',  ( -1.000000000000000000, 1.288607544181256449E-16, 0.000000000000000000 ) ) ;
#5197 = CARTESIAN_POINT ( 'NONE',  ( -58.82991074935231524, -0.2577531494038359794, -1.058401375502683064E-14 ) ) ;
#5198 = CARTESIAN_POINT ( 'NONE',  ( 0.3199181899538769414, 107.4969721965504021, -4.676354563382915330 ) ) ;
#5199 = CARTESIAN_POINT ( 'NONE',  ( -16.72896750809251998, 155.2649736186859570, 0.2017331744915137337 ) ) ;
#5200 = VERTEX_POINT ( 'NONE', #15315 ) ;
#5201 = CARTESIAN_POINT ( 'NONE',  ( -58.21785149106106871, 1.559091779220117546, -0.3785645914143067059 ) ) ;
#5202 = ORIENTED_EDGE ( 'NONE', *, *, #35747, .F. ) ;
#5203 = CARTESIAN_POINT ( 'NONE',  ( -46.34235131104743743, 20.67093754025578534, -4.736928721793741914 ) ) ;
#5204 = CARTESIAN_POINT ( 'NONE',  ( -2.884051542275779756, 156.0957788938021054, -0.05763021347587621995 ) ) ;
#5205 = CARTESIAN_POINT ( 'NONE',  ( 5.510877305967752271, -15.11690630435501248, 2.581843384194929758 ) ) ;
#5206 = CARTESIAN_POINT ( 'NONE',  ( -13.31748376333910322, 121.6721647909590303, 1.150164054616430676 ) ) ;
#5207 = CARTESIAN_POINT ( 'NONE',  ( 21.76596270643820219, 150.3096123636779566, -1.000581967439477138 ) ) ;
#5208 = CARTESIAN_POINT ( 'NONE',  ( -3.789191232057584902, 13.46218022696137773, 2.646434746401360893 ) ) ;
#5209 = CARTESIAN_POINT ( 'NONE',  ( -23.32660363739045906, 146.7646281656787437, -0.9249455126139313199 ) ) ;
#5210 = CARTESIAN_POINT ( 'NONE',  ( -49.91180784202388310, 16.43617519331882804, -4.943574328148589991 ) ) ;
#5211 = ORIENTED_EDGE ( 'NONE', *, *, #2760, .T. ) ;
#5212 = AXIS2_PLACEMENT_3D ( 'NONE', #11950, #28562, #34546 ) ;
#5213 = CARTESIAN_POINT ( 'NONE',  ( -2.183349241107786387, 116.1870506606769311, -0.03693642060881925648 ) ) ;
#5214 = DIRECTION ( 'NONE',  ( -0.8745520943968240202, 0.4849315768086553402, -5.361993529360572958E-16 ) ) ;
#5215 = CARTESIAN_POINT ( 'NONE',  ( -10.94646760555361276, 123.1276765127550021, 1.119819633367153289 ) ) ;
#5216 = CARTESIAN_POINT ( 'NONE',  ( -56.64449391386203558, 3.408586874113735288, -2.059255000246300149 ) ) ;
#5217 = CARTESIAN_POINT ( 'NONE',  ( 4.191956958763752183, 119.0775769483117870, -0.8365378509937176910 ) ) ;
#5218 = CARTESIAN_POINT ( 'NONE',  ( -13.51395941584921268, 155.6725583577350278, -2.021746995258101975 ) ) ;
#5219 = CARTESIAN_POINT ( 'NONE',  ( -54.98111839650035648, 8.542840639972862249, -3.427624633821342304 ) ) ;
#5220 = EDGE_CURVE ( 'NONE', #12023, #39424, #37016, .T. ) ;
#5221 = CARTESIAN_POINT ( 'NONE',  ( 3.160209531530921545, 156.1781389015385457, -0.7303267873898456886 ) ) ;
#5222 = VERTEX_POINT ( 'NONE', #25124 ) ;
#5223 = CARTESIAN_POINT ( 'NONE',  ( -5.349253755625555939, 156.5090806470891209, -1.752114854137454492 ) ) ;
#5224 = CARTESIAN_POINT ( 'NONE',  ( 3.048550003781630213, -15.65190959513015834, 4.520219006486421165 ) ) ;
#5225 = CARTESIAN_POINT ( 'NONE',  ( -4.452087279397210828, 118.1112359772488105, -0.7572249732135748479 ) ) ;
#5226 = CARTESIAN_POINT ( 'NONE',  ( -57.85534701229748578, 0.8496279762696679061, -1.203237356453227047 ) ) ;
#5227 = CARTESIAN_POINT ( 'NONE',  ( -4.890164892654324191, 117.4101971730238461, 0.9753743779596022456 ) ) ;
#5228 = CARTESIAN_POINT ( 'NONE',  ( 12.25802010074268722, 153.5964916033214820, 2.078998712700113938 ) ) ;
#5229 = CARTESIAN_POINT ( 'NONE',  ( 5.332935397695207413, 50.63946620154572997, 0.1065647409268298818 ) ) ;
#5230 = CARTESIAN_POINT ( 'NONE',  ( -8.364652471777612064, 2.666895906452835252, -0.9765287277423425616 ) ) ;
#5231 = CARTESIAN_POINT ( 'NONE',  ( 15.79012389680288564, 146.9282941555416073, 0.7681517710631365903 ) ) ;
#5232 = DIRECTION ( 'NONE',  ( 0.9998501190848629872, 0.01731298258490743258, 8.537024980200819846E-16 ) ) ;
#5233 = TOROIDAL_SURFACE ( 'NONE', #3184, 6.985000000000000320, 0.6350000000000000089 ) ;
#5235 = ORIENTED_EDGE ( 'NONE', *, *, #26947, .T. ) ;
#5234 = DIRECTION ( 'NONE',  ( -1.000000000000000000, 0.000000000000000000, 0.000000000000000000 ) ) ;
#5236 = CARTESIAN_POINT ( 'NONE',  ( -1.144332903081027197, 117.3993836041148597, 1.432019610544279509 ) ) ;
#5237 = DIRECTION ( 'NONE',  ( 5.188838149069472160E-16, -1.699382548006136559E-16, -1.000000000000000000 ) ) ;
#5238 = CARTESIAN_POINT ( 'NONE',  ( -57.60038635073814817, 1.097546858218806376, -1.001372043670648409E-14 ) ) ;
#5239 = CARTESIAN_POINT ( 'NONE',  ( -48.81380759447691275, 19.38479668107215304, 4.754960688114458378 ) ) ;
#5240 = CARTESIAN_POINT ( 'NONE',  ( -23.33610279681233379, 149.0590277239482475, -0.3121099645145853363 ) ) ;
#5241 = VERTEX_POINT ( 'NONE', #23158 ) ;
#5242 = CARTESIAN_POINT ( 'NONE',  ( -47.36975192132249646, 22.26287704218617236, -3.814390537888114441 ) ) ;
#5243 = CARTESIAN_POINT ( 'NONE',  ( -6.895199152412361698, 121.8168396766305079, -0.5159271962741722728 ) ) ;
#5244 = CARTESIAN_POINT ( 'NONE',  ( -23.91048590848665967, 81.84235438443283783, 1.269999999999993801 ) ) ;
#5245 = ORIENTED_EDGE ( 'NONE', *, *, #12340, .T. ) ;
#5246 = CARTESIAN_POINT ( 'NONE',  ( 0.2391656075941314130, 115.7030485030756637, -1.756104538880229438 ) ) ;
#5247 = CARTESIAN_POINT ( 'NONE',  ( -4.547323659248203143, 121.1438296405421937, -0.2486498796252667176 ) ) ;
#5248 = CARTESIAN_POINT ( 'NONE',  ( 4.521557965551993519, -14.38033123432501448, 4.565926699156682922 ) ) ;
#5249 = CARTESIAN_POINT ( 'NONE',  ( -15.47853073355919840, 123.0316835747794642, 0.9738675477772638089 ) ) ;
#5250 = AXIS2_PLACEMENT_3D ( 'NONE', #29878, #716, #26681 ) ;
#5251 = CARTESIAN_POINT ( 'NONE',  ( 4.016744494447205049, 117.3993836135117732, -1.174929138160409448 ) ) ;
#5252 = CARTESIAN_POINT ( 'NONE',  ( 23.34743456777619386, 142.7586093370927074, 0.6964168797349272744 ) ) ;
#5253 = CARTESIAN_POINT ( 'NONE',  ( 6.506917054590420690, 121.7798191776175685, 0.1679176037484078621 ) ) ;
#5254 = CARTESIAN_POINT ( 'NONE',  ( -4.977848145772336252, 117.5941869881971655, 0.7723625501233751800 ) ) ;
#5255 = CARTESIAN_POINT ( 'NONE',  ( -0.09387087892865565719, 20.69761720779959902, -0.9769954323643923466 ) ) ;
#5256 = CARTESIAN_POINT ( 'NONE',  ( -5.779653879267294236, 116.9360814311326777, -0.1581498910197087771 ) ) ;
#5257 = CARTESIAN_POINT ( 'NONE',  ( -44.94860098973432372, 21.36157941369687308, -3.600951499729750704 ) ) ;
#5258 = EDGE_CURVE ( 'NONE', #41397, #9260, #16575, .T. ) ;
#5259 = CARTESIAN_POINT ( 'NONE',  ( 1.589478822742971486E-15, 16.51000000000000156, 0.000000000000000000 ) ) ;
#5260 = ORIENTED_EDGE ( 'NONE', *, *, #10766, .T. ) ;
#5261 = CARTESIAN_POINT ( 'NONE',  ( 3.533749852891390208, 117.8629878115362715, 0.8862737175697782410 ) ) ;
#5262 = CARTESIAN_POINT ( 'NONE',  ( -35.99603394726484851, 64.04701136959550922, 1.523999999999990029 ) ) ;
#5263 = CARTESIAN_POINT ( 'NONE',  ( 9.950292893259801374, 157.6892375622926181, 1.550998551202242615 ) ) ;
#5264 = CARTESIAN_POINT ( 'NONE',  ( -58.21232023750493312, 0.08677210334285366533, -0.8315773506267210013 ) ) ;
#5265 = CIRCLE ( 'NONE', #24969, 0.5080000000000002292 ) ;
#5266 = CARTESIAN_POINT ( 'NONE',  ( 18.00466200016590435, 151.7072807693909340, -1.676127293294198628 ) ) ;
#5267 = CARTESIAN_POINT ( 'NONE',  ( -7.601118931484537100, 27.11072341857771306, -3.643763446188946542 ) ) ;
#5268 = CARTESIAN_POINT ( 'NONE',  ( -22.03343284943311176, 146.2042277794223537, -2.039575571141828192 ) ) ;
#5269 = CARTESIAN_POINT ( 'NONE',  ( 4.810014216029472323, 117.7355684663886137, -0.8789097560846608204 ) ) ;
#5270 = EDGE_CURVE ( 'NONE', #4943, #14176, #28686, .T. ) ;
#5271 = CARTESIAN_POINT ( 'NONE',  ( 1.375939976466430181, 106.2431249238853894, 5.170880015306797084 ) ) ;
#5272 = ORIENTED_EDGE ( 'NONE', *, *, #18338, .T. ) ;
#5273 = AXIS2_PLACEMENT_3D ( 'NONE', #12456, #39074, #6483 ) ;
#5274 = CARTESIAN_POINT ( 'NONE',  ( -13.61628268276122178, 150.2179846313823930, -0.04905232040057764392 ) ) ;
#5275 = CARTESIAN_POINT ( 'NONE',  ( -19.45004534592214185, 148.0998626603252148, -2.515250464377976947 ) ) ;
#5276 = CARTESIAN_POINT ( 'NONE',  ( 6.296695397805594396, -14.23921929796089003, 0.5540845800015932188 ) ) ;
#5277 = CARTESIAN_POINT ( 'NONE',  ( -3.361735136380934019, 117.3993835122084590, -1.373601552275676596 ) ) ;
#5278 = EDGE_CURVE ( 'NONE', #19512, #3855, #16360, .T. ) ;
#5279 = ORIENTED_EDGE ( 'NONE', *, *, #7178, .F. ) ;
#5280 = CARTESIAN_POINT ( 'NONE',  ( 8.582646176847930519, 120.3810071108087243, 1.481269161951472624 ) ) ;
#5281 = CARTESIAN_POINT ( 'NONE',  ( -3.174366308152013261, 91.02546620154572565, -0.06343139340882732180 ) ) ;
#5282 = CARTESIAN_POINT ( 'NONE',  ( -5.341065829615910587, 115.6909491485453003, 0.1995911688841381648 ) ) ;
#5283 = TOROIDAL_SURFACE ( 'NONE', #29068, 5.080000000000005400, 0.5080000000000000071 ) ;
#5284 = CARTESIAN_POINT ( 'NONE',  ( -2.312669815851230659, 124.5312663981120380, -0.02133033151766248331 ) ) ;
#5285 = CARTESIAN_POINT ( 'NONE',  ( -7.766292583485225443, -1.596223907437250844, -3.263082884517814364 ) ) ;
#5286 = CARTESIAN_POINT ( 'NONE',  ( 3.609032566395310671, 120.7384399880717467, 0.4518473439704071004 ) ) ;
#5287 = DIRECTION ( 'NONE',  ( -4.017660918040594346E-17, 1.000000000000000000, 2.376309959284834438E-19 ) ) ;
#5288 = CARTESIAN_POINT ( 'NONE',  ( 5.848384816632722583, 117.2350771734024164, -0.3616545339607747933 ) ) ;
#5289 = EDGE_CURVE ( 'NONE', #8441, #23676, #21186, .T. ) ;
#5290 = DIRECTION ( 'NONE',  ( -0.9891443546370349837, 0.000000000000000000, 0.1469470846586743706 ) ) ;
#5291 = CARTESIAN_POINT ( 'NONE',  ( -58.36255351679519521, -0.2764007135021583905, 0.1060264582682535484 ) ) ;
#5292 = EDGE_CURVE ( 'NONE', #41065, #30610, #19972, .T. ) ;
#5293 = CARTESIAN_POINT ( 'NONE',  ( 1.826496821415122707, -15.21410320048187970, 5.439012564009858330 ) ) ;
#5294 = CARTESIAN_POINT ( 'NONE',  ( -4.166291299642304047, 118.2394655740918097, 0.2241564256093856733 ) ) ;
#5295 = CARTESIAN_POINT ( 'NONE',  ( -24.32950799593924884, 77.42192949967211746, -1.270000000000005569 ) ) ;
#5296 = AXIS2_PLACEMENT_3D ( 'NONE', #1105, #26226, #20667 ) ;
#5297 = ORIENTED_EDGE ( 'NONE', *, *, #23821, .T. ) ;
#5298 = CARTESIAN_POINT ( 'NONE',  ( -47.65206802627297833, 20.46304711373551299, 5.210715034831059356 ) ) ;
#5299 = CARTESIAN_POINT ( 'NONE',  ( 4.179037867723048194, 119.2769959767378651, -0.7610518346563297509 ) ) ;
#5300 = CARTESIAN_POINT ( 'NONE',  ( -4.705839724742440389, 116.0444662015457595, 3.565396701626624143 ) ) ;
#5301 = CARTESIAN_POINT ( 'NONE',  ( 4.237069621333032110, 118.2250994327943943, 0.4770513927000196164 ) ) ;
#5302 = CARTESIAN_POINT ( 'NONE',  ( -15.52857178871880883, 148.0963874134046705, -1.155438959258076936 ) ) ;
#5303 = CARTESIAN_POINT ( 'NONE',  ( -5.369399562154598904, 64.90898011766716991, 1.270000000000005569 ) ) ;
#5304 = CARTESIAN_POINT ( 'NONE',  ( 3.703049682113265018, 116.6240124373522065, 0.07399574541707873432 ) ) ;
#5305 = ADVANCED_FACE ( 'NONE', ( #19549, #3180 ), #38542, .F. ) ;
#5306 = ORIENTED_EDGE ( 'NONE', *, *, #30088, .F. ) ;
#5307 = CARTESIAN_POINT ( 'NONE',  ( 2.889066315880882030, 25.55657059589919911, 3.609430016826872478 ) ) ;
#5308 = CARTESIAN_POINT ( 'NONE',  ( -30.83281893200567936, 55.49295607027229238, 1.269999999999994467 ) ) ;
#5309 = CARTESIAN_POINT ( 'NONE',  ( 7.019433301159567762, 78.79326733250422876, -2.552382320839209573 ) ) ;
#5310 = CARTESIAN_POINT ( 'NONE',  ( -47.98391741143318256, 19.46693557046443246, 5.364172754690429201 ) ) ;
#5311 = CARTESIAN_POINT ( 'NONE',  ( 6.079341768894599873, 121.3741006014788724, 0.4360735354898734317 ) ) ;
#5312 = CARTESIAN_POINT ( 'NONE',  ( 2.838909340336904563, 21.51804255560577772, 3.663749385350952181 ) ) ;
#5313 = CARTESIAN_POINT ( 'NONE',  ( 15.38106892591210872, 121.3506620944898060, 1.079669858139658434 ) ) ;
#5314 = CARTESIAN_POINT ( 'NONE',  ( 3.570581317670051380, 104.6144662015457243, -3.261568590886288810 ) ) ;
#5316 = CARTESIAN_POINT ( 'NONE',  ( 3.087569247026485275, 117.8293475852256904, -0.6612947004247918814 ) ) ;
#5315 = CARTESIAN_POINT ( 'NONE',  ( 2.971193505762239617, -14.05637172046637851, 0.8995351626913862253 ) ) ;
#5317 = CARTESIAN_POINT ( 'NONE',  ( -1.363824289596636374, 119.4570717772418220, 0.5813626927913073672 ) ) ;
#5318 = CARTESIAN_POINT ( 'NONE',  ( -2.394960105286914942, 16.54535949628658997, -3.951836011466995036 ) ) ;
#5319 = CARTESIAN_POINT ( 'NONE',  ( -1.907136510351378655, 116.7789519286944966, -0.3469662120689607776 ) ) ;
#5320 = CARTESIAN_POINT ( 'NONE',  ( -0.6881565663083963891, 18.49284505249605459, 0.6899137464212180548 ) ) ;
#5321 = ORIENTED_EDGE ( 'NONE', *, *, #29282, .F. ) ;
#5322 = CARTESIAN_POINT ( 'NONE',  ( -57.43023524350843445, 1.739013888464230329, 1.477089945056089704 ) ) ;
#5323 = CARTESIAN_POINT ( 'NONE',  ( -3.061305989504190972, 156.1243923452879017, 0.5262318146843659727 ) ) ;
#5324 = CARTESIAN_POINT ( 'NONE',  ( 5.272318886577700425, -12.73938755324596706, 2.198237985477529577 ) ) ;
#5325 = CARTESIAN_POINT ( 'NONE',  ( 0.5597765207467094717, 119.9180165495073283, -0.4599786748625143695 ) ) ;
#5326 = VERTEX_POINT ( 'NONE', #3612 ) ;
#5327 = CARTESIAN_POINT ( 'NONE',  ( 0.9215934890950072678, 115.7029463657684829, 1.750466622602536493 ) ) ;
#5328 = CARTESIAN_POINT ( 'NONE',  ( -4.777110523374184403, 117.8777403950456062, -0.8659071637066898530 ) ) ;
#5329 = CARTESIAN_POINT ( 'NONE',  ( 0.0005023639977465172704, 120.9974662015457056, -0.02514034870427557522 ) ) ;
#5330 = ORIENTED_EDGE ( 'NONE', *, *, #40453, .T. ) ;
#5331 = CARTESIAN_POINT ( 'NONE',  ( 16.68944084648531501, 128.5636217276695561, 2.149857652400631203 ) ) ;
#5332 = CARTESIAN_POINT ( 'NONE',  ( -5.664977208693890098, 57.14999999999999147, 5.033228321271210781 ) ) ;
#5333 = CARTESIAN_POINT ( 'NONE',  ( -30.45812239790965492, 71.16801738242446618, 1.269999999999990470 ) ) ;
#5334 = CARTESIAN_POINT ( 'NONE',  ( 0.03212616895145502249, 157.6269964811067155, -1.607724863813388971 ) ) ;
#5335 = EDGE_CURVE ( 'NONE', #37322, #28854, #3004, .T. ) ;
#5336 = CARTESIAN_POINT ( 'NONE',  ( 23.25176476241877310, 142.6711341654318801, 0.007203867522444172208 ) ) ;
#5337 = CARTESIAN_POINT ( 'NONE',  ( -3.909619041219702495, 60.89059347946586342, -1.269999999999992024 ) ) ;
#5338 = AXIS2_PLACEMENT_3D ( 'NONE', #12582, #16609, #25571 ) ;
#5339 = CARTESIAN_POINT ( 'NONE',  ( 1.868973561629162061, -15.15741002263305859, 5.907646661756425388 ) ) ;
#5340 = CARTESIAN_POINT ( 'NONE',  ( -5.332935397695334423, 51.14746620154573264, -0.1065647409268298818 ) ) ;
#5341 = CARTESIAN_POINT ( 'NONE',  ( -18.35410564743290607, 77.35382415001784295, 1.904999999999988480 ) ) ;
#5342 = CARTESIAN_POINT ( 'NONE',  ( -4.646523143152131219, 117.9818477556987943, 0.7218086234193739070 ) ) ;
#5343 = ORIENTED_EDGE ( 'NONE', *, *, #10441, .T. ) ;
#5344 = VERTEX_POINT ( 'NONE', #32559 ) ;
#5345 = CARTESIAN_POINT ( 'NONE',  ( -0.2209998912935267623, 118.7629491485454025, 1.272056456734703245 ) ) ;
#5346 = ADVANCED_FACE ( 'NONE', ( #19598 ), #32353, .T. ) ;
#5347 = CARTESIAN_POINT ( 'NONE',  ( -5.811960698193874286, 118.8837068780349142, -1.247592088532381460 ) ) ;
#5348 = CARTESIAN_POINT ( 'NONE',  ( -6.804471202056847190, 123.7298400107579255, -0.1732695889264300182 ) ) ;
#5349 = CARTESIAN_POINT ( 'NONE',  ( 4.730984371466873561, 117.6315449097853048, 1.144802877355001192 ) ) ;
#5350 = CARTESIAN_POINT ( 'NONE',  ( -11.32678463655042478, 56.02547433970777035, -4.456118031212342068 ) ) ;
#5351 = CARTESIAN_POINT ( 'NONE',  ( -0.7718547489771787617, 119.9044272045951374, 0.6164056859965566515 ) ) ;
#5352 = CARTESIAN_POINT ( 'NONE',  ( 2.294499597581835193, -9.852027417895397932, -4.012603411698490774 ) ) ;
#5353 = EDGE_CURVE ( 'NONE', #22436, #16174, #26797, .T. ) ;
#5354 = CARTESIAN_POINT ( 'NONE',  ( -53.63638764239521350, 11.23543775674477807, 3.971736527645110648 ) ) ;
#5355 = CARTESIAN_POINT ( 'NONE',  ( -15.77830307927088249, 80.39606975582424297, -1.524000000000001798 ) ) ;
#5356 = CARTESIAN_POINT ( 'NONE',  ( 3.206936388013850614, -12.21552616865279006, 0.5380348851386724807 ) ) ;
#5357 = CARTESIAN_POINT ( 'NONE',  ( 1.980640663884704722, 106.8720524443079967, -4.823141945187445323 ) ) ;
#5358 = CARTESIAN_POINT ( 'NONE',  ( -26.37263903973852663, 72.23735686029533554, -1.524000000000005794 ) ) ;
#5359 = CARTESIAN_POINT ( 'NONE',  ( -6.441001096823943506, 29.32969738650800551, -0.01017983961634277151 ) ) ;
#5360 = DIRECTION ( 'NONE',  ( -4.017660918040594346E-17, 1.000000000000000000, 2.376309959284834438E-19 ) ) ;
#5361 = CARTESIAN_POINT ( 'NONE',  ( -0.2084201458593382406, 5.265951782950084592, 4.622859108429906883 ) ) ;
#5363 = EDGE_LOOP ( 'NONE', ( #4322, #31448, #25073, #34490 ) ) ;
#5362 = CARTESIAN_POINT ( 'NONE',  ( 5.654702199549676678, 159.1134716836843381, 0.5125381600378310365 ) ) ;
#5364 = CARTESIAN_POINT ( 'NONE',  ( 1.753713527278395468, 104.6144662015458096, -4.497131813391320954 ) ) ;
#5365 = CARTESIAN_POINT ( 'NONE',  ( 2.557542807212066283, -15.51814986354871451, 4.851437248720891660 ) ) ;
#5366 = CARTESIAN_POINT ( 'NONE',  ( -19.22350799451007575, 148.9694856701144090, 1.735702374547824389 ) ) ;
#5367 = AXIS2_PLACEMENT_3D ( 'NONE', #29426, #3670, #38606 ) ;
#5368 = CARTESIAN_POINT ( 'NONE',  ( -0.9749442489646007459, 26.91501818708639249, 0.01812370653153724809 ) ) ;
#5369 = CARTESIAN_POINT ( 'NONE',  ( 0.6724949529566155437, 16.91434809748496804, 0.7070771739444717818 ) ) ;
#5370 = ORIENTED_EDGE ( 'NONE', *, *, #19801, .F. ) ;
#5371 = ORIENTED_EDGE ( 'NONE', *, *, #4575, .F. ) ;
#5372 = CARTESIAN_POINT ( 'NONE',  ( -41.33672448130794663, 22.78954268934618810, 1.170983984347486961 ) ) ;
#5373 = CARTESIAN_POINT ( 'NONE',  ( 3.315449255180855204, 124.9344662015457743, 0.06625056644921942239 ) ) ;
#5374 = CARTESIAN_POINT ( 'NONE',  ( -5.877307974080659747, 120.8872308857076519, 0.5842564153471766497 ) ) ;
#5375 = CARTESIAN_POINT ( 'NONE',  ( 13.46199999999999797, 12.17394877578616708, 0.000000000000000000 ) ) ;
#5376 = CARTESIAN_POINT ( 'NONE',  ( 1.928300050954173450, -15.05328954375542772, 5.649432967411273765 ) ) ;
#5377 = CARTESIAN_POINT ( 'NONE',  ( 5.091199858995886451, 119.8577235299091228, -0.8121313320900890309 ) ) ;
#5378 = CARTESIAN_POINT ( 'NONE',  ( -13.90099558903415478, 123.5874490550988014, -1.899532866591826519 ) ) ;
#5379 = DIRECTION ( 'NONE',  ( -1.000000000000000000, 1.140319995778305956E-16, 0.000000000000000000 ) ) ;
#5380 = CARTESIAN_POINT ( 'NONE',  ( -0.02896191955447584981, 39.05846921699762220, 0.8727513426688231490 ) ) ;
#5381 = CARTESIAN_POINT ( 'NONE',  ( 9.439772580079011988, 124.2753396726362780, -0.1368060863603346999 ) ) ;
#5382 = VERTEX_POINT ( 'NONE', #19760 ) ;
#5383 = CARTESIAN_POINT ( 'NONE',  ( 3.220686968960577712, -14.48737495597347902, 2.486805533510040078 ) ) ;
#5384 = DIRECTION ( 'NONE',  ( -1.000000000000000000, 9.627370216492862708E-17, 0.000000000000000000 ) ) ;
#5385 = AXIS2_PLACEMENT_3D ( 'NONE', #20306, #23932, #16493 ) ;
#5386 = CIRCLE ( 'NONE', #18269, 0.6349999999999993427 ) ;
#5387 = CARTESIAN_POINT ( 'NONE',  ( 4.999358879416575974, 117.3993846089301911, 0.8254721163526904659 ) ) ;
#5388 = CARTESIAN_POINT ( 'NONE',  ( -48.44802435119614614, 18.63281525352784129, 5.198089189977588731 ) ) ;
#5389 = CARTESIAN_POINT ( 'NONE',  ( -3.339653329301207840, -2.245917679271888900, -3.199182135983138053 ) ) ;
#5390 = CARTESIAN_POINT ( 'NONE',  ( 10.39772550536720885, 123.9810924921358151, 1.245468829273463474 ) ) ;
#5391 = CARTESIAN_POINT ( 'NONE',  ( -3.312261290190312568, 29.35545767321095667, 2.878016369877077985 ) ) ;
#5392 = CARTESIAN_POINT ( 'NONE',  ( -5.205184729905311336, 115.4673366222922368, 1.303740999714490201 ) ) ;
#5393 = CARTESIAN_POINT ( 'NONE',  ( 0.09481320634720795393, -4.229605868409334057, 4.636458411128852930 ) ) ;
#5394 = CARTESIAN_POINT ( 'NONE',  ( 8.487687333566158898, 123.3253871723413368, 0.1696041924978713422 ) ) ;
#5395 = CARTESIAN_POINT ( 'NONE',  ( 3.645047284007026267, 5.522537913078280347, -7.602695550683356451 ) ) ;
#5396 = CARTESIAN_POINT ( 'NONE',  ( -56.89469692534096623, 2.545995565645275960, -0.6470027801917211940 ) ) ;
#5397 = CARTESIAN_POINT ( 'NONE',  ( -2.141217111143084217, 116.5628937121521176, -0.4137402603370525234 ) ) ;
#5398 = CARTESIAN_POINT ( 'NONE',  ( -0.1292312685654156412, 109.4728569552520554, -3.923176234211465552 ) ) ;
#5399 = CARTESIAN_POINT ( 'NONE',  ( -5.382937502775954980E-14, 83.56599999999998829, -1.904999999999999805 ) ) ;
#5400 = CARTESIAN_POINT ( 'NONE',  ( -7.992722778381481596, -7.251515252772184894, -2.728257467986670903 ) ) ;
#5401 = EDGE_CURVE ( 'NONE', #1824, #8452, #9771, .T. ) ;
#5402 = CARTESIAN_POINT ( 'NONE',  ( 1.957861286920753674, 117.9394489915384270, 1.364553959153947282 ) ) ;
#5403 = DIRECTION ( 'NONE',  ( 0.000000000000000000, -0.000000000000000000, 1.000000000000000000 ) ) ;
#5404 = CARTESIAN_POINT ( 'NONE',  ( -23.34387769576312621, 77.71194901948682343, -1.270000000000005125 ) ) ;
#5405 = CARTESIAN_POINT ( 'NONE',  ( 0.4040709798585657153, 123.7646714092001190, -0.1152108919326050862 ) ) ;
#5406 = CARTESIAN_POINT ( 'NONE',  ( -23.05883864707335817, 142.5499849734818838, 0.2756568390806650726 ) ) ;
#5407 = ORIENTED_EDGE ( 'NONE', *, *, #15141, .F. ) ;
#5408 = CARTESIAN_POINT ( 'NONE',  ( -58.26284211471887176, 1.387681237079871455, -0.7239480823116948294 ) ) ;
#5409 = VECTOR ( 'NONE', #6805, 1000.000000000000000 ) ;
#5410 = ORIENTED_EDGE ( 'NONE', *, *, #27398, .F. ) ;
#5411 = DIRECTION ( 'NONE',  ( -0.01997839162482737546, -1.040247600000940825E-18, 0.9998004120163610509 ) ) ;
#5412 = CARTESIAN_POINT ( 'NONE',  ( -8.741281759966728515, 123.6764614546807621, -0.1311366048815914842 ) ) ;
#5413 = CARTESIAN_POINT ( 'NONE',  ( 6.479796796485603139, -13.80134569450770776, 0.08439370571411514144 ) ) ;
#5414 = CARTESIAN_POINT ( 'NONE',  ( -15.00359386227412273, 154.7288491705591866, 1.534247969496847386 ) ) ;
#5415 = CARTESIAN_POINT ( 'NONE',  ( 17.95360460524294410, 154.0540368679750998, -0.8775891217286382329 ) ) ;
#5416 = CARTESIAN_POINT ( 'NONE',  ( 3.874746376330849618, 18.20996518813934628, -2.522041008920607563 ) ) ;
#5417 = CARTESIAN_POINT ( 'NONE',  ( -0.3142790036447159485, 116.6413645472259617, -0.2007485675953368798 ) ) ;
#5418 = CARTESIAN_POINT ( 'NONE',  ( -49.90791155052789918, 16.44236289295141873, -4.944395792362849207 ) ) ;
#5419 = VERTEX_POINT ( 'NONE', #13180 ) ;
#5420 = CARTESIAN_POINT ( 'NONE',  ( 5.560951712478671816, 116.7029514248484929, 0.1869645659760804934 ) ) ;
#5421 = CARTESIAN_POINT ( 'NONE',  ( -17.14500000000466784, 71.11999999999886768, -1.270000000000000684 ) ) ;
#5422 = CARTESIAN_POINT ( 'NONE',  ( -17.22187362939842359, 148.7218176724978775, 1.531815132551777259 ) ) ;
#5423 = CARTESIAN_POINT ( 'NONE',  ( -51.00679592072113877, 14.45111400903523169, -4.539175725115415005 ) ) ;
#5424 = CARTESIAN_POINT ( 'NONE',  ( 19.29290905409789758, 147.1635184732690220, -1.739861672056419506 ) ) ;
#5425 = CARTESIAN_POINT ( 'NONE',  ( -21.10215338253927797, 147.9292434580435724, -2.361242315759020993 ) ) ;
#5426 = CARTESIAN_POINT ( 'NONE',  ( -52.50198181065980663, 11.96455506022023307, -4.263607785004590589 ) ) ;
#5427 = CARTESIAN_POINT ( 'NONE',  ( 15.90968206782430983, 148.0001117310855250, -0.7891277450764202506 ) ) ;
#5428 = ORIENTED_EDGE ( 'NONE', *, *, #19832, .F. ) ;
#5429 = CARTESIAN_POINT ( 'NONE',  ( -8.234130529647242014, 121.1361926620737393, -1.330377128061139835 ) ) ;
#5430 = CARTESIAN_POINT ( 'NONE',  ( 1.868457900240735103, -15.55086107261449690, 5.421086310357067894 ) ) ;
#5431 = CARTESIAN_POINT ( 'NONE',  ( -4.065972646788793554, 118.2429491485453070, -0.3080848862740693250 ) ) ;
#5432 = CARTESIAN_POINT ( 'NONE',  ( -58.24807683554808335, 1.288543178753334573, -1.357556113208963744 ) ) ;
#5433 = CIRCLE ( 'NONE', #29220, 0.5080000000000002292 ) ;
#5434 = CARTESIAN_POINT ( 'NONE',  ( -4.792200577477630397, 117.5371802918334225, 0.9878184568134641408 ) ) ;
#5435 = CARTESIAN_POINT ( 'NONE',  ( 5.074328365123657925, 120.0747842884402132, 0.9638994778299828647 ) ) ;
#5436 = PLANE ( 'NONE',  #21230 ) ;
#5437 = CIRCLE ( 'NONE', #20363, 0.5080000000000014504 ) ;
#5438 = CARTESIAN_POINT ( 'NONE',  ( -5.377075248297400911, 4.191758615746518757, 6.528609652590111168 ) ) ;
#5439 = CARTESIAN_POINT ( 'NONE',  ( 5.911602206138902638, 121.5031286879076902, 0.2921876764073587651 ) ) ;
#5440 = DIRECTION ( 'NONE',  ( -1.000000000000000000, -6.353134868986659519E-16, -0.000000000000000000 ) ) ;
#5442 = ORIENTED_EDGE ( 'NONE', *, *, #38816, .F. ) ;
#5441 = CARTESIAN_POINT ( 'NONE',  ( -41.05189575270516400, 23.09451173561988213, -0.9172222222222270460 ) ) ;
#5443 = CARTESIAN_POINT ( 'NONE',  ( 0.000000000000000000, 0.000000000000000000, 0.000000000000000000 ) ) ;
#5444 = CARTESIAN_POINT ( 'NONE',  ( -23.91048590848665611, 81.84235438443283783, -1.270000000000006235 ) ) ;
#5445 = CARTESIAN_POINT ( 'NONE',  ( -38.65395868481546415, 29.38327706004843876, -1.270000000000004903 ) ) ;
#5446 = CARTESIAN_POINT ( 'NONE',  ( -52.43464216530867361, 18.97776253654341616, 0.3470174342361194708 ) ) ;
#5447 = CARTESIAN_POINT ( 'NONE',  ( -0.001838942458917565501, 116.4858755864912183, 0.09202820039585841994 ) ) ;
#5448 = ORIENTED_EDGE ( 'NONE', *, *, #10739, .F. ) ;
#5449 = CARTESIAN_POINT ( 'NONE',  ( -48.26009918843823954, 20.16784055841990764, -4.711418872450288120 ) ) ;
#5450 = CARTESIAN_POINT ( 'NONE',  ( -6.877540358266958975, 121.7309737470392434, -0.6052161323226827871 ) ) ;
#5451 = CARTESIAN_POINT ( 'NONE',  ( -7.794969618782333853, 122.5994144667442498, -0.004875387122262515339 ) ) ;
#5452 = ORIENTED_EDGE ( 'NONE', *, *, #23772, .T. ) ;
#5453 = CARTESIAN_POINT ( 'NONE',  ( 0.03523692298162432734, 115.6909491485452719, -1.763399716048400734 ) ) ;
#5454 = CARTESIAN_POINT ( 'NONE',  ( -9.153275543502907396, 153.8946005065304803, -0.4698995960908562419 ) ) ;
#5455 = CARTESIAN_POINT ( 'NONE',  ( 5.856266048228023990, -12.49204451700697227, 1.108958003446382845 ) ) ;
#5456 = CARTESIAN_POINT ( 'NONE',  ( -21.26362230212582816, 150.1117090729339623, 1.276404781699089996 ) ) ;
#5457 = CARTESIAN_POINT ( 'NONE',  ( 5.177913976931196594, 78.94499979771845233, -5.372100000000001430 ) ) ;
#5458 = CARTESIAN_POINT ( 'NONE',  ( 15.84538651563799050, 121.0146182718019645, 0.4760991727851862088 ) ) ;
#5459 = CARTESIAN_POINT ( 'NONE',  ( 15.76023951477780294, 145.9043208129480433, 0.3821549961928484840 ) ) ;
#5460 = DIRECTION ( 'NONE',  ( -5.188838149069472160E-16, 1.699382548006136559E-16, 1.000000000000000000 ) ) ;
#5461 = CARTESIAN_POINT ( 'NONE',  ( -0.009113691291695666039, 25.33460033795575583, 0.9756159547818916700 ) ) ;
#5462 = CARTESIAN_POINT ( 'NONE',  ( -4.723387343850809827, 116.7592613395855352, -0.1361797943638454467 ) ) ;
#5463 = DIRECTION ( 'NONE',  ( 0.9807655518882955059, -0.1951894777626270172, 8.537024980200854359E-16 ) ) ;
#5464 = TOROIDAL_SURFACE ( 'NONE', #14946, 3.683000000000000718, 0.5080000000000000071 ) ;
#5465 = DIRECTION ( 'NONE',  ( -5.463695987328526437E-16, 1.000000000000000000, 1.672774450599033775E-31 ) ) ;
#5466 = ORIENTED_EDGE ( 'NONE', *, *, #25402, .F. ) ;
#5467 = CARTESIAN_POINT ( 'NONE',  ( -6.079585152903477230, 118.8420829952417535, 0.9834774059785402756 ) ) ;
#5468 = CARTESIAN_POINT ( 'NONE',  ( -3.942997264624582776, -11.51663297089948479, -2.426127359622226809 ) ) ;
#5469 = CARTESIAN_POINT ( 'NONE',  ( 20.86915823776852008, 136.4823663107028722, 1.950121757083878249 ) ) ;
#5470 = CARTESIAN_POINT ( 'NONE',  ( 20.39294766749429755, 148.4497675966422889, -1.664483663417329673 ) ) ;
#5471 = CARTESIAN_POINT ( 'NONE',  ( -8.001679540263406665, 18.69059125004590172, 2.668541714186715819 ) ) ;
#5472 = CARTESIAN_POINT ( 'NONE',  ( -1.281755300609965120, 159.3505072347868747, -0.9987438389826045482 ) ) ;
#5473 = CARTESIAN_POINT ( 'NONE',  ( 4.932541054738843300, 117.5465815472490192, -0.8858376886457886012 ) ) ;
#5474 = CARTESIAN_POINT ( 'NONE',  ( 7.474242191267162383, 123.6620266863018855, 0.1838331482465498379 ) ) ;
#5475 = ORIENTED_EDGE ( 'NONE', *, *, #32093, .T. ) ;
#5476 = CARTESIAN_POINT ( 'NONE',  ( -6.497458072406325336, 121.7745328324513139, -0.05723077286956937404 ) ) ;
#5477 = CARTESIAN_POINT ( 'NONE',  ( -18.98749958112902902, 148.5750135429820205, -2.495758040776018927 ) ) ;
#5478 = CARTESIAN_POINT ( 'NONE',  ( 5.316001070410483642, -15.20466279102368468, 3.045604417706107458 ) ) ;
#5479 = LINE ( 'NONE', #37217, #23356 ) ;
#5480 = AXIS2_PLACEMENT_3D ( 'NONE', #19956, #36168, #15913 ) ;
#5481 = FACE_OUTER_BOUND ( 'NONE', #32919, .T. ) ;
#5482 = ORIENTED_EDGE ( 'NONE', *, *, #29960, .F. ) ;
#5483 = CARTESIAN_POINT ( 'NONE',  ( 11.65353862096119641, 154.7938929448963279, 2.201148936174281534 ) ) ;
#5484 = DIRECTION ( 'NONE',  ( 0.000000000000000000, 1.000000000000000000, 0.000000000000000000 ) ) ;
#5485 = AXIS2_PLACEMENT_3D ( 'NONE', #1085, #8088, #10443 ) ;
#5486 = DIRECTION ( 'NONE',  ( 4.017660918040594346E-17, -1.000000000000000000, -2.376309959284834438E-19 ) ) ;
#5487 = CARTESIAN_POINT ( 'NONE',  ( -2.102284131448474369, 122.9394440205640961, 0.1126375150955782195 ) ) ;
#5488 = CARTESIAN_POINT ( 'NONE',  ( -0.5966991250155297966, -8.296908750894687046, 8.413794654835093922 ) ) ;
#5489 = CARTESIAN_POINT ( 'NONE',  ( 0.6895396258585522187, 156.3865044363621450, 0.6062415235663760615 ) ) ;
#5490 = CARTESIAN_POINT ( 'NONE',  ( -5.219367156868218061, 115.6909491485453003, -1.134611224921844963 ) ) ;
#5491 = CARTESIAN_POINT ( 'NONE',  ( 3.184986510633057488, 159.3937097445585778, -0.5650791069852592052 ) ) ;
#5492 = CARTESIAN_POINT ( 'NONE',  ( 5.353961914031110325, 56.51499999999804658, -5.213928161110970905 ) ) ;
#5493 = CARTESIAN_POINT ( 'NONE',  ( -58.05284929258671411, 0.3898940286592555982, 0.7867345219013538449 ) ) ;
#5494 = CARTESIAN_POINT ( 'NONE',  ( 8.798408771645801707, 117.6899328986124402, 0.1004551508774383928 ) ) ;
#5495 = CIRCLE ( 'NONE', #29299, 0.2539999999999956737 ) ;
#5496 = EDGE_CURVE ( 'NONE', #41032, #12622, #5711, .T. ) ;
#5497 = ADVANCED_FACE ( 'NONE', ( #9875 ), #26122, .T. ) ;
#5498 = CARTESIAN_POINT ( 'NONE',  ( 2.083301838685657881, -15.46665383083971790, 5.961979448439958418 ) ) ;
#5499 = CARTESIAN_POINT ( 'NONE',  ( -4.239777078203335492, 118.2238256456127061, 0.3214240529150897974 ) ) ;
#5500 = CARTESIAN_POINT ( 'NONE',  ( -15.73471677569744287, 120.8416612192341972, -0.3144170877231853845 ) ) ;
#5501 = ORIENTED_EDGE ( 'NONE', *, *, #13894, .F. ) ;
#5502 = CARTESIAN_POINT ( 'NONE',  ( -49.66210360255988832, 16.76989353321783227, 4.946330335750482199 ) ) ;
#5503 = CARTESIAN_POINT ( 'NONE',  ( -4.317885076038099790, 119.4472151493546761, -0.9270640149902646954 ) ) ;
#5504 = DIRECTION ( 'NONE',  ( -0.1469470846586743706, 0.000000000000000000, -0.9891443546370348727 ) ) ;
#5505 = CARTESIAN_POINT ( 'NONE',  ( -10.15204665306235476, 124.8647468421599598, -0.8418846390287857417 ) ) ;
#5506 = CARTESIAN_POINT ( 'NONE',  ( -19.86616884172038766, 72.62886460123898758, 1.523999999999996691 ) ) ;
#5507 = AXIS2_PLACEMENT_3D ( 'NONE', #15024, #2277, #34429 ) ;
#5508 = CARTESIAN_POINT ( 'NONE',  ( 0.2378307671391127198, 117.3993841993812453, -1.487622118729645893 ) ) ;
#5509 = ORIENTED_EDGE ( 'NONE', *, *, #9443, .T. ) ;
#5510 = CARTESIAN_POINT ( 'NONE',  ( -3.130497002865707312, 23.39511390029671745, 3.426874451367011520 ) ) ;
#5511 = CARTESIAN_POINT ( 'NONE',  ( -30.83281893229463932, 55.49295607038747846, 1.523999999999994914 ) ) ;
#5512 = CARTESIAN_POINT ( 'NONE',  ( -41.08172402297500270, 23.06268970576013189, -1.270028526666295621 ) ) ;
#5513 = DIRECTION ( 'NONE',  ( 6.146657985744592735E-16, 3.905054717696927382E-31, 1.000000000000000000 ) ) ;
#5514 = CARTESIAN_POINT ( 'NONE',  ( -41.05189575270519242, 23.09451173561980042, 1.269999999999989582 ) ) ;
#5515 = CARTESIAN_POINT ( 'NONE',  ( -7.786259069948810563, 122.6240336826886050, -0.1181640060794083291 ) ) ;
#5516 = CYLINDRICAL_SURFACE ( 'NONE', #34093, 0.2539999999999942859 ) ;
#5517 = CARTESIAN_POINT ( 'NONE',  ( 20.20545065706713572, 152.4988772720997190, 1.451042778694937585 ) ) ;
#5518 = CARTESIAN_POINT ( 'NONE',  ( 4.722155446386091526, 104.6144662015456817, -1.045890991608505960 ) ) ;
#5520 = CARTESIAN_POINT ( 'NONE',  ( 18.85936551755639101, 131.8417273817641444, -1.350502370828212229 ) ) ;
#5519 = CARTESIAN_POINT ( 'NONE',  ( 3.221942100833175893, -14.53498920702628361, 2.661941298785070575 ) ) ;
#5521 = VECTOR ( 'NONE', #18287, 1000.000000000000000 ) ;
#5522 = CARTESIAN_POINT ( 'NONE',  ( -0.5282936316508035635, 119.4440140289964774, 0.5434071943388012471 ) ) ;
#5523 = CARTESIAN_POINT ( 'NONE',  ( 3.724956840101937505, 21.94285949141939440, 2.734508905299370518 ) ) ;
#5524 = CARTESIAN_POINT ( 'NONE',  ( -18.24338043389154507, 154.1370782493726210, -1.275500441016771402 ) ) ;
#5525 = CARTESIAN_POINT ( 'NONE',  ( -0.8533247626149625953, -2.668348290978065140, -0.4694259674561338525 ) ) ;
#5526 = ORIENTED_EDGE ( 'NONE', *, *, #16135, .T. ) ;
#5527 = CARTESIAN_POINT ( 'NONE',  ( -55.03835892454119261, 5.996057868307938854, 1.012875379724323288 ) ) ;
#5528 = CARTESIAN_POINT ( 'NONE',  ( -15.50313878892752939, 143.5853813351167219, 0.4270882868188066173 ) ) ;
#5529 = CARTESIAN_POINT ( 'NONE',  ( 5.396235140300779776, -11.83248475511457976, 0.6634469457710948648 ) ) ;
#5530 = CARTESIAN_POINT ( 'NONE',  ( 12.65121035427608298, 128.4643691153342218, -0.9906145297030367614 ) ) ;
#5531 = VERTEX_POINT ( 'NONE', #947 ) ;
#5532 = CARTESIAN_POINT ( 'NONE',  ( 0.5744245648901143975, 115.7029491485453718, 1.760676250340797777 ) ) ;
#5533 = CARTESIAN_POINT ( 'NONE',  ( -4.860056194691428466, 117.7242711327382239, -0.9629742322061086712 ) ) ;
#5534 = EDGE_CURVE ( 'NONE', #32767, #27965, #19456, .T. ) ;
#5535 = CARTESIAN_POINT ( 'NONE',  ( 7.788912029362537126, 154.6472212274131550, 0.1129171994251849803 ) ) ;
#5536 = VERTEX_POINT ( 'NONE', #19664 ) ;
#5537 = CARTESIAN_POINT ( 'NONE',  ( 19.91185195753428516, 145.3736917597469471, 2.515063280254572042 ) ) ;
#5538 = CARTESIAN_POINT ( 'NONE',  ( -5.241362157049126225, 57.14999999999999147, 5.310945289804169356 ) ) ;
#5539 = FACE_OUTER_BOUND ( 'NONE', #28619, .T. ) ;
#5540 = AXIS2_PLACEMENT_3D ( 'NONE', #20060, #13686, #33081 ) ;
#5541 = DIRECTION ( 'NONE',  ( 5.188838149069472160E-16, -1.699382548006136559E-16, -1.000000000000000000 ) ) ;
#5542 = CARTESIAN_POINT ( 'NONE',  ( 22.80463473692766740, 150.3987591554885626, 0.1267456695372862208 ) ) ;
#5543 = CARTESIAN_POINT ( 'NONE',  ( -4.781543117819943234, 56.51500000000003610, -4.872198453344445568 ) ) ;
#5544 = CIRCLE ( 'NONE', #24577, 5.588000000000006295 ) ;
#5545 = B_SPLINE_CURVE_WITH_KNOTS ( 'NONE', 3,
 ( #26177, #38763, #3193, #25756, #29378, #431 ),
 .UNSPECIFIED., .F., .F.,
 ( 4, 2, 4 ),
 ( 0.000000000000000000, 0.5000000000000000000, 1.000000000000000000 ),
 .UNSPECIFIED. ) ;
#5546 = CARTESIAN_POINT ( 'NONE',  ( 1.717835917352494635, -15.15497214477301569, 5.627788587114283203 ) ) ;
#5547 = CYLINDRICAL_SURFACE ( 'NONE', #26967, 3.175000000000001155 ) ;
#5548 = CARTESIAN_POINT ( 'NONE',  ( -41.26650320839694785, 23.23696823412480583, -1.524000000000005128 ) ) ;
#5549 = EDGE_CURVE ( 'NONE', #16059, #22469, #1632, .T. ) ;
#5550 = CARTESIAN_POINT ( 'NONE',  ( -4.706501277415600981, 117.8934301135909095, 0.8007959269290801929 ) ) ;
#5551 = ORIENTED_EDGE ( 'NONE', *, *, #15474, .F. ) ;
#5552 = EDGE_LOOP ( 'NONE', ( #27301, #37486, #19163, #32871 ) ) ;
#5553 = DIRECTION ( 'NONE',  ( -0.9998004120163608288, -4.016384292689131511E-17, -0.01997839162482749342 ) ) ;
#5554 = CARTESIAN_POINT ( 'NONE',  ( 5.779644130035700655, 118.6808122264324084, -0.9965243451110286088 ) ) ;
#5555 = CARTESIAN_POINT ( 'NONE',  ( 0.1065646865915093333, 105.8844662015456777, -5.332932678536312032 ) ) ;
#5556 = CARTESIAN_POINT ( 'NONE',  ( 4.842532773218567677, 117.4782487948497902, 1.162086725208648863 ) ) ;
#5557 = AXIS2_PLACEMENT_3D ( 'NONE', #24369, #4812, #18182 ) ;
#5558 = LINE ( 'NONE', #27285, #29085 ) ;
#5559 = CARTESIAN_POINT ( 'NONE',  ( -0.3839444928497607878, 119.8383472832136931, 0.6866461459122013000 ) ) ;
#5560 = CARTESIAN_POINT ( 'NONE',  ( 4.560200836559435977, -11.68919918208664122, 0.6963878748952898601 ) ) ;
#5561 = CARTESIAN_POINT ( 'NONE',  ( 3.682264917456191888, 97.37546620154573418, 0.07358041635424013294 ) ) ;
#5562 = CARTESIAN_POINT ( 'NONE',  ( 0.1116392523994730462, 39.20946620154573736, -5.586884702347429510 ) ) ;
#5563 = CARTESIAN_POINT ( 'NONE',  ( 1.897380780832740532, -15.05783359004129984, 5.662421594695133287 ) ) ;
#5564 = CARTESIAN_POINT ( 'NONE',  ( 5.756868464772053606, 120.3160329940760818, -0.2053529492706007153 ) ) ;
#5565 = CARTESIAN_POINT ( 'NONE',  ( -5.103418814394366620, 120.3680889145531552, -0.8767301089910150003 ) ) ;
#5566 = EDGE_CURVE ( 'NONE', #26975, #29909, #36507, .T. ) ;
#5567 = CARTESIAN_POINT ( 'NONE',  ( -6.067023846813282439, 121.4357121891808191, -0.1206843736590161587 ) ) ;
#5568 = DIRECTION ( 'NONE',  ( 4.017660918040594346E-17, -1.000000000000000000, -2.376309959284834438E-19 ) ) ;
#5569 = CARTESIAN_POINT ( 'NONE',  ( 2.003160574663116034, 15.61121511114846960, 4.187759092076685619 ) ) ;
#5571 = ORIENTED_EDGE ( 'NONE', *, *, #14629, .F. ) ;
#5570 = CARTESIAN_POINT ( 'NONE',  ( 22.96526709448173165, 149.8455236008688303, 1.052246632350672950 ) ) ;
#5572 = CARTESIAN_POINT ( 'NONE',  ( -0.8085285286411788563, 104.6144662015543361, -5.283841362478505665 ) ) ;
#5573 = CARTESIAN_POINT ( 'NONE',  ( 2.429471885602138670, -15.51652123318236676, 4.968198114871331228 ) ) ;
#5574 = CARTESIAN_POINT ( 'NONE',  ( -11.67114148714794730, 122.1450671466348439, 1.284540048876763096 ) ) ;
#5575 = AXIS2_PLACEMENT_3D ( 'NONE', #8731, #21693, #25336 ) ;
#5576 = CARTESIAN_POINT ( 'NONE',  ( -0.3022039251088723399, 24.96921649940425425, -0.9259629999792299282 ) ) ;
#5577 = VECTOR ( 'NONE', #19668, 1000.000000000000227 ) ;
#5578 = CARTESIAN_POINT ( 'NONE',  ( -0.6941440390767986690, 12.16465383894776409, -0.6855803344193639459 ) ) ;
#5579 = ORIENTED_EDGE ( 'NONE', *, *, #31004, .T. ) ;
#5580 = ORIENTED_EDGE ( 'NONE', *, *, #34715, .F. ) ;
#5581 = DIRECTION ( 'NONE',  ( -0.1715592850456333085, -0.1224830539174543292, 0.9775302108976914317 ) ) ;
#5582 = CARTESIAN_POINT ( 'NONE',  ( 5.854942301702412699, 124.9344662015456890, 0.1169956811762814242 ) ) ;
#5583 =( NAMED_UNIT ( * ) SI_UNIT ( $, .STERADIAN. ) SOLID_ANGLE_UNIT ( ) );
#5584 = CARTESIAN_POINT ( 'NONE',  ( -16.26403174311784028, 147.1082353761072454, 0.7878939306839422008 ) ) ;
#5585 = ADVANCED_FACE ( 'NONE', ( #16474, #39495 ), #32678, .F. ) ;
#5586 = CARTESIAN_POINT ( 'NONE',  ( 6.057513928997550146, 86.35999999999998522, -1.904999999999999805 ) ) ;
#5587 = CARTESIAN_POINT ( 'NONE',  ( 3.722123463297008605, -13.62806973238828157, 3.608531954378976891 ) ) ;
#5588 = CARTESIAN_POINT ( 'NONE',  ( 15.69153790699141027, 150.8349565870724120, -1.587821608835076503 ) ) ;
#5589 =( REPRESENTATION_RELATIONSHIP ('NONE','NONE', #30767, #26424 ) REPRESENTATION_RELATIONSHIP_WITH_TRANSFORMATION ( #17653 )SHAPE_REPRESENTATION_RELATIONSHIP( ) );
#5590 = CARTESIAN_POINT ( 'NONE',  ( -16.68944084648544646, 128.5636217276695561, -2.149857652400630759 ) ) ;
#5591 = CARTESIAN_POINT ( 'NONE',  ( -29.48103325898055971, 60.42855201934086296, 1.523999999999994026 ) ) ;
#5592 = CARTESIAN_POINT ( 'NONE',  ( -12.85860202769644545, 133.7716054015561156, -0.2569454702854385153 ) ) ;
#5593 = CARTESIAN_POINT ( 'NONE',  ( 4.074910602682932925, 118.2429491485453354, -0.1454311599470142491 ) ) ;
#5594 = CARTESIAN_POINT ( 'NONE',  ( 9.317815699932298301, 124.0984330410602183, -0.1356161447201455761 ) ) ;
#5595 = VERTEX_POINT ( 'NONE', #7126 ) ;
#5596 = CARTESIAN_POINT ( 'NONE',  ( 2.459637058406862309, -15.11974833578012856, 4.824092508607692231 ) ) ;
#5597 = CARTESIAN_POINT ( 'NONE',  ( -4.466782427718574588, 71.06098887363195615, -1.269999999999994245 ) ) ;
#5598 = EDGE_CURVE ( 'NONE', #27342, #23556, #41098, .T. ) ;
#5599 = LINE ( 'NONE', #24957, #36807 ) ;
#5600 = ADVANCED_FACE ( 'NONE', ( #26272 ), #8525, .F. ) ;
#5601 = CARTESIAN_POINT ( 'NONE',  ( -57.99063839910164830, 1.082714195262735046, 1.370926835928194976 ) ) ;
#5602 = CARTESIAN_POINT ( 'NONE',  ( 0.2036312542886812293, -3.545347522689146214, -4.628372119175537591 ) ) ;
#5603 = CARTESIAN_POINT ( 'NONE',  ( 16.42797441217041765, 147.8801373804967341, 1.766026403434534098 ) ) ;
#5604 = DIRECTION ( 'NONE',  ( 5.188838149069472160E-16, -1.699382548006136559E-16, -1.000000000000000000 ) ) ;
#5605 = CARTESIAN_POINT ( 'NONE',  ( -2.668012146925317740, 107.2306503360107541, 4.624472725681509466 ) ) ;
#5606 = AXIS2_PLACEMENT_3D ( 'NONE', #11506, #30065, #7285 ) ;
#5607 = CARTESIAN_POINT ( 'NONE',  ( -4.550674770548566173, 2.667180226961371137, -0.8080508602523945871 ) ) ;
#5608 = CARTESIAN_POINT ( 'NONE',  ( 5.308493528853203358, 121.3525139070573147, 0.1060763342189516983 ) ) ;
#5609 = ADVANCED_FACE ( 'NONE', ( #39282 ), #39057, .T. ) ;
#5610 = CARTESIAN_POINT ( 'NONE',  ( -7.571256676022106724, -0.2985773316772562525, 3.683590697331973196 ) ) ;
#5611 = CARTESIAN_POINT ( 'NONE',  ( -57.51979792895002674, 1.380172231454854348, -0.6550001595470087423 ) ) ;
#5612 = CARTESIAN_POINT ( 'NONE',  ( -2.148791889500600405, 116.6464491036702640, -0.4521275957688462022 ) ) ;
#5613 = CARTESIAN_POINT ( 'NONE',  ( -1.058122102717379942, 124.9344662015457459, -0.02114379780294260366 ) ) ;
#5614 = LINE ( 'NONE', #24534, #15098 ) ;
#5615 = DIRECTION ( 'NONE',  ( -5.188838149069471174E-16, 1.699382548006136313E-16, 1.000000000000000000 ) ) ;
#5616 = CARTESIAN_POINT ( 'NONE',  ( -8.268995186617910775, -7.056286353048313309, -1.660136952399225319 ) ) ;
#5617 = CARTESIAN_POINT ( 'NONE',  ( 0.3344074102203439813, 117.9394486947857814, 1.410084100385009531 ) ) ;
#5618 = DIRECTION ( 'NONE',  ( -1.000000000000000000, 0.000000000000000000, 0.000000000000000000 ) ) ;
#5619 = DIRECTION ( 'NONE',  ( -0.000000000000000000, -0.000000000000000000, -1.000000000000000000 ) ) ;
#5620 = CARTESIAN_POINT ( 'NONE',  ( 0.3781434503561393878, 120.9711055683163323, -0.4753422346318206815 ) ) ;
#5621 = CARTESIAN_POINT ( 'NONE',  ( -16.81386451639902901, 122.6968688451475771, 0.2091777910580985833 ) ) ;
#5622 = ORIENTED_EDGE ( 'NONE', *, *, #38069, .F. ) ;
#5623 = CARTESIAN_POINT ( 'NONE',  ( -58.40930376703802551, 1.028767233150276628, -0.4283228411258474533 ) ) ;
#5624 = ORIENTED_EDGE ( 'NONE', *, *, #2230, .F. ) ;
#5625 = DIRECTION ( 'NONE',  ( 0.9998004120163608288, 4.016384292689131511E-17, 0.01997839162482749342 ) ) ;
#5626 = CARTESIAN_POINT ( 'NONE',  ( -15.72656178636810331, 146.8976252942685505, -0.1802331088929658987 ) ) ;
#5627 = CARTESIAN_POINT ( 'NONE',  ( 2.659284927817582744, -15.52939239755456136, 5.761088356787748666 ) ) ;
#5628 = CARTESIAN_POINT ( 'NONE',  ( -3.179094171403719304, 118.3302933575512412, 0.7469981754565537813 ) ) ;
#5629 = CARTESIAN_POINT ( 'NONE',  ( 1.068372181839128965, 117.3444111807523882, -0.4585463030235086834 ) ) ;
#5630 = CARTESIAN_POINT ( 'NONE',  ( -2.359559261509405204, 14.11188314818778267, 3.974389579228013503 ) ) ;
#5631 = CARTESIAN_POINT ( 'NONE',  ( -15.37635245578029419, 120.8297411738997624, -0.7275678838439406659 ) ) ;
#5632 = CARTESIAN_POINT ( 'NONE',  ( -58.17229861323505702, 0.6892682111524470745, -1.169530247053243821 ) ) ;
#5633 = EDGE_CURVE ( 'NONE', #2940, #2461, #33618, .T. ) ;
#5634 = ORIENTED_EDGE ( 'NONE', *, *, #2083, .T. ) ;
#5635 = CARTESIAN_POINT ( 'NONE',  ( -2.182332153758789417, 116.1897970675078255, -0.04360822100441016230 ) ) ;
#5636 = DIRECTION ( 'NONE',  ( -0.8745520943968243532, 0.4849315768086547296, -6.829619984160642269E-16 ) ) ;
#5637 = CARTESIAN_POINT ( 'NONE',  ( -16.62515567699083618, 149.4842840675632658, 1.536177446654198198 ) ) ;
#5638 = CARTESIAN_POINT ( 'NONE',  ( -54.63495462180135576, 7.558260771377723231, -3.173136904912474243 ) ) ;
#5639 = CARTESIAN_POINT ( 'NONE',  ( 0.03245814172805025488, 157.7902383798253538, -1.624338139048501439 ) ) ;
#5640 = CARTESIAN_POINT ( 'NONE',  ( -12.91357091396832146, 121.2479969211051127, -1.612259173617573094 ) ) ;
#5641 = CARTESIAN_POINT ( 'NONE',  ( -56.34046819891496938, 4.202508019718290022, -2.501728563949862760 ) ) ;
#5642 = AXIS2_PLACEMENT_3D ( 'NONE', #33119, #13299, #3948 ) ;
#5643 = CARTESIAN_POINT ( 'NONE',  ( 16.17714305270723685, 147.4171829256358137, -0.7878123557203797755 ) ) ;
#5644 = B_SPLINE_CURVE_WITH_KNOTS ( 'NONE', 3,
 ( #21446, #34476, #12096, #21872, #25084, #41504, #12310, #5309, #31476, #38091 ),
 .UNSPECIFIED., .F., .F.,
 ( 4, 2, 2, 2, 4 ),
 ( -0.0004895961982421361599, 0.0005229314014804232590, 0.001535459001202982678, 0.002547986600925542314, 0.003560514200648101299 ),
 .UNSPECIFIED. ) ;
#5645 = ORIENTED_EDGE ( 'NONE', *, *, #34502, .T. ) ;
#5646 = CARTESIAN_POINT ( 'NONE',  ( -2.462641994822475144, 119.6096776070104681, -0.7191205607878169426 ) ) ;
#5647 = CARTESIAN_POINT ( 'NONE',  ( 2.631420558634286255, -15.64638348417481062, 4.926794133592228064 ) ) ;
#5648 = CARTESIAN_POINT ( 'NONE',  ( -4.113113975211506457, 118.2429491485453070, -0.3449889555224052717 ) ) ;
#5649 = ADVANCED_FACE ( 'NONE', ( #29687 ), #15892, .F. ) ;
#5650 = CARTESIAN_POINT ( 'NONE',  ( -57.15088083682995546, 2.378576142695001838, -1.865916551128065981 ) ) ;
#5651 = AXIS2_PLACEMENT_3D ( 'NONE', #21369, #34196, #5655 ) ;
#5652 = EDGE_CURVE ( 'NONE', #31966, #35910, #20082, .T. ) ;
#5653 = CARTESIAN_POINT ( 'NONE',  ( -5.008553330431526618, 117.3993852298624745, 0.7755932876167446199 ) ) ;
#5654 = CARTESIAN_POINT ( 'NONE',  ( 17.44789039799410446, 148.6234142586927476, 2.276312578826294786 ) ) ;
#5655 = DIRECTION ( 'NONE',  ( -0.8745520943968230210, 0.4849315768086570611, -6.829619984160674809E-16 ) ) ;
#5656 = CARTESIAN_POINT ( 'NONE',  ( -0.5673920217975719771, -4.456920702667952483, 8.403146712094516246 ) ) ;
#5657 = CARTESIAN_POINT ( 'NONE',  ( 2.942445288855353169, 156.0884104482065595, 0.3607664148606970489 ) ) ;
#5658 = DIRECTION ( 'NONE',  ( -0.01731298258489111577, 0.9998501190848634312, 2.778415991487939406E-15 ) ) ;
#5660 = ORIENTED_EDGE ( 'NONE', *, *, #22168, .F. ) ;
#5659 = CARTESIAN_POINT ( 'NONE',  ( -6.096037513970406607, 78.08166987308820239, -1.269999999999996243 ) ) ;
#5661 = CARTESIAN_POINT ( 'NONE',  ( -1.006826980415389095, 118.1588900228295387, 0.8541050747360177109 ) ) ;
#5662 = CARTESIAN_POINT ( 'NONE',  ( -36.98328822617348521, 27.82293856516311692, 1.269999999999995577 ) ) ;
#5663 = DIRECTION ( 'NONE',  ( 0.3582377630123966261, -0.9336303900108832154, 0.000000000000000000 ) ) ;
#5664 = CIRCLE ( 'NONE', #40359, 0.3810000000000000053 ) ;
#5665 = FACE_OUTER_BOUND ( 'NONE', #37347, .T. ) ;
#5666 = CARTESIAN_POINT ( 'NONE',  ( -50.19988854512629217, 18.36332526648348917, 3.854797337117271017 ) ) ;
#5667 = CARTESIAN_POINT ( 'NONE',  ( -8.215251585939828516, 117.5146787832509858, -0.03113046551775517159 ) ) ;
#5668 = ORIENTED_EDGE ( 'NONE', *, *, #37538, .F. ) ;
#5669 = CARTESIAN_POINT ( 'NONE',  ( -49.65119436432973998, 19.91503915004672720, -3.137105223390908471 ) ) ;
#5670 = CARTESIAN_POINT ( 'NONE',  ( 7.858252769910347268, 122.3222094090309326, -0.3873341666547952533 ) ) ;
#5671 = LINE ( 'NONE', #31633, #35316 ) ;
#5672 = ORIENTED_EDGE ( 'NONE', *, *, #29504, .F. ) ;
#5673 = CARTESIAN_POINT ( 'NONE',  ( 2.370544184569783219, 115.7028721635570747, -1.611047144755549887 ) ) ;
#5674 = CARTESIAN_POINT ( 'NONE',  ( -9.185235947232945009, 124.1858035287836231, -0.2689572614166575448 ) ) ;
#5675 = CARTESIAN_POINT ( 'NONE',  ( 2.642260502442670855, -15.21879886190521880, 5.833332612881661383 ) ) ;
#5676 = CARTESIAN_POINT ( 'NONE',  ( -21.00062727315632927, 150.0074445146613584, 1.385517290469731266 ) ) ;
#5677 = CARTESIAN_POINT ( 'NONE',  ( 5.525651935317158703, 78.91763798174282840, -5.107334513333023018 ) ) ;
#5678 = CARTESIAN_POINT ( 'NONE',  ( 22.94033276177397340, 150.1476136049543868, 0.7879714733284358674 ) ) ;
#5679 = CARTESIAN_POINT ( 'NONE',  ( 14.67388681441289933, 148.8571912859537179, 0.3592780155011008336 ) ) ;
#5680 = CARTESIAN_POINT ( 'NONE',  ( -4.896144065122994604, 117.7626873562327603, 0.6092677679091855758 ) ) ;
#5681 = CARTESIAN_POINT ( 'NONE',  ( -0.5268263777171366957, 24.48095756788062261, 0.8226642508852344271 ) ) ;
#5682 = CARTESIAN_POINT ( 'NONE',  ( -13.42863190281036800, 156.9273374874128137, -0.3327859972200287175 ) ) ;
#5683 = CARTESIAN_POINT ( 'NONE',  ( -38.65395868481546415, 29.38327706004843876, 1.269999999999994245 ) ) ;
#5684 = FACE_OUTER_BOUND ( 'NONE', #13749, .T. ) ;
#5685 = VERTEX_POINT ( 'NONE', #26491 ) ;
#5686 = CARTESIAN_POINT ( 'NONE',  ( 6.113542531766674948, 119.0002034676630416, 1.241036244702666380 ) ) ;
#5687 = DIRECTION ( 'NONE',  ( -0.9998239923360758841, 0.01876124593811817620, 8.953619244849184656E-16 ) ) ;
#5688 = CARTESIAN_POINT ( 'NONE',  ( 5.210988722241143734, 158.8115599018184412, 1.325654878232527700 ) ) ;
#5689 = CARTESIAN_POINT ( 'NONE',  ( 0.03067001211929459153, 158.6015251912307633, -1.534852821454057548 ) ) ;
#5690 = CARTESIAN_POINT ( 'NONE',  ( 0.2322036383927537639, 20.64316925235604216, 8.417729739967510838 ) ) ;
#5691 = CARTESIAN_POINT ( 'NONE',  ( -9.366440581936362975, 118.7255599110314961, -1.127239873969282602 ) ) ;
#5692 = CARTESIAN_POINT ( 'NONE',  ( 4.755450631031003184, 117.7575004727687400, -0.8921683121825315643 ) ) ;
#5693 = CARTESIAN_POINT ( 'NONE',  ( 4.366878780879478228, 111.2667756541687538, 3.131538613950388239 ) ) ;
#5694 = CARTESIAN_POINT ( 'NONE',  ( -0.001255909994593423394, 120.9722815239556439, 0.06285087176068931969 ) ) ;
#5695 = CARTESIAN_POINT ( 'NONE',  ( -5.971676678096491386, 157.1185343457808301, -1.951309749225692336 ) ) ;
#5696 = CARTESIAN_POINT ( 'NONE',  ( 2.449088499779481953, -15.60605025760848719, 5.768239595176595458 ) ) ;
#5697 = PRESENTATION_LAYER_ASSIGNMENT (  '', '', ( #11115 ) ) ;
#5698 = DIRECTION ( 'NONE',  ( 3.035386659626960118E-16, -0.000000000000000000, 1.000000000000000000 ) ) ;
#5699 = CARTESIAN_POINT ( 'NONE',  ( -41.18107378286554621, 22.95619949144852967, -1.523999999999998023 ) ) ;
#5700 = CIRCLE ( 'NONE', #14515, 0.2539999999999998925 ) ;
#5701 = ORIENTED_EDGE ( 'NONE', *, *, #33419, .F. ) ;
#5702 = CARTESIAN_POINT ( 'NONE',  ( 18.35995883219814928, 144.7751241387205425, 2.452750363274776912 ) ) ;
#5703 = SURFACE_STYLE_FILL_AREA ( #18661 ) ;
#5704 = CARTESIAN_POINT ( 'NONE',  ( 5.008145224984434485, 117.3993836135855418, -0.7758584094373792706 ) ) ;
#5705 = AXIS2_PLACEMENT_3D ( 'NONE', #23947, #4179, #27364 ) ;
#5706 = CARTESIAN_POINT ( 'NONE',  ( -1.751097875589126440, 120.5851793143259130, 0.4017021596164531139 ) ) ;
#5707 = CARTESIAN_POINT ( 'NONE',  ( -7.571256676022106724, -0.2985773316772562525, 3.683590697331973196 ) ) ;
#5708 = CARTESIAN_POINT ( 'NONE',  ( 7.694217360203059464, 122.2455405838764335, 0.6631844599531894202 ) ) ;
#5709 = CARTESIAN_POINT ( 'NONE',  ( 14.60500000000000043, 71.11999999999999034, 5.016499999999999737 ) ) ;
#5710 = CARTESIAN_POINT ( 'NONE',  ( 16.58356254348269587, 122.7279807066903032, -0.3948093068319185606 ) ) ;
#5711 = B_SPLINE_CURVE_WITH_KNOTS ( 'NONE', 3,
 ( #26167, #9976, #2978, #22950, #38751, #10188, #420, #35976, #32782, #26377, #7015, #19983, #3828, #12756, #25541, #16792, #9560, #22319, #32146, #15942, #28937, #10821, #17623, #27432, #30625, #16998, #30209, #40028, #10404, #33632, #8051, #837, #17211, #14425, #36824, #13812, #33838, #37233, #14012, #1049, #26810, #39601, #17417, #36615, #40239, #27019, #24015, #39818, #20812, #4249, #1468, #24222, #20601, #33418, #23804, #13602, #26592, #27226, #23376, #40446, #11238, #10611, #36409, #20392, #632, #4460, #21024, #7642, #7227, #23593, #30414, #11034, #34047, #7851, #37034, #1262, #4877, #20186, #14217, #7434, #29793, #33212, #4666, #4037, #29998, #31835, #25233, #6075, #16048, #18830, #9464, #1677, #8255, #22428, #2674, #25851, #14632, #35047, #15632, #3089, #28636, #41648, #12455, #38656, #38237, #5868, #6279, #25449, #22222, #15427, #35251, #38860, #5086, #35457, #11440, #38447, #34257, #41436, #9263, #41862, #35672, #28428, #12241, #19037, #12865, #18038, #29051, #37433, #27634, #22018, #30830, #40645, #9053, #32043, #31039, #2880, #15842, #28849, #12659, #25649, #19249, #24428, #21227, #32260, #42069, #2464, #9671, #22636, #17832, #109, #13072, #39711, #16895, #26063 ),
 .UNSPECIFIED., .F., .F.,
 ( 4, 2, 2, 2, 1, 2, 2, 1, 2, 2, 1, 2, 2, 2, 1, 2, 2, 2, 1, 2, 2, 2, 1, 1, 2, 2, 2, 2, 1, 1, 2, 2, 2, 2, 1, 1, 1, 2, 2, 2, 2, 2, 1, 1, 1, 1, 2, 2, 2, 2, 2, 1, 1, 1, 2, 2, 2, 2, 2, 1, 1, 1, 1, 1, 2, 2, 2, 1, 1, 1, 2, 2, 2, 1, 1, 1, 1, 1, 1, 2, 2, 2, 2, 2, 1, 1, 1, 1, 2, 2, 2, 1, 1, 1, 2, 2, 4 ),
 ( 0.000000000000000000, 0.001953125000004253542, 0.003906250000008507084, 0.005859375000012760626, 0.006835937500015010562, 0.007324218750016135530, 0.007812500000017260499, 0.008056640625017824284, 0.008178710937518268373, 0.008300781250018712462, 0.008544921875019602375, 0.008666992187520046464, 0.008789062500020490554, 0.009277343750020565147, 0.009521484375020599841, 0.009643554687520533922, 0.009765625000020466268, 0.01074218750001992677, 0.01123046875001975850, 0.01147460937501967523, 0.01171875000001959370, 0.01367187500001920859, 0.01464843750001911492, 0.01513671875001906982, 0.01538085937501904726, 0.01562500000001902645, 0.02343750000001785377, 0.02734375000001739581, 0.02929687500001716682, 0.03027343750001705233, 0.03076171875001698988, 0.03125000000001693090, 0.04687500000001662559, 0.05468750000001662559, 0.05859375000001661865, 0.06054687500001661171, 0.06152343750001676437, 0.06201171875001699335, 0.06250000000001720846, 0.09375000000002055300, 0.1093750000000222322, 0.1171875000000230649, 0.1210937500000234812, 0.1230468750000235784, 0.1240234375000235090, 0.1245117187500235922, 0.1247558593750236478, 0.1250000000000236755, 0.1875000000000396905, 0.2187500000000476563, 0.2343750000000518197, 0.2421875000000539568, 0.2460937500000550116, 0.2480468750000557054, 0.2490234375000561773, 0.2500000000000566769, 0.3750000000001075806, 0.4375000000001327827, 0.4687500000001454947, 0.4843750000001519895, 0.4921875000001553757, 0.4960937500001573186, 0.4980468750001585398, 0.4990234375001590394, 0.4995117187501594280, 0.5000000000001597611, 0.5625000000001978417, 0.5937500000002169376, 0.6093750000002263745, 0.6171875000002311484, 0.6210937500002333689, 0.6250000000002357003, 0.6875000000002793321, 0.7187500000003014256, 0.7343750000003125278, 0.7421875000003183009, 0.7460937500003208545, 0.7480468750003222977, 0.7490234375003230749, 0.7495117187503236300, 0.7500000000003242961, 0.8125000000002705614, 0.8437500000002434719, 0.8593750000002298162, 0.8671875000002228218, 0.8710937500002193801, 0.8730468750002178258, 0.8740234375002170486, 0.8745117187502164935, 0.8750000000002160494, 0.9062500000001612044, 0.9218750000001334488, 0.9296875000001197931, 0.9335937500001127987, 0.9355468750001096900, 0.9375000000001064704, 1.000000000000000000 ),
 .UNSPECIFIED. ) ;
#5712 = CARTESIAN_POINT ( 'NONE',  ( -5.639506490940112471, 64.42185452804264401, -1.523999999999993582 ) ) ;
#5713 = CARTESIAN_POINT ( 'NONE',  ( -57.93978974282668304, 0.6351742460125603396, 0.9371179993346451242 ) ) ;
#5714 = CARTESIAN_POINT ( 'NONE',  ( -8.594951744493888768, 74.76616009375631222, 1.524000000000002464 ) ) ;
#5715 = CARTESIAN_POINT ( 'NONE',  ( -5.638141748396392039, 57.15000000000040359, 5.060111600445807767 ) ) ;
#5716 = CARTESIAN_POINT ( 'NONE',  ( -6.439570805302779653E-14, 116.4254662015457313, -3.894619736530179447E-17 ) ) ;
#5717 = VERTEX_POINT ( 'NONE', #33105 ) ;
#5718 = CARTESIAN_POINT ( 'NONE',  ( -47.67648637180144533, 19.71513033058998232, 5.327979952964769339 ) ) ;
#5719 = CARTESIAN_POINT ( 'NONE',  ( -8.090109699362759699, 121.0242191076253988, -1.329746640891595888 ) ) ;
#5720 = CARTESIAN_POINT ( 'NONE',  ( -5.247413993112555630, 104.6144662015457385, -1.481417380683311968 ) ) ;
#5721 = AXIS2_PLACEMENT_3D ( 'NONE', #37398, #18417, #2266 ) ;
#5722 = CARTESIAN_POINT ( 'NONE',  ( 0.009747742627749139341, 156.3581291470199233, -0.4878169013068171522 ) ) ;
#5723 = CARTESIAN_POINT ( 'NONE',  ( -29.04966993600562830, 66.62533279660628693, 1.523999999999992916 ) ) ;
#5724 = DIRECTION ( 'NONE',  ( 1.011795553208986377E-16, 1.000000000000000000, -0.000000000000000000 ) ) ;
#5725 = VERTEX_POINT ( 'NONE', #3936 ) ;
#5726 = CARTESIAN_POINT ( 'NONE',  ( 4.585487687326599726, 17.13547844546973309, 0.5842699607688729424 ) ) ;
#5727 = CARTESIAN_POINT ( 'NONE',  ( -29.78720458926533965, 57.91457584465491948, 1.523999999999994026 ) ) ;
#5728 = CARTESIAN_POINT ( 'NONE',  ( -41.06680163122255323, 23.07855206975608553, -1.270000052244677269 ) ) ;
#5729 = FACE_OUTER_BOUND ( 'NONE', #34176, .T. ) ;
#5730 = AXIS2_PLACEMENT_3D ( 'NONE', #23695, #10301, #27331 ) ;
#5731 = DIRECTION ( 'NONE',  ( -0.8572391118119460085, -0.5149185422762189157, -3.573031421855289661E-16 ) ) ;
#5732 = CARTESIAN_POINT ( 'NONE',  ( -6.992768045718048775, 121.9460250970137594, -0.06266173978408597078 ) ) ;
#5733 = CARTESIAN_POINT ( 'NONE',  ( 5.332935392244917416, 115.7029491189645825, 0.1065647408284378928 ) ) ;
#5734 = CARTESIAN_POINT ( 'NONE',  ( 21.67644226493397142, 136.7703657609320658, 1.576579429902728036 ) ) ;
#5735 = CARTESIAN_POINT ( 'NONE',  ( -20.83467972660109524, 65.95194780259438971, -1.904999999999999583 ) ) ;
#5737 = CARTESIAN_POINT ( 'NONE',  ( 20.25200034474471522, 150.8812763393641490, -1.391365372170581649 ) ) ;
#5736 = CARTESIAN_POINT ( 'NONE',  ( 5.511339492712161281, 56.51499999999996504, 5.111277471823914453 ) ) ;
#5738 = CARTESIAN_POINT ( 'NONE',  ( -8.333011053690857040, 121.0263440914440736, 1.031464938890432226 ) ) ;
#5739 = CARTESIAN_POINT ( 'NONE',  ( -4.024516124431025688, 26.91537645720152128, -2.298571904627217499 ) ) ;
#5740 = CARTESIAN_POINT ( 'NONE',  ( -14.30760545270006290, 120.4308286971427862, -0.9551244717093422265 ) ) ;
#5741 = AXIS2_PLACEMENT_3D ( 'NONE', #24274, #8098, #17466 ) ;
#5742 = CARTESIAN_POINT ( 'NONE',  ( -0.5387148418522960114, 9.198764818822382949, 0.8109227438555447476 ) ) ;
#5743 = EDGE_LOOP ( 'NONE', ( #7863, #9841, #15969, #38792 ) ) ;
#5744 = CARTESIAN_POINT ( 'NONE',  ( -55.77633192430580777, 4.649224570933515821, 0.8844362032702561827 ) ) ;
#5745 = CARTESIAN_POINT ( 'NONE',  ( -10.62272853480731172, 153.0636280899912549, 0.4455235322555911037 ) ) ;
#5746 = CARTESIAN_POINT ( 'NONE',  ( 5.123467091704872800, -13.13098499675426112, 2.859697440480786668 ) ) ;
#5747 = CARTESIAN_POINT ( 'NONE',  ( 16.77814054344316474, 146.6545634508490821, -1.109899152166417213 ) ) ;
#5748 = EDGE_LOOP ( 'NONE', ( #2074, #21257 ) ) ;
#5749 = CARTESIAN_POINT ( 'NONE',  ( 3.234322848356350644, 115.7029687383090675, 1.652822622332805969 ) ) ;
#5750 = CARTESIAN_POINT ( 'NONE',  ( -4.745068207385612524, 117.6672791227833414, -1.125171127401668469 ) ) ;
#5751 = CARTESIAN_POINT ( 'NONE',  ( 0.6418402141071639644, 156.3034662015456888, -0.01455126635812856346 ) ) ;
#5752 = ORIENTED_EDGE ( 'NONE', *, *, #38896, .T. ) ;
#5753 = CARTESIAN_POINT ( 'NONE',  ( 12.56843540011181304, 155.2353133052689032, 2.219430909113760730 ) ) ;
#5754 = CARTESIAN_POINT ( 'NONE',  ( -14.73199999999999932, 12.96416000000000146, 0.000000000000000000 ) ) ;
#5755 = VECTOR ( 'NONE', #4383, 1000.000000000000000 ) ;
#5756 = CARTESIAN_POINT ( 'NONE',  ( 15.21351360038763012, 143.4186079242255119, 0.3040022078858786170 ) ) ;
#5757 = CARTESIAN_POINT ( 'NONE',  ( 4.958342374402591624, 117.4102150217221237, -0.9055978162701078249 ) ) ;
#5758 = CARTESIAN_POINT ( 'NONE',  ( 23.17968947452040851, 149.6103952014060212, 0.1325215592567121625 ) ) ;
#5759 = CARTESIAN_POINT ( 'NONE',  ( 0.08519874065564590759, 108.5751225745497948, -4.263693374914214296 ) ) ;
#5760 = CARTESIAN_POINT ( 'NONE',  ( -46.91715763656851124, 25.27325160652277347, 1.792044074526565778 ) ) ;
#5761 = CARTESIAN_POINT ( 'NONE',  ( -46.60530155212501313, 26.17382724835480445, 0.9172222222222133903 ) ) ;
#5762 = CARTESIAN_POINT ( 'NONE',  ( 1.647208221611285328, -15.32968734497926278, 5.596083536306344364 ) ) ;
#5763 = CARTESIAN_POINT ( 'NONE',  ( -43.83556092231052048, 21.45200552150719631, 2.811646013901242025 ) ) ;
#5764 = DIRECTION ( 'NONE',  ( 0.9998004120163609398, 0.000000000000000000, 0.01997839162482749689 ) ) ;
#5765 = CARTESIAN_POINT ( 'NONE',  ( -4.663774143481600021, 117.9610258373863019, 0.7407624695946702920 ) ) ;
#5766 = EDGE_LOOP ( 'NONE', ( #38103, #42066, #18579, #34671 ) ) ;
#5767 = CYLINDRICAL_SURFACE ( 'NONE', #41815, 0.2539999999999973390 ) ;
#5768 = CARTESIAN_POINT ( 'NONE',  ( -8.436567987665011259, 119.3310770286054492, -1.366807089744759285 ) ) ;
#5769 = CARTESIAN_POINT ( 'NONE',  ( -3.617430929662352135, 113.7286232773062125, -2.299356966923025158 ) ) ;
#5770 = CARTESIAN_POINT ( 'NONE',  ( 4.663391270879224670, 118.0052440920974277, 0.7715685123608813090 ) ) ;
#5771 = CARTESIAN_POINT ( 'NONE',  ( -46.60530155212503445, 26.17382724835477958, -1.524000000000008237 ) ) ;
#5772 = CARTESIAN_POINT ( 'NONE',  ( -0.3819982885359083369, 122.2435587914033022, 0.2867773152523558911 ) ) ;
#5773 = CARTESIAN_POINT ( 'NONE',  ( -4.288638401707804526, -7.253218809911426312, -1.756103832032595680 ) ) ;
#5774 = CARTESIAN_POINT ( 'NONE',  ( 4.931598085382976393, 117.4109156735239452, -0.9380226465277491377 ) ) ;
#5775 = LINE ( 'NONE', #31109, #26003 ) ;
#5776 = CARTESIAN_POINT ( 'NONE',  ( 5.416028590487108829, 119.2618716387835747, -0.3471801096392532759 ) ) ;
#5777 = CARTESIAN_POINT ( 'NONE',  ( -4.324763564747823530, 120.2039194668847699, -0.7996884002708144479 ) ) ;
#5778 = CARTESIAN_POINT ( 'NONE',  ( -5.153324091238889793, 56.51694919289756314, 4.640537933326888798 ) ) ;
#5779 = CARTESIAN_POINT ( 'NONE',  ( -6.016145911062735330, 28.73530235815178102, 1.153596677464569398 ) ) ;
#5780 = CARTESIAN_POINT ( 'NONE',  ( -2.146936912001416342, 115.7025561470850192, 1.628770542867131743 ) ) ;
#5781 = CARTESIAN_POINT ( 'NONE',  ( 4.458631606973747274, 16.91056413504885825, 1.251853190366734259 ) ) ;
#5783 = ORIENTED_EDGE ( 'NONE', *, *, #21007, .T. ) ;
#5782 = CARTESIAN_POINT ( 'NONE',  ( 8.168866085573474933, 117.6493956690293317, 0.5746791023534236764 ) ) ;
#5784 = CARTESIAN_POINT ( 'NONE',  ( 4.895073708310537342, 104.6144662015544640, -2.147637011550606267 ) ) ;
#5785 = CARTESIAN_POINT ( 'NONE',  ( 3.893829680932177517, -15.58178733528788129, 3.041689768969074503 ) ) ;
#5786 = CARTESIAN_POINT ( 'NONE',  ( -14.27152401005736415, 125.7140216354555804, 1.459898031787023598 ) ) ;
#5787 = CARTESIAN_POINT ( 'NONE',  ( -0.5888577047260095121, 18.69815917492401880, 0.7773729966010974879 ) ) ;
#5788 = CARTESIAN_POINT ( 'NONE',  ( 0.3244192847266222923, 10.43846528477952340, -0.9201954171864650256 ) ) ;
#5789 = ORIENTED_EDGE ( 'NONE', *, *, #19811, .F. ) ;
#5790 = ORIENTED_EDGE ( 'NONE', *, *, #21638, .T. ) ;
#5791 = CARTESIAN_POINT ( 'NONE',  ( -27.10368288468284348, 75.59070314479281194, 1.523999999999992916 ) ) ;
#5792 = CARTESIAN_POINT ( 'NONE',  ( 0.3635706870683514946, 106.2969274751293938, 5.168771910137537340 ) ) ;
#5793 =( NAMED_UNIT ( * ) PLANE_ANGLE_UNIT ( ) SI_UNIT ( $, .RADIAN. ) );
#5794 = CARTESIAN_POINT ( 'NONE',  ( -9.788763933237108361, 123.8372022493589100, 0.5907035020478677012 ) ) ;
#5795 = DIRECTION ( 'NONE',  ( 1.000000000000000000, 6.353134868986659519E-16, 0.000000000000000000 ) ) ;
#5796 = CARTESIAN_POINT ( 'NONE',  ( 3.015147157152042290, -12.41699557045261670, 0.4662733852003331791 ) ) ;
#5797 = CARTESIAN_POINT ( 'NONE',  ( 11.09075344257208684, 123.0430266451958232, -1.157373622111985467 ) ) ;
#5798 = CARTESIAN_POINT ( 'NONE',  ( -17.72814975036780183, 131.6735282812448986, -2.269257323068798460 ) ) ;
#5799 = CARTESIAN_POINT ( 'NONE',  ( 3.174366308151880922, 104.6144662015457243, 0.06343139340882769650 ) ) ;
#5800 = EDGE_CURVE ( 'NONE', #12982, #7108, #29898, .T. ) ;
#5801 = CARTESIAN_POINT ( 'NONE',  ( 7.963027852037909859, 121.6653397483754020, 1.110511108043854778 ) ) ;
#5802 = CARTESIAN_POINT ( 'NONE',  ( -0.01691503824241830795, 39.20946620154573026, 0.8464976821738520174 ) ) ;
#5803 = CARTESIAN_POINT ( 'NONE',  ( 9.357997026032778720, 124.2740283646700306, -0.04730198213477312952 ) ) ;
#5804 = VERTEX_POINT ( 'NONE', #40755 ) ;
#5805 = CARTESIAN_POINT ( 'NONE',  ( -2.372405652431340606, 106.9230564690743819, -4.772463516138556905 ) ) ;
#5806 = DIRECTION ( 'NONE',  ( 0.3256999990547876367, 0.9454731675810326141, 8.328397965208553695E-18 ) ) ;
#5807 = DIRECTION ( 'NONE',  ( 0.1469470846586743706, 0.000000000000000000, 0.9891443546370348727 ) ) ;
#5808 = CARTESIAN_POINT ( 'NONE',  ( -58.60951264191312049, -0.2527965749330313150, 0.4344104473664969213 ) ) ;
#5809 = ADVANCED_FACE ( 'NONE', ( #33526 ), #41774, .T. ) ;
#5810 = CARTESIAN_POINT ( 'NONE',  ( 1.466575460758787530, 20.86946789039323491, 8.308456332865098659 ) ) ;
#5811 = CARTESIAN_POINT ( 'NONE',  ( 10.07755082079036235, 123.5826510519420509, 1.213607387526569381 ) ) ;
#5812 = DIRECTION ( 'NONE',  ( -4.017660918040594346E-17, 1.000000000000000000, 2.376309959284834438E-19 ) ) ;
#5813 = CARTESIAN_POINT ( 'NONE',  ( 21.90617686096470251, 151.4314113202728436, 0.4124301881307766982 ) ) ;
#5814 = CARTESIAN_POINT ( 'NONE',  ( -0.3637657132513893443, 105.8833743670705445, 5.328194401858565854 ) ) ;
#5815 = CARTESIAN_POINT ( 'NONE',  ( 4.349802767100347189, -10.92635770930747796, -1.576909098649299512 ) ) ;
#5816 = CARTESIAN_POINT ( 'NONE',  ( 4.218275339060157059, 155.8585684991085714, 0.08429118021179421438 ) ) ;
#5817 = AXIS2_PLACEMENT_3D ( 'NONE', #2743, #19107, #29118 ) ;
#5818 = CARTESIAN_POINT ( 'NONE',  ( 4.267473507877284078, -4.198009126799147062, -7.300781474974544771 ) ) ;
#5819 = CARTESIAN_POINT ( 'NONE',  ( 5.516891121731406500, 117.1192735582419004, -0.5335394950436042061 ) ) ;
#5820 = CARTESIAN_POINT ( 'NONE',  ( -0.4232488410869896800, 124.9344662015457317, -0.008457519121176893320 ) ) ;
#5821 = CARTESIAN_POINT ( 'NONE',  ( 4.854633716284418199, 115.7029491485453150, -1.279498648767042557 ) ) ;
#5822 = CARTESIAN_POINT ( 'NONE',  ( -6.573280687130626123E-14, 88.99346620154574339, 1.699031322814114629E-29 ) ) ;
#5823 = CARTESIAN_POINT ( 'NONE',  ( 7.741462187161934239, -10.92447321953606654, -3.338652055795839679 ) ) ;
#5824 = CARTESIAN_POINT ( 'NONE',  ( 0.3314860322431096296, 118.1588881126417050, 0.9092559162175757326 ) ) ;
#5825 = CARTESIAN_POINT ( 'NONE',  ( -10.39456080247343905, 81.94606122948148652, 1.524000000000000465 ) ) ;
#5826 = LINE ( 'NONE', #27750, #18847 ) ;
#5827 = EDGE_CURVE ( 'NONE', #6380, #30889, #15223, .T. ) ;
#5828 = CARTESIAN_POINT ( 'NONE',  ( 0.6471768874970514895, 112.6282971158091470, -2.732684515117583590 ) ) ;
#5829 = CARTESIAN_POINT ( 'NONE',  ( -22.91960207526971871, 149.8162411397050278, 0.2683370967508547644 ) ) ;
#5830 = ORIENTED_EDGE ( 'NONE', *, *, #2746, .T. ) ;
#5831 = CARTESIAN_POINT ( 'NONE',  ( -58.46425016648313999, 0.8496528882456222398, -0.7404953295986963502 ) ) ;
#5832 = EDGE_CURVE ( 'NONE', #3703, #276, #32095, .T. ) ;
#5833 = ORIENTED_EDGE ( 'NONE', *, *, #13123, .F. ) ;
#5834 = CARTESIAN_POINT ( 'NONE',  ( -43.11180532272962296, 21.58876176643009615, -2.074236749942713232 ) ) ;
#5835 = CARTESIAN_POINT ( 'NONE',  ( -15.77337136323457578, 146.5674407247335864, -0.1809852566079092895 ) ) ;
#5836 = CARTESIAN_POINT ( 'NONE',  ( 4.513795256570364067, -15.26848473984131260, 4.551867270201407578 ) ) ;
#5837 = CARTESIAN_POINT ( 'NONE',  ( -5.883382875664681322, 118.7305451321402501, 0.9239882381799517930 ) ) ;
#5838 = EDGE_CURVE ( 'NONE', #26546, #20056, #8427, .T. ) ;
#5839 = CARTESIAN_POINT ( 'NONE',  ( 14.39601482975355040, 155.9958976045614349, -1.017949466214369325 ) ) ;
#5840 = CARTESIAN_POINT ( 'NONE',  ( 3.345514242732226418, 6.565394131763864216, 3.211428121085859733 ) ) ;
#5841 = CARTESIAN_POINT ( 'NONE',  ( -1.872007501980990085, 116.6503132507590124, -0.2654151457657343283 ) ) ;
#5842 = CARTESIAN_POINT ( 'NONE',  ( -55.34422897054474788, 6.609666497766444770, -3.132814435880084680 ) ) ;
#5843 = ORIENTED_EDGE ( 'NONE', *, *, #38086, .F. ) ;
#5844 = CARTESIAN_POINT ( 'NONE',  ( -0.01046636459302786523, 120.7331730230139755, 0.5237796829255390030 ) ) ;
#5845 = DIRECTION ( 'NONE',  ( 4.017660918040594346E-17, -1.000000000000000000, -2.376309959284834438E-19 ) ) ;
#5846 = CARTESIAN_POINT ( 'NONE',  ( -0.008945177888008831735, 119.9096241394016715, 0.4476532798976762817 ) ) ;
#5847 = DIRECTION ( 'NONE',  ( -5.188838149069472160E-16, 1.699382548006136559E-16, 1.000000000000000000 ) ) ;
#5848 = CARTESIAN_POINT ( 'NONE',  ( 11.27019207447471416, 122.4230570912197038, -1.244363564371071540 ) ) ;
#5849 = CARTESIAN_POINT ( 'NONE',  ( -21.29267830536757700, 148.0064520001644723, -2.314741142932118301 ) ) ;
#5850 = CARTESIAN_POINT ( 'NONE',  ( -51.58367816905025194, 14.91232437457545146, -4.609044670965841917 ) ) ;
#5851 = CARTESIAN_POINT ( 'NONE',  ( 9.279111390949699611, 123.6186430441458981, -0.4039598099628549099 ) ) ;
#5852 = CIRCLE ( 'NONE', #39957, 3.683000000000001162 ) ;
#5853 = ORIENTED_EDGE ( 'NONE', *, *, #27124, .F. ) ;
#5854 = CARTESIAN_POINT ( 'NONE',  ( -11.03566430468816328, 123.0430266451958232, -1.599512106649902288 ) ) ;
#5855 = CARTESIAN_POINT ( 'NONE',  ( 2.813987013336220144, -15.51818976969260255, 4.585835125202748053 ) ) ;
#5856 = CARTESIAN_POINT ( 'NONE',  ( -4.106443892462531942, 118.2429491485453070, -0.3519330368941736564 ) ) ;
#5857 = CARTESIAN_POINT ( 'NONE',  ( -58.60752282809816904, -0.1920500713008393978, -0.6598870774482961110 ) ) ;
#5858 = CARTESIAN_POINT ( 'NONE',  ( -4.887531664472737347, 117.7483860691352646, 0.7386977146963198404 ) ) ;
#5859 = CARTESIAN_POINT ( 'NONE',  ( 17.73873607445671041, 146.7645792007554633, 2.242890973037755753 ) ) ;
#5860 = DIRECTION ( 'NONE',  ( 0.000000000000000000, 1.000000000000000000, 0.000000000000000000 ) ) ;
#5861 = CARTESIAN_POINT ( 'NONE',  ( -7.781828003681788175, 2.241565531857627303, -3.240848859074576094 ) ) ;
#5862 = CARTESIAN_POINT ( 'NONE',  ( 13.02783148976608807, 133.9378623523624299, 0.5757418746946232346 ) ) ;
#5863 = DIRECTION ( 'NONE',  ( 0.6559537821943239866, -0.7548010569845283735, 4.686333752532408853E-16 ) ) ;
#5865 = EDGE_CURVE ( 'NONE', #10936, #33761, #11552, .T. ) ;
#5864 = CARTESIAN_POINT ( 'NONE',  ( -47.69647088358534148, 18.57426963660985209, -3.960430087866680271 ) ) ;
#5866 = CARTESIAN_POINT ( 'NONE',  ( -0.8541570955536235132, 117.3993835805775490, 1.452923500009727809 ) ) ;
#5867 = CARTESIAN_POINT ( 'NONE',  ( -58.43690671596436914, -0.4125963578781866037, 0.2423173958219003998 ) ) ;
#5868 = CARTESIAN_POINT ( 'NONE',  ( -53.84250820861786480, 9.549132715125418613, 3.786023059759871412 ) ) ;
#5869 = CYLINDRICAL_SURFACE ( 'NONE', #6629, 0.5080000000000000071 ) ;
#5870 = CARTESIAN_POINT ( 'NONE',  ( -6.059261036834497460, 88.73331249999999670, -5.016499999999999737 ) ) ;
#5871 = CARTESIAN_POINT ( 'NONE',  ( -52.70911355518960306, 14.14937146821753444, 3.349573991549116059 ) ) ;
#5872 = CARTESIAN_POINT ( 'NONE',  ( -23.34154082800050745, 148.8574307740229585, -0.2355990431193896728 ) ) ;
#5873 = VERTEX_POINT ( 'NONE', #40133 ) ;
#5874 = CARTESIAN_POINT ( 'NONE',  ( -49.10997966587441965, 20.64911895071488956, -3.108984601230539990 ) ) ;
#5875 = CARTESIAN_POINT ( 'NONE',  ( -7.802523906719404323, 122.5105737818149407, -0.4685457770883232897 ) ) ;
#5876 = ADVANCED_FACE ( 'NONE', ( #4777 ), #12497, .T. ) ;
#5877 = CARTESIAN_POINT ( 'NONE',  ( 5.008145594203718076, 117.3993868333640478, -0.7758522469519856246 ) ) ;
#5878 = ORIENTED_EDGE ( 'NONE', *, *, #36551, .F. ) ;
#5879 = CARTESIAN_POINT ( 'NONE',  ( 1.799517872912148819, 115.7029357459833818, -1.654564060799146752 ) ) ;
#5880 = CARTESIAN_POINT ( 'NONE',  ( -15.78121303607992942, 145.9231181611787918, -0.5460855120906793481 ) ) ;
#5881 = CARTESIAN_POINT ( 'NONE',  ( 5.728675787863017455, -12.92793046001887447, 1.911514839944304045 ) ) ;
#5882 = CARTESIAN_POINT ( 'NONE',  ( -0.009931510163747995362, 117.7854482299006378, 0.4970133802592051064 ) ) ;
#5883 = CARTESIAN_POINT ( 'NONE',  ( -5.151949832170181764, 116.8361703259256217, -0.1799158315879852421 ) ) ;
#5884 = CARTESIAN_POINT ( 'NONE',  ( 22.51303867192105912, 150.7865899205276321, 0.6781733187083919256 ) ) ;
#5885 = ADVANCED_FACE ( 'NONE', ( #39641 ), #1089, .T. ) ;
#5886 = CARTESIAN_POINT ( 'NONE',  ( 5.942184298922027708, 155.4082271737278234, 0.2231331471019911694 ) ) ;
#5887 = CARTESIAN_POINT ( 'NONE',  ( -36.65473259702431363, 28.27472347546386544, -1.524000000000003574 ) ) ;
#5888 = CARTESIAN_POINT ( 'NONE',  ( -0.9756160567605162148, 3.744600508531710226, -0.009113680661486545098 ) ) ;
#5889 = CARTESIAN_POINT ( 'NONE',  ( -15.18737561846517892, 156.0999766016731769, -0.3708822620858232555 ) ) ;
#5890 = FACE_OUTER_BOUND ( 'NONE', #28904, .T. ) ;
#5891 = CARTESIAN_POINT ( 'NONE',  ( -3.682264917456322895, 66.13346620154572975, -0.07358041635423968885 ) ) ;
#5892 = ORIENTED_EDGE ( 'NONE', *, *, #10812, .F. ) ;
#5893 = CARTESIAN_POINT ( 'NONE',  ( 5.529506464480028249, 117.0650090453692798, 0.6737858539469722130 ) ) ;
#5894 = DIRECTION ( 'NONE',  ( -3.035386659626960118E-16, 0.000000000000000000, -1.000000000000000000 ) ) ;
#5895 = CARTESIAN_POINT ( 'NONE',  ( 21.09420047167885315, 149.7512365312068709, 2.228874019815534346 ) ) ;
#5896 = CARTESIAN_POINT ( 'NONE',  ( 7.699499347746429301, 119.6133147451300971, -1.075113282820071570 ) ) ;
#5897 = CARTESIAN_POINT ( 'NONE',  ( 1.285294229880325600, 5.975470260049262627, -8.359553334813638159 ) ) ;
#5898 = EDGE_CURVE ( 'NONE', #28135, #8589, #36447, .T. ) ;
#5899 = CARTESIAN_POINT ( 'NONE',  ( -21.19929070476258204, 136.5942649496780632, -1.819607900871525574 ) ) ;
#5900 = CARTESIAN_POINT ( 'NONE',  ( 4.712039816507104462, 117.8377826564535980, -0.8492390109202567761 ) ) ;
#5901 = CARTESIAN_POINT ( 'NONE',  ( 6.914225208283751201, 121.8192184429722005, 0.2944576502256240347 ) ) ;
#5902 = CARTESIAN_POINT ( 'NONE',  ( -7.800806202325043515, 154.6345575486818404, -0.04849676858278722386 ) ) ;
#5903 = CARTESIAN_POINT ( 'NONE',  ( -18.80567741551218930, 148.1672603684278329, -2.476295349149460367 ) ) ;
#5904 = CARTESIAN_POINT ( 'NONE',  ( 3.388119949408427978, -15.58183483456807039, 5.324763925812813881 ) ) ;
#5905 = CARTESIAN_POINT ( 'NONE',  ( 4.726842832297071695, 118.5931160184169073, 1.020482801973786380 ) ) ;
#5906 = VECTOR ( 'NONE', #37668, 1000.000000000000114 ) ;
#5907 = CARTESIAN_POINT ( 'NONE',  ( -1.960935811749206170, 117.3993839180219254, -1.450040409155178622 ) ) ;
#5909 = EDGE_LOOP ( 'NONE', ( #36788, #29258, #23926, #22409 ) ) ;
#5908 = AXIS2_PLACEMENT_3D ( 'NONE', #22731, #28933, #13386 ) ;
#5910 = CARTESIAN_POINT ( 'NONE',  ( 9.495519422240706220, 121.2752502669211339, 1.536911970732435684 ) ) ;
#5911 = CARTESIAN_POINT ( 'NONE',  ( -17.14500000000000313, 71.11999999999999034, -5.714999999999998970 ) ) ;
#5912 = CARTESIAN_POINT ( 'NONE',  ( -46.38316532014830784, 26.05065462784526176, -1.524000000000014676 ) ) ;
#5913 = CARTESIAN_POINT ( 'NONE',  ( -1.341555883842942887, 107.4826764677166864, 4.621745984720207368 ) ) ;
#5914 = CARTESIAN_POINT ( 'NONE',  ( -8.308456333890557488, -0.7205321100333081930, 1.466575456822119206 ) ) ;
#5915 = CARTESIAN_POINT ( 'NONE',  ( 9.680894551640095713, 124.1466939447965814, 0.8054060769509039375 ) ) ;
#5916 = CARTESIAN_POINT ( 'NONE',  ( 10.53014098995821435, 157.9057380314836223, -0.5653498989572928179 ) ) ;
#5917 = CARTESIAN_POINT ( 'NONE',  ( 5.450166374333662134, 56.51500000000003610, -4.451212169035211552 ) ) ;
#5919 = VECTOR ( 'NONE', #8561, 1000.000000000000000 ) ;
#5918 = CARTESIAN_POINT ( 'NONE',  ( -58.36373456865217690, -0.2788725735744660983, 0.09695730896412824151 ) ) ;
#5920 = CARTESIAN_POINT ( 'NONE',  ( -6.552838421881942555E-14, 85.18346620154574111, 1.207165459533130484E-19 ) ) ;
#5921 = CARTESIAN_POINT ( 'NONE',  ( -23.14542444889682571, 82.37908244650444090, -1.524000000000005794 ) ) ;
#5922 = CARTESIAN_POINT ( 'NONE',  ( -22.53527615164633602, 150.7831677823008363, -0.4503084484864735004 ) ) ;
#5923 = ORIENTED_EDGE ( 'NONE', *, *, #8940, .T. ) ;
#5924 = CARTESIAN_POINT ( 'NONE',  ( -8.204323950348388905, 120.4574377990110463, -1.430383891062076085 ) ) ;
#5925 = DIRECTION ( 'NONE',  ( -1.000000000000000000, 0.000000000000000000, 0.000000000000000000 ) ) ;
#5926 = CIRCLE ( 'NONE', #23587, 0.2540000000000000036 ) ;
#5927 = CARTESIAN_POINT ( 'NONE',  ( -7.064669522240172306, 121.9740017686541194, -0.4795729057185782462 ) ) ;
#5928 = CARTESIAN_POINT ( 'NONE',  ( -41.23752580366542020, 23.26788267949596190, 1.523999999999992916 ) ) ;
#5929 = CARTESIAN_POINT ( 'NONE',  ( 11.73662545640870114, 118.7267541726749869, 0.2503127652027327121 ) ) ;
#5930 = EDGE_CURVE ( 'NONE', #17444, #16646, #7072, .T. ) ;
#5931 = VERTEX_POINT ( 'NONE', #10023 ) ;
#5932 = CARTESIAN_POINT ( 'NONE',  ( 3.121479725567877228, 16.06095178295013071, 3.416230322513892137 ) ) ;
#5933 = CARTESIAN_POINT ( 'NONE',  ( -5.041288869262119832, 105.1216794573741282, 1.777295568394765546 ) ) ;
#5934 = CARTESIAN_POINT ( 'NONE',  ( -6.426369768295692736E-14, 159.6054662015457382, 1.032716915552223178E-16 ) ) ;
#5935 = LINE ( 'NONE', #8906, #34673 ) ;
#5936 = AXIS2_PLACEMENT_3D ( 'NONE', #23220, #36886, #14072 ) ;
#5937 = CARTESIAN_POINT ( 'NONE',  ( -6.401666570281891566, 64.12941061790216679, 1.270000000000005125 ) ) ;
#5938 = CARTESIAN_POINT ( 'NONE',  ( -6.068594780648083997, 121.4118082408263746, 0.08813677267068076304 ) ) ;
#5939 = ADVANCED_FACE ( 'NONE', ( #17040 ), #7686, .F. ) ;
#5940 = CARTESIAN_POINT ( 'NONE',  ( -2.131885088311801901, 26.04095958170969638, -4.099730575217565232 ) ) ;
#5941 = CARTESIAN_POINT ( 'NONE',  ( 21.30289582938779702, 151.2846570542378117, 1.588627997894106247 ) ) ;
#5942 = CARTESIAN_POINT ( 'NONE',  ( 2.602530512026160370, 104.6144662015457243, -4.073939027099183541 ) ) ;
#5944 = CARTESIAN_POINT ( 'NONE',  ( 7.150008447151647850, 158.1912585135832785, -1.373277972272069380 ) ) ;
#5943 = CARTESIAN_POINT ( 'NONE',  ( -0.1058213901579529159, 105.9761915687834914, 5.295735085524055030 ) ) ;
#5945 = CARTESIAN_POINT ( 'NONE',  ( -9.808453647370097173, 155.3230018269108825, 1.667681936676748133 ) ) ;
#5946 = CARTESIAN_POINT ( 'NONE',  ( 0.7725151586569730666, -15.29989167607388900, -0.5872501270430795506 ) ) ;
#5947 = CARTESIAN_POINT ( 'NONE',  ( -16.43260349481045424, 122.7513851185756693, -1.135385547233646042 ) ) ;
#5948 = EDGE_LOOP ( 'NONE', ( #15129, #15605, #31191, #32905 ) ) ;
#5949 = CARTESIAN_POINT ( 'NONE',  ( -57.26476250566310711, 1.946856395439316989, 1.045107959733424074 ) ) ;
#5950 = CARTESIAN_POINT ( 'NONE',  ( -12.26386414673838843, 130.6044139104978115, 0.2969705276545481776 ) ) ;
#5951 = CARTESIAN_POINT ( 'NONE',  ( 3.928490385995774936, -14.72231570353084429, 5.141255514400237203 ) ) ;
#5952 = CARTESIAN_POINT ( 'NONE',  ( 10.67172107669495418, 123.8807653058400575, -0.9292482510779808136 ) ) ;
#5953 = DIRECTION ( 'NONE',  ( -5.206863593109713661E-17, 1.000000000000000000, -1.077750396879097183E-30 ) ) ;
#5954 = AXIS2_PLACEMENT_3D ( 'NONE', #8859, #15448, #35271 ) ;
#5955 = CARTESIAN_POINT ( 'NONE',  ( -4.676071978438741894, 117.9791466300892750, -0.8444188316661053184 ) ) ;
#5956 = CARTESIAN_POINT ( 'NONE',  ( 15.21929369751753924, 143.4245298570049840, 0.2523546585945008469 ) ) ;
#5957 = ORIENTED_EDGE ( 'NONE', *, *, #39249, .F. ) ;
#5958 = CARTESIAN_POINT ( 'NONE',  ( 20.02396230387740772, 148.3334041379468715, 2.502640320863741774 ) ) ;
#5959 = DIRECTION ( 'NONE',  ( 0.9998501190848635423, 0.01731298258488073519, 5.158639060800513087E-16 ) ) ;
#5960 = CARTESIAN_POINT ( 'NONE',  ( 18.32410244842765934, 8.844871939465424049, 2.244055341071511024E-15 ) ) ;
#5961 = CARTESIAN_POINT ( 'NONE',  ( 5.002599301907898699, 117.4023545182666055, -0.8031422281648238348 ) ) ;
#5962 = AXIS2_PLACEMENT_3D ( 'NONE', #8377, #21342, #6242 ) ;
#5963 = CARTESIAN_POINT ( 'NONE',  ( 0.3151558924358287550, 116.5752054743899038, -0.1523977429619429169 ) ) ;
#5964 = CARTESIAN_POINT ( 'NONE',  ( -15.36699999999999378, 12.96302561210691984, 0.000000000000000000 ) ) ;
#5965 = CARTESIAN_POINT ( 'NONE',  ( -46.83932897938335316, 25.61700229504076631, 1.554731942900158259 ) ) ;
#5966 = CARTESIAN_POINT ( 'NONE',  ( -46.67361288142431164, 26.04169289900193363, 0.9171659260646253253 ) ) ;
#5967 = CARTESIAN_POINT ( 'NONE',  ( 1.694057231424134446, -15.22899506564825955, 5.771026123934793972 ) ) ;
#5968 = CARTESIAN_POINT ( 'NONE',  ( -48.21404017327530767, 19.06235592689615288, 5.351320745402585288 ) ) ;
#5969 = CARTESIAN_POINT ( 'NONE',  ( -4.665613787933919454, 118.0266005560186358, 0.5747475622275362017 ) ) ;
#5970 = VERTEX_POINT ( 'NONE', #13227 ) ;
#5971 = ORIENTED_EDGE ( 'NONE', *, *, #29037, .F. ) ;
#5972 = CARTESIAN_POINT ( 'NONE',  ( 14.73199999999999754, 61.59499999999999886, 5.016499999999999737 ) ) ;
#5973 = CARTESIAN_POINT ( 'NONE',  ( -5.958530970433706386, 119.2302670178880817, -1.266206984860304585 ) ) ;
#5974 = CARTESIAN_POINT ( 'NONE',  ( -3.948369173669738608, 116.4303826247378026, -1.336099082351541956 ) ) ;
#5975 = CARTESIAN_POINT ( 'NONE',  ( 4.772709941698821901, 117.8804716543160112, 0.8736280956481000670 ) ) ;
#5976 = CARTESIAN_POINT ( 'NONE',  ( 3.205191379615736746, -14.47393913169138102, 3.051678166811226500 ) ) ;
#5977 = CARTESIAN_POINT ( 'NONE',  ( -10.42685857375371050, 124.8149993102252182, -1.042337215157124186 ) ) ;
#5978 = CIRCLE ( 'NONE', #22269, 0.5079999999999997851 ) ;
#5979 = CARTESIAN_POINT ( 'NONE',  ( -2.983771112188844832, -5.329111280313512999, 3.548611825089460048 ) ) ;
#5980 = CARTESIAN_POINT ( 'NONE',  ( -1.958751975754273289, 106.7073577057565643, 4.892300404344175568 ) ) ;
#5981 = CARTESIAN_POINT ( 'NONE',  ( -5.591535794131393899, 65.03215273817657760, 1.524000000000005572 ) ) ;
#5982 = CARTESIAN_POINT ( 'NONE',  ( 5.578601203221819738, 117.9513286348681476, -0.5234822864975615664 ) ) ;
#5983 = CARTESIAN_POINT ( 'NONE',  ( -10.91091678335021342, 123.4376579628654014, -1.516229561143084492 ) ) ;
#5984 = CARTESIAN_POINT ( 'NONE',  ( 16.31694223957253698, 121.4173703750124531, 0.3260513381110077824 ) ) ;
#5985 = CARTESIAN_POINT ( 'NONE',  ( -3.991072007095600949, 33.40439263831326855, 3.842775004540742501 ) ) ;
#5986 = CARTESIAN_POINT ( 'NONE',  ( -4.589169710308834915, 115.7029491485453434, 1.333228958008984888 ) ) ;
#5987 = CARTESIAN_POINT ( 'NONE',  ( -1.178223178616622402, 14.53665720681882689, 4.476207649055042204 ) ) ;
#5989 = ORIENTED_EDGE ( 'NONE', *, *, #23477, .F. ) ;
#5988 = CARTESIAN_POINT ( 'NONE',  ( 23.25105004451259916, 146.7258352529021863, 1.066525923017375810 ) ) ;
#5990 = CARTESIAN_POINT ( 'NONE',  ( 2.045048008636439540, 104.6144662015458096, -4.372098095898148351 ) ) ;
#5991 = CARTESIAN_POINT ( 'NONE',  ( 3.879565938682602244, -15.27118588775909558, 0.8622231344456012803 ) ) ;
#5992 = CARTESIAN_POINT ( 'NONE',  ( -3.289525010481907596, 118.9727644790723531, 0.7721065173366226109 ) ) ;
#5993 = CARTESIAN_POINT ( 'NONE',  ( -0.5956917769015268593, 15.89737491555829685, -0.7703063551142234067 ) ) ;
#5994 = B_SPLINE_CURVE_WITH_KNOTS ( 'NONE', 3,
 ( #6052, #32650, #18802, #19014, #38633, #35645, #291, #22822, #19434, #6255 ),
 .UNSPECIFIED., .F., .F.,
 ( 4, 2, 2, 2, 4 ),
 ( 0.000000000000000000, 0.0001138296224026695075, 0.0002276592448053389066, 0.0004553184896106773254, 0.0009106369792213540003 ),
 .UNSPECIFIED. ) ;
#5995 = CARTESIAN_POINT ( 'NONE',  ( 0.5139362334885246852, 0.5165572279304807557, -0.8313783143454911428 ) ) ;
#5996 = VERTEX_POINT ( 'NONE', #22994 ) ;
#5997 = ORIENTED_EDGE ( 'NONE', *, *, #14599, .T. ) ;
#5998 = CARTESIAN_POINT ( 'NONE',  ( -13.46199999999999442, 12.17394877578617063, 1.841354584184931751E-15 ) ) ;
#5999 = CARTESIAN_POINT ( 'NONE',  ( 1.025137579952656308, 106.6134986179334589, 5.027802332087124348 ) ) ;
#6000 = CARTESIAN_POINT ( 'NONE',  ( -0.4838554169687688811, 0.1183881754249058588, 4.002417470467119770E-14 ) ) ;
#6001 = CARTESIAN_POINT ( 'NONE',  ( -9.877746432283343481, 123.9483309312939099, 0.5948279539607077560 ) ) ;
#6002 = CARTESIAN_POINT ( 'NONE',  ( -9.538359384048678891, 124.8019839352694476, -0.1905991205270209377 ) ) ;
#6003 = CARTESIAN_POINT ( 'NONE',  ( 2.740927916200229131, -14.67636064986481337, 4.771625012207401539 ) ) ;
#6004 = CARTESIAN_POINT ( 'NONE',  ( 17.52489820599659254, 148.6234142586927476, -1.577473031907404621 ) ) ;
#6005 = CARTESIAN_POINT ( 'NONE',  ( -17.05522983032417628, 131.5760549582342094, -2.311017189013932160 ) ) ;
#6006 = DIRECTION ( 'NONE',  ( 0.9998004120163610509, 4.016384292689131511E-17, 0.01997839162482749689 ) ) ;
#6007 = CARTESIAN_POINT ( 'NONE',  ( 8.788213500272473055, 117.7098710386940894, 0.3783554591865261885 ) ) ;
#6008 = CARTESIAN_POINT ( 'NONE',  ( 4.074910602682932925, 118.2429491485453354, -0.1454311599470142491 ) ) ;
#6009 = CARTESIAN_POINT ( 'NONE',  ( 15.68661553393314456, 147.2319784351455780, -0.01612984191841659518 ) ) ;
#6010 = ORIENTED_EDGE ( 'NONE', *, *, #20468, .F. ) ;
#6011 = CARTESIAN_POINT ( 'NONE',  ( 2.666490510518176649, -13.49855353256042889, 0.05227394649444832425 ) ) ;
#6012 = CARTESIAN_POINT ( 'NONE',  ( 5.586884702347362897, 123.6644662015457214, 0.1116392523995368424 ) ) ;
#6013 = CARTESIAN_POINT ( 'NONE',  ( 2.928799644063047936, 38.81416391459460158, 1.351591292951386469 ) ) ;
#6014 = STYLED_ITEM ( 'NONE', ( #11741 ), #21408 ) ;
#6015 = FACE_OUTER_BOUND ( 'NONE', #12670, .T. ) ;
#6016 = CARTESIAN_POINT ( 'NONE',  ( -6.293633234193186432, 17.08131519529194975, -5.670988759835773330 ) ) ;
#6017 = CARTESIAN_POINT ( 'NONE',  ( 14.37089176232986354, 134.5679602169015254, 1.683180344383908400 ) ) ;
#6018 = CARTESIAN_POINT ( 'NONE',  ( -5.451267667241070720E-14, 85.80437499999999318, 0.000000000000000000 ) ) ;
#6019 = CARTESIAN_POINT ( 'NONE',  ( 5.781358041568656070, 116.9360814311326777, 0.07286664083783171708 ) ) ;
#6020 = ADVANCED_FACE ( 'NONE', ( #36021 ), #881, .T. ) ;
#6021 = CARTESIAN_POINT ( 'NONE',  ( -4.473299935328737931, 111.2795884869231173, 2.951234740152492986 ) ) ;
#6022 = CARTESIAN_POINT ( 'NONE',  ( -0.2095918955067871126, -8.989892990265463624, -4.636818132431064221 ) ) ;
#6023 = CARTESIAN_POINT ( 'NONE',  ( 1.561582345843624431, 156.2588034088681184, 0.03120413162939523685 ) ) ;
#6024 = B_SPLINE_CURVE_WITH_KNOTS ( 'NONE', 3,
 ( #41497, #8485, #37866, #21652, #15274, #25078 ),
 .UNSPECIFIED., .F., .F.,
 ( 4, 2, 4 ),
 ( 0.000000000000000000, 0.5000000000000000000, 1.000000000000000000 ),
 .UNSPECIFIED. ) ;
#6025 = CARTESIAN_POINT ( 'NONE',  ( 15.86975487621997871, 125.3951846505478329, 1.921535798876653711 ) ) ;
#6026 = CARTESIAN_POINT ( 'NONE',  ( 4.673167956146812685, 25.32871407960522347, 7.020956665532097851 ) ) ;
#6027 = CARTESIAN_POINT ( 'NONE',  ( -5.476986130384075224, 117.4239406935068786, -0.9134031189204426804 ) ) ;
#6028 = CARTESIAN_POINT ( 'NONE',  ( -0.2094794444023877211, 111.5577547982948801, -3.149697633913104422 ) ) ;
#6029 = CARTESIAN_POINT ( 'NONE',  ( -22.98488057257204886, 150.1591296352320910, -0.4592926148156235011 ) ) ;
#6030 = DIRECTION ( 'NONE',  ( -5.188838149069471174E-16, 1.699382548006136313E-16, 1.000000000000000000 ) ) ;
#6031 = CARTESIAN_POINT ( 'NONE',  ( -2.768688662514669385, 30.30441277318858795, -3.700580903672975541 ) ) ;
#6032 = CARTESIAN_POINT ( 'NONE',  ( 3.117173950248831815, 118.1588878836352166, 0.8040983753412327406 ) ) ;
#6033 = CARTESIAN_POINT ( 'NONE',  ( -41.25198653392084935, 23.25239942703034046, 1.523999999999994248 ) ) ;
#6034 = CARTESIAN_POINT ( 'NONE',  ( 2.234143439902941175, -15.10063862499563747, 5.099642030148213934 ) ) ;
#6035 = EDGE_CURVE ( 'NONE', #15131, #15945, #25434, .T. ) ;
#6036 = CARTESIAN_POINT ( 'NONE',  ( 0.7761819157717084749, 120.0979018405971175, -0.5779541898223675700 ) ) ;
#6037 = CARTESIAN_POINT ( 'NONE',  ( -22.39781672572324567, 150.5530013069706285, 0.3987920954333213919 ) ) ;
#6038 = VERTEX_POINT ( 'NONE', #7727 ) ;
#6039 = CARTESIAN_POINT ( 'NONE',  ( -3.682264917456323339, 78.83346620154574680, -0.07358041635423968885 ) ) ;
#6040 = ORIENTED_EDGE ( 'NONE', *, *, #20631, .T. ) ;
#6041 = CARTESIAN_POINT ( 'NONE',  ( -41.77909418348673398, 22.73884196981018491, -1.565812447105877192 ) ) ;
#6042 = CARTESIAN_POINT ( 'NONE',  ( 4.894061823620152296, -15.42295773938226411, 3.608731902971048733 ) ) ;
#6043 = CARTESIAN_POINT ( 'NONE',  ( -1.172281656590623111, 158.5855360310326319, 1.517099175104413833 ) ) ;
#6044 = CARTESIAN_POINT ( 'NONE',  ( 12.65084386183212040, 120.1953580586475567, -0.8051295378619940379 ) ) ;
#6045 = CARTESIAN_POINT ( 'NONE',  ( -3.812863311134618183, 2.017465188139291765, -2.614655560905410958 ) ) ;
#6046 = CARTESIAN_POINT ( 'NONE',  ( -57.53431004061603460, 2.062971833132837496, -1.787249339056213637 ) ) ;
#6047 = ORIENTED_EDGE ( 'NONE', *, *, #261, .F. ) ;
#6048 = CARTESIAN_POINT ( 'NONE',  ( -58.34514637059952236, -0.2398883667948381593, -0.1955437934783339493 ) ) ;
#6049 = CARTESIAN_POINT ( 'NONE',  ( 0.4232488410868608941, 124.9344662015457317, 0.008457519121177021690 ) ) ;
#6050 = CARTESIAN_POINT ( 'NONE',  ( -6.654617103318593247E-14, 104.6144662015457243, 1.534725424433578570E-31 ) ) ;
#6051 = CARTESIAN_POINT ( 'NONE',  ( -14.11650378654216631, 131.1061190467503934, 1.279305142450560151 ) ) ;
#6052 = CARTESIAN_POINT ( 'NONE',  ( 5.152689472752729039, 116.8412042436348912, 0.1029629964107459106 ) ) ;
#6053 = CIRCLE ( 'NONE', #35292, 6.350000000000004974 ) ;
#6054 = CARTESIAN_POINT ( 'NONE',  ( 5.877700541659331535, 119.5807162246413498, -0.9453723347071265604 ) ) ;
#6055 = AXIS2_PLACEMENT_3D ( 'NONE', #41594, #12403, #35614 ) ;
#6056 = CARTESIAN_POINT ( 'NONE',  ( -18.56731909478085996, 131.8045874826418071, -2.147352672676718033 ) ) ;
#6057 = CARTESIAN_POINT ( 'NONE',  ( -53.17586183559576085, 10.67386474145934372, -4.017225210190888518 ) ) ;
#6058 = CARTESIAN_POINT ( 'NONE',  ( 4.498274173885895344, 155.8822484669112214, -0.6329996689149901545 ) ) ;
#6059 = ORIENTED_EDGE ( 'NONE', *, *, #13894, .T. ) ;
#6060 = CARTESIAN_POINT ( 'NONE',  ( -0.5133504486497384445, 119.5442839488369628, -0.5494766105906193632 ) ) ;
#6061 = CARTESIAN_POINT ( 'NONE',  ( 3.555255404795384599, -15.46298345743583802, 3.323699395844104565 ) ) ;
#6062 = CARTESIAN_POINT ( 'NONE',  ( -4.149547856688258207, 118.2393522679058009, -0.3953376121465850823 ) ) ;
#6063 = ADVANCED_FACE ( 'NONE', ( #33296 ), #27098, .T. ) ;
#6064 = CARTESIAN_POINT ( 'NONE',  ( -57.60038635073814817, 1.097546858218806376, -1.033898108845213542E-14 ) ) ;
#6065 = CARTESIAN_POINT ( 'NONE',  ( -4.902692966696466925, 117.7192222769238441, 0.7484533029765950696 ) ) ;
#6066 = CARTESIAN_POINT ( 'NONE',  ( 11.83432680469861431, 124.3826620800890339, 1.661842703385269848 ) ) ;
#6067 = CARTESIAN_POINT ( 'NONE',  ( -47.10086694477701030, 25.28009754958737787, 1.863548351650762491 ) ) ;
#6068 = CARTESIAN_POINT ( 'NONE',  ( 2.332027132427558769, 25.33165720878049498, 3.998286310156994983 ) ) ;
#6069 = CARTESIAN_POINT ( 'NONE',  ( 14.27613791431590151, 138.9852717218771261, 0.6171993629658321101 ) ) ;
#6070 = DIRECTION ( 'NONE',  ( -0.01731298258487873332, 0.9998501190848635423, -9.050832817465997210E-15 ) ) ;
#6071 = TOROIDAL_SURFACE ( 'NONE', #30567, 3.683000000000000718, 0.5080000000000000071 ) ;
#6072 = CARTESIAN_POINT ( 'NONE',  ( -48.84381969468221030, 17.12102923570560975, -3.921819500614954102 ) ) ;
#6073 = CARTESIAN_POINT ( 'NONE',  ( -0.2378499585937704497, 117.3993841996711041, 1.487621480530184614 ) ) ;
#6074 = CARTESIAN_POINT ( 'NONE',  ( -10.57002714855771863, 82.40335727708655611, 1.269999999999999796 ) ) ;
#6075 = CARTESIAN_POINT ( 'NONE',  ( -56.45305112249246093, 4.342240606964129945, 2.533486158674154165 ) ) ;
#6076 = CARTESIAN_POINT ( 'NONE',  ( -29.88458269586515925, 69.13647124293702007, -1.270000000000007123 ) ) ;
#6077 = CARTESIAN_POINT ( 'NONE',  ( -5.965356522962928842, 53.58606249999999704, -5.016499999999999737 ) ) ;
#6078 = CARTESIAN_POINT ( 'NONE',  ( -53.73190450750161773, 11.39902669490613896, 3.613030284815563764 ) ) ;
#6079 = CARTESIAN_POINT ( 'NONE',  ( -22.50450395291955275, 150.7830971219523519, -0.1219060866366470514 ) ) ;
#6080 = ORIENTED_EDGE ( 'NONE', *, *, #40749, .T. ) ;
#6081 = CARTESIAN_POINT ( 'NONE',  ( -50.19988854512629217, 18.36332526648348917, -3.854797337117289224 ) ) ;
#6082 = CARTESIAN_POINT ( 'NONE',  ( 6.957078529942896772, 121.9380298548064445, -0.02067918444371699693 ) ) ;
#6083 = CARTESIAN_POINT ( 'NONE',  ( 4.854575378875618519, 117.4045355995268096, -0.9984935320486798549 ) ) ;
#6084 = ORIENTED_EDGE ( 'NONE', *, *, #23404, .F. ) ;
#6085 = CARTESIAN_POINT ( 'NONE',  ( 1.153264477914338615, 115.7029425313346280, -1.700750124145387732 ) ) ;
#6086 = CARTESIAN_POINT ( 'NONE',  ( -15.76687399610644391, 145.9134097338176730, -0.4436328104633034397 ) ) ;
#6087 = CARTESIAN_POINT ( 'NONE',  ( 2.458590490134419770, -15.31022926314896893, 5.890968354261565842 ) ) ;
#6088 = CARTESIAN_POINT ( 'NONE',  ( -17.06313393459315719, 153.7580772870718988, 1.402989014430432668 ) ) ;
#6089 = CARTESIAN_POINT ( 'NONE',  ( -5.010144981628188887, 117.3993855238222608, -0.7522679339500687457 ) ) ;
#6090 = CARTESIAN_POINT ( 'NONE',  ( 23.33231982438472940, 148.8574307740229585, 0.6970557703302366903 ) ) ;
#6091 = CARTESIAN_POINT ( 'NONE',  ( 8.410838065576685452, 123.3149317519321784, 0.2957792723555629499 ) ) ;
#6092 = LINE ( 'NONE', #41666, #1308 ) ;
#6093 = CARTESIAN_POINT ( 'NONE',  ( 0.7153056356866435150, 7.414959551268969662, 0.6636563042211964802 ) ) ;
#6094 = CARTESIAN_POINT ( 'NONE',  ( -6.901437262003314643, 117.1762911274595496, -0.2238905109288658601 ) ) ;
#6095 = CARTESIAN_POINT ( 'NONE',  ( -4.085839532347236513, 71.06758511999679229, -1.523999999999994026 ) ) ;
#6096 = EDGE_CURVE ( 'NONE', #16976, #21597, #30866, .T. ) ;
#6097 = FACE_OUTER_BOUND ( 'NONE', #1294, .T. ) ;
#6098 = EDGE_LOOP ( 'NONE', ( #278, #12115, #24384, #26357 ) ) ;
#6099 = CARTESIAN_POINT ( 'NONE',  ( -5.697209421088824222, 117.9270612091053891, 0.8225170165645491194 ) ) ;
#6100 = ORIENTED_EDGE ( 'NONE', *, *, #19550, .F. ) ;
#6101 = CARTESIAN_POINT ( 'NONE',  ( -58.36736542105735026, -0.2864936770574270097, -0.06035461783101484651 ) ) ;
#6102 = CARTESIAN_POINT ( 'NONE',  ( 12.03559625110886522, 156.5645100661158153, 1.882936990620205808 ) ) ;
#6103 = CARTESIAN_POINT ( 'NONE',  ( 12.82775609536331807, 122.1393999080170971, -1.276540306405074876 ) ) ;
#6104 = CARTESIAN_POINT ( 'NONE',  ( -8.197529660144020625, 8.984976746712527884, 2.078235512056660017 ) ) ;
#6105 = CARTESIAN_POINT ( 'NONE',  ( -11.09758427587551743, 119.2389763063149388, -1.130321237809625234 ) ) ;
#6106 = CARTESIAN_POINT ( 'NONE',  ( 4.657610911615179816, 117.9597807199399000, -0.7455203706293841437 ) ) ;
#6107 = CARTESIAN_POINT ( 'NONE',  ( 8.798071512540863282, 117.6842349196870572, 0.1758064070670784795 ) ) ;
#6108 = CARTESIAN_POINT ( 'NONE',  ( -10.43234786055289653, 153.0845720789597522, -0.001036074960336963707 ) ) ;
#6109 = EDGE_CURVE ( 'NONE', #13560, #20581, #40109, .T. ) ;
#6110 = CARTESIAN_POINT ( 'NONE',  ( -10.72551448100101901, 121.7859837122882283, -1.665033671525604220 ) ) ;
#6112 = CARTESIAN_POINT ( 'NONE',  ( 2.008732664060286055, -15.70244684250787870, 5.701976698490775597 ) ) ;
#6111 = VECTOR ( 'NONE', #27402, 1000.000000000000000 ) ;
#6113 = AXIS2_PLACEMENT_3D ( 'NONE', #13664, #37094, #4731 ) ;
#6114 = CARTESIAN_POINT ( 'NONE',  ( -6.376221727585796537E-14, 51.14746620154573264, 5.777789833161707559E-29 ) ) ;
#6115 = CARTESIAN_POINT ( 'NONE',  ( -47.71508057896579658, 20.49549959222711593, -5.111566084959475731 ) ) ;
#6116 = ORIENTED_EDGE ( 'NONE', *, *, #24581, .T. ) ;
#6117 = CARTESIAN_POINT ( 'NONE',  ( 14.67610382776214628, 152.8628051715174365, 2.323547792494559339 ) ) ;
#6118 = DIRECTION ( 'NONE',  ( -0.9998004120163608288, 0.000000000000000000, -0.01997839162482747608 ) ) ;
#6119 = EDGE_CURVE ( 'NONE', #22153, #37301, #40606, .T. ) ;
#6120 = CARTESIAN_POINT ( 'NONE',  ( -5.878298779570172883, 78.21245918282636467, 1.270000000000002904 ) ) ;
#6121 = CARTESIAN_POINT ( 'NONE',  ( -3.145827930498041880, 117.0475107411037641, 1.097865318250619948 ) ) ;
#6122 = ADVANCED_FACE ( 'NONE', ( #13690 ), #25634, .T. ) ;
#6123 = CARTESIAN_POINT ( 'NONE',  ( 8.391225363336687337, -15.30560670943152957, -0.4339906691978474562 ) ) ;
#6124 = CARTESIAN_POINT ( 'NONE',  ( 15.79391552826336209, 147.6293441119438512, 1.163731531224506899 ) ) ;
#6125 = CARTESIAN_POINT ( 'NONE',  ( 0.01133159106138621405, 159.5297144918048673, -0.5670791535570575137 ) ) ;
#6126 = LINE ( 'NONE', #19091, #7004 ) ;
#6127 = DIRECTION ( 'NONE',  ( -1.000000000000000000, 0.000000000000000000, -0.000000000000000000 ) ) ;
#6128 = CIRCLE ( 'NONE', #28560, 1.000000000000000888 ) ;
#6129 = CARTESIAN_POINT ( 'NONE',  ( -15.19604463793445959, 156.0859089222169587, -0.3036531364422413448 ) ) ;
#6130 = ADVANCED_FACE ( 'NONE', ( #14511, #37113 ), #20267, .F. ) ;
#6131 = ORIENTED_EDGE ( 'NONE', *, *, #29960, .T. ) ;
#6132 = CARTESIAN_POINT ( 'NONE',  ( -8.200576496910658264, 120.4759052327119235, -1.428406516435469342 ) ) ;
#6133 = CARTESIAN_POINT ( 'NONE',  ( 3.038459613674064919, -15.39881274666275779, 5.660802783634620639 ) ) ;
#6134 = CARTESIAN_POINT ( 'NONE',  ( -15.96686920080710870, 146.6619865182943272, -1.046663894505766468 ) ) ;
#6135 = CARTESIAN_POINT ( 'NONE',  ( 13.85159022459153988, 59.63164443796365077, 5.016499999999999737 ) ) ;
#6136 = CARTESIAN_POINT ( 'NONE',  ( 23.34372044207203700, 149.0681261006882039, 0.4664630893996631333 ) ) ;
#6137 = VERTEX_POINT ( 'NONE', #40531 ) ;
#6138 = CARTESIAN_POINT ( 'NONE',  ( -4.012847786888796620, 11.73797844546971270, -2.294585225469591983 ) ) ;
#6139 = CARTESIAN_POINT ( 'NONE',  ( -30.29872984390849311, 56.23795811431430280, 1.523999999999994026 ) ) ;
#6140 = DIRECTION ( 'NONE',  ( -0.000000000000000000, -0.000000000000000000, -1.000000000000000000 ) ) ;
#6141 = DIRECTION ( 'NONE',  ( -5.206863593109713661E-17, 1.000000000000000000, -1.077750396879097183E-30 ) ) ;
#6142 = DIRECTION ( 'NONE',  ( 0.4849315768086535638, 0.8745520943968251304, 1.030032898892975065E-16 ) ) ;
#6143 = CARTESIAN_POINT ( 'NONE',  ( 6.049108887567863135, 120.6719078856681193, 0.9521718272089157997 ) ) ;
#6144 = CARTESIAN_POINT ( 'NONE',  ( 4.531904421025400254, 4.026177021345840323, -0.9239884639389631671 ) ) ;
#6145 = CARTESIAN_POINT ( 'NONE',  ( -0.007599820978813201684, 117.2191897141855179, 0.3803261187632672735 ) ) ;
#6146 = CARTESIAN_POINT ( 'NONE',  ( 15.78437780952694069, 146.2378312303354448, 0.3154094333657936899 ) ) ;
#6148 = CARTESIAN_POINT ( 'NONE',  ( 1.211137314531071985, 158.8088198215516229, -1.425359051240900232 ) ) ;
#6147 = CARTESIAN_POINT ( 'NONE',  ( 2.666490510518176649, -13.49855353256042889, 0.05227394649444832425 ) ) ;
#6149 = CARTESIAN_POINT ( 'NONE',  ( -1.441504266290200897, 6.599927940091079748, -4.410093354674724964 ) ) ;
#6150 = CARTESIAN_POINT ( 'NONE',  ( -14.90772019895849709, 120.8072429308574414, -0.9794594453158805836 ) ) ;
#6151 = ORIENTED_EDGE ( 'NONE', *, *, #38941, .T. ) ;
#6152 = ADVANCED_FACE ( 'NONE', ( #40324 ), #11323, .T. ) ;
#6153 = CARTESIAN_POINT ( 'NONE',  ( -3.022581645176320553, 156.1079525116674631, 0.4343475099915219961 ) ) ;
#6154 = CARTESIAN_POINT ( 'NONE',  ( 5.218988718559132600, -14.41095047787725747, 3.833162268628383718 ) ) ;
#6155 = CARTESIAN_POINT ( 'NONE',  ( -5.008987216574991130, 117.3966124399498199, 0.7756614662348499944 ) ) ;
#6156 = CARTESIAN_POINT ( 'NONE',  ( -4.635334609548626084, 118.0286145527519039, -0.7659634255356302379 ) ) ;
#6157 = CARTESIAN_POINT ( 'NONE',  ( 15.64289809528657926, 147.2198192248932571, 0.2613308799247722747 ) ) ;
#6158 = B_SPLINE_CURVE_WITH_KNOTS ( 'NONE', 3,
 ( #16161, #19364, #16378, #3843, #30014, #29809, #12771, #35786, #649, #10420, #25761, #38768, #26396, #35996, #22548, #436, #19570, #13198, #22754, #39185, #13406, #9579, #23391, #36208, #22966, #6394, #32369, #38978, #3410, #23174, #11, #6599, #7030, #3199, #12977, #9786, #29383, #223, #9994, #36423, #25970, #6809, #29602, #10204, #33015, #13617, #16593, #19778, #32798 ),
 .UNSPECIFIED., .F., .F.,
 ( 4, 1, 1, 1, 1, 1, 1, 1, 1, 1, 1, 1, 1, 1, 1, 1, 1, 1, 1, 1, 1, 1, 1, 1, 1, 1, 1, 1, 1, 1, 1, 1, 1, 1, 1, 1, 1, 1, 1, 1, 1, 1, 1, 1, 1, 1, 4 ),
 ( 0.000000000000000000, 0.007812500000000000000, 0.01562500000000000000, 0.02343750000000000000, 0.03125000000000000000, 0.04687500000000000000, 0.06250000000000000000, 0.07812500000000000000, 0.09375000000000000000, 0.1093750000000000000, 0.1250000000000000000, 0.1406250000000000000, 0.1562500000000000000, 0.1875000000000000000, 0.2187500000000000000, 0.2500000000000000000, 0.2812500000000000000, 0.3125000000000000000, 0.3281250000000000000, 0.3437500000000000000, 0.3750000000000000000, 0.4062500000000000000, 0.4375000000000000000, 0.4687500000000000000, 0.5000000000000000000, 0.5312500000000000000, 0.5625000000000000000, 0.5937500000000000000, 0.6250000000000000000, 0.6562500000000000000, 0.6718750000000000000, 0.6875000000000000000, 0.7187500000000000000, 0.7500000000000000000, 0.7812500000000000000, 0.8125000000000000000, 0.8437500000000000000, 0.8750000000000000000, 0.8906250000000000000, 0.9062500000000000000, 0.9218750000000000000, 0.9375000000000000000, 0.9531250000000000000, 0.9687500000000000000, 0.9765625000000000000, 0.9843750000000000000, 1.000000000000000000 ),
 .UNSPECIFIED. ) ;
#6159 = ORIENTED_EDGE ( 'NONE', *, *, #30069, .T. ) ;
#6160 = CARTESIAN_POINT ( 'NONE',  ( 13.64693284513001004, 123.6869008171703541, 1.914747182567867023 ) ) ;
#6161 = CARTESIAN_POINT ( 'NONE',  ( 3.174366308151881810, 76.29346620154572634, 0.06343139340882768262 ) ) ;
#6162 = CARTESIAN_POINT ( 'NONE',  ( 9.538359384048550993, 124.8019839352694476, 0.1905991205270211042 ) ) ;
#6163 = CARTESIAN_POINT ( 'NONE',  ( -2.917496378899196774, 117.0242007548465608, 0.3950530357975751139 ) ) ;
#6164 = ADVANCED_FACE ( 'NONE', ( #30499, #1130 ), #24312, .T. ) ;
#6165 = LINE ( 'NONE', #38330, #749 ) ;
#6166 = CARTESIAN_POINT ( 'NONE',  ( 21.39485547647971586, 132.5159896776619917, 0.01683271311856786301 ) ) ;
#6167 = CARTESIAN_POINT ( 'NONE',  ( 5.266289895157169814E-14, 83.56599999999998829, 1.904999999999999805 ) ) ;
#6168 = CARTESIAN_POINT ( 'NONE',  ( -46.82598356868722789, 25.66206020625350348, 1.525368666045084032 ) ) ;
#6169 = CARTESIAN_POINT ( 'NONE',  ( -46.72476011081990066, 26.09744872113180847, 0.08471799968938857617 ) ) ;
#6170 = AXIS2_PLACEMENT_3D ( 'NONE', #9533, #32536, #19529 ) ;
#6171 = FACE_OUTER_BOUND ( 'NONE', #34367, .T. ) ;
#6172 = CARTESIAN_POINT ( 'NONE',  ( -47.71508057896579658, 20.49549959222711593, 5.111566084959459744 ) ) ;
#6173 = CARTESIAN_POINT ( 'NONE',  ( -6.654617103318593247E-14, 104.6144662015457243, 1.534725424433578570E-31 ) ) ;
#6174 = CARTESIAN_POINT ( 'NONE',  ( -4.600121016240784400, 118.0774895349771327, 0.5278871946396123116 ) ) ;
#6175 = ORIENTED_EDGE ( 'NONE', *, *, #15168, .F. ) ;
#6176 = ORIENTED_EDGE ( 'NONE', *, *, #3424, .F. ) ;
#6177 = CARTESIAN_POINT ( 'NONE',  ( -5.008987216574991130, 117.3966124399498199, 0.7756614662348499944 ) ) ;
#6178 = CARTESIAN_POINT ( 'NONE',  ( 3.500270007598507149, 118.6368327427319400, -0.7934551251016943585 ) ) ;
#6179 = CARTESIAN_POINT ( 'NONE',  ( -7.643894675291609708, 124.7210964017841377, -0.1527028184316445991 ) ) ;
#6181 = CARTESIAN_POINT ( 'NONE',  ( 4.720176955733354163, 117.9455280608507337, 0.8233293243692888508 ) ) ;
#6180 = AXIS2_PLACEMENT_3D ( 'NONE', #31773, #22156, #31347 ) ;
#6182 = CARTESIAN_POINT ( 'NONE',  ( 3.216700609619024931, -14.42020774479446921, 2.887214088933996337 ) ) ;
#6183 = CARTESIAN_POINT ( 'NONE',  ( -11.02756477914281419, 153.1537610418535849, -1.395931567138233076 ) ) ;
#6184 = CARTESIAN_POINT ( 'NONE',  ( -1.783861003286922209, 115.7029489855490851, -1.723409893597471543 ) ) ;
#6185 = DIRECTION ( 'NONE',  ( 1.000000000000000000, 6.353134868986659519E-16, 0.000000000000000000 ) ) ;
#6186 = LINE ( 'NONE', #19361, #18516 ) ;
#6187 = CARTESIAN_POINT ( 'NONE',  ( 6.130181428581209069, 119.5149100643186983, -0.2724793030934817839 ) ) ;
#6188 = CARTESIAN_POINT ( 'NONE',  ( -3.575075884023375394, 156.6183338678525558, -1.521800568792661013 ) ) ;
#6189 = CARTESIAN_POINT ( 'NONE',  ( -13.46199999999999442, 12.17394877578617063, 1.648619521012166368E-15 ) ) ;
#6190 = CARTESIAN_POINT ( 'NONE',  ( 5.078986093043053707, 82.13546620154573930, 0.1014902294541238092 ) ) ;
#6191 = CARTESIAN_POINT ( 'NONE',  ( -4.358130382724847429, 115.7036741551124663, 1.373039722754557657 ) ) ;
#6192 = CARTESIAN_POINT ( 'NONE',  ( 2.584458374606236841, 15.83607344512877368, 3.832284875798456447 ) ) ;
#6194 = VERTEX_POINT ( 'NONE', #39898 ) ;
#6193 = CARTESIAN_POINT ( 'NONE',  ( 3.185756255432559580, 159.4163042773305676, 0.6073767776667650109 ) ) ;
#6195 = CARTESIAN_POINT ( 'NONE',  ( 0.8444020299261373319, 104.6144662015456674, -4.761538540800747121 ) ) ;
#6196 = CARTESIAN_POINT ( 'NONE',  ( 3.394867371861720606, -15.19666007832035071, 3.108802900814295000 ) ) ;
#6197 = CARTESIAN_POINT ( 'NONE',  ( -7.611130975157204048, 119.9600249249614592, 1.076879093209133664 ) ) ;
#6198 = CARTESIAN_POINT ( 'NONE',  ( 0.9581548452940278349, 12.22225311242794099, 0.1719060106794997322 ) ) ;
#6199 = CARTESIAN_POINT ( 'NONE',  ( 0.9340445150430609633, -0.5783478219614121008, -0.2901879621234355056 ) ) ;
#6200 = ORIENTED_EDGE ( 'NONE', *, *, #29018, .T. ) ;
#6201 = ORIENTED_EDGE ( 'NONE', *, *, #20106, .F. ) ;
#6202 = DIRECTION ( 'NONE',  ( 0.8745520943968243532, -0.4849315768086547296, 6.829619984160642269E-16 ) ) ;
#6203 = CARTESIAN_POINT ( 'NONE',  ( 5.854120942168423269, 124.7508695889173111, 0.1197652058513697382 ) ) ;
#6204 = DIRECTION ( 'NONE',  ( 0.000000000000000000, 0.000000000000000000, 1.000000000000000000 ) ) ;
#6205 = CARTESIAN_POINT ( 'NONE',  ( -9.963230294258281106, 124.0638329749226330, 0.5989708749582572933 ) ) ;
#6206 = DIRECTION ( 'NONE',  ( 0.01997839162482793751, 0.000000000000000000, -0.9998004120163608288 ) ) ;
#6207 = CARTESIAN_POINT ( 'NONE',  ( 2.073997095138572000, -14.95492255878227894, 5.604884748988061105 ) ) ;
#6208 = CARTESIAN_POINT ( 'NONE',  ( 18.00062125403720970, 147.1528319293316542, -1.577578161537398271 ) ) ;
#6209 = CARTESIAN_POINT ( 'NONE',  ( -14.08011273344106939, 154.3735777161816429, -2.279704494881448884 ) ) ;
#6210 = CARTESIAN_POINT ( 'NONE',  ( -18.35410564743290607, 77.35382415001784295, 1.904999999999988480 ) ) ;
#6211 = CIRCLE ( 'NONE', #29995, 0.3809999999999984510 ) ;
#6212 = DIRECTION ( 'NONE',  ( -0.9998004120163608288, -5.205824365704082573E-17, -0.01997839162482763914 ) ) ;
#6213 = CARTESIAN_POINT ( 'NONE',  ( -2.613675400483765010, 35.04346971370642905, 1.554312572134140424 ) ) ;
#6214 = CARTESIAN_POINT ( 'NONE',  ( 11.35800195117471745, 128.2076764602477681, -0.1601657033123584928 ) ) ;
#6215 = ORIENTED_EDGE ( 'NONE', *, *, #40126, .T. ) ;
#6216 = DIRECTION ( 'NONE',  ( -0.7548010569845180484, -0.6559537821943359770, 0.000000000000000000 ) ) ;
#6217 = AXIS2_PLACEMENT_3D ( 'NONE', #41108, #28523, #8303 ) ;
#6218 = CARTESIAN_POINT ( 'NONE',  ( -3.216045294022573664, 29.79186273158684983, 3.430717191674401700 ) ) ;
#6219 = CARTESIAN_POINT ( 'NONE',  ( 4.977872327462655733, 117.5914563484107447, -0.7726522923643426299 ) ) ;
#6220 = CARTESIAN_POINT ( 'NONE',  ( 9.472608709197571031, 123.5188755717998816, 0.9573233835003832626 ) ) ;
#6221 = DIRECTION ( 'NONE',  ( 0.9998004120163609398, 0.000000000000000000, 0.01997839162482749689 ) ) ;
#6222 = CARTESIAN_POINT ( 'NONE',  ( 8.217303172778491316, 117.5015518944296247, 0.1195796404652191836 ) ) ;
#6223 = CARTESIAN_POINT ( 'NONE',  ( -5.257173101726059450, 116.1034411669277375, 1.028648520082846574 ) ) ;
#6224 = DIRECTION ( 'NONE',  ( -0.8745520943968235761, 0.4849315768086558398, -4.268512490100410909E-16 ) ) ;
#6225 = DIRECTION ( 'NONE',  ( 9.627370216492862708E-17, 1.000000000000000000, -0.000000000000000000 ) ) ;
#6226 = CARTESIAN_POINT ( 'NONE',  ( -3.391986336308672634, 31.79029220026756519, 0.7414760692215754956 ) ) ;
#6227 = CARTESIAN_POINT ( 'NONE',  ( 20.88630183647680028, 148.3608207065297222, 2.399927473325583094 ) ) ;
#6228 = CARTESIAN_POINT ( 'NONE',  ( 5.478597439045088890, 28.15663318097115209, -6.435035585623773535 ) ) ;
#6229 = CARTESIAN_POINT ( 'NONE',  ( 2.190996476981287966, 116.7774030019725444, -0.4241678434939673004 ) ) ;
#6230 = CARTESIAN_POINT ( 'NONE',  ( -0.08587196332417050548, 108.5751225745497806, -4.267111774705384164 ) ) ;
#6231 = CARTESIAN_POINT ( 'NONE',  ( -22.66375647020940320, 150.6386093215953679, -0.4528757910175281731 ) ) ;
#6232 = CARTESIAN_POINT ( 'NONE',  ( 4.854633716284414646, 115.7029491485453292, -1.279498648767039448 ) ) ;
#6233 = CARTESIAN_POINT ( 'NONE',  ( 1.821748264913740423, 104.6144662015434932, 5.025386274610280424 ) ) ;
#6234 = CIRCLE ( 'NONE', #799, 0.2539999999999932867 ) ;
#6235 = CARTESIAN_POINT ( 'NONE',  ( -4.151662239014343392, 13.23730288530712862, 2.070234887608822572 ) ) ;
#6236 = FACE_OUTER_BOUND ( 'NONE', #2164, .T. ) ;
#6237 = FACE_OUTER_BOUND ( 'NONE', #22954, .T. ) ;
#6238 = CARTESIAN_POINT ( 'NONE',  ( 3.131463087139035206, -14.49961247625831895, 3.567833873788547550 ) ) ;
#6239 = CARTESIAN_POINT ( 'NONE',  ( 1.803835135052165084, 120.9773948236336878, -0.3431470217397347144 ) ) ;
#6240 = CARTESIAN_POINT ( 'NONE',  ( -8.157450159232212172, 117.7673425867732249, 0.3794901880580580644 ) ) ;
#6241 = VERTEX_POINT ( 'NONE', #7517 ) ;
#6242 = DIRECTION ( 'NONE',  ( 0.9998004120163608288, 0.000000000000000000, 0.01997839162482749342 ) ) ;
#6243 = ORIENTED_EDGE ( 'NONE', *, *, #14042, .F. ) ;
#6244 = CARTESIAN_POINT ( 'NONE',  ( -41.09670346151852982, 23.04688172093031895, -1.270085369932521191 ) ) ;
#6245 = AXIS2_PLACEMENT_3D ( 'NONE', #16132, #42153, #195 ) ;
#6246 = CARTESIAN_POINT ( 'NONE',  ( 2.438853454531733966, -15.63545089637397112, 5.735818209389550226 ) ) ;
#6247 = CARTESIAN_POINT ( 'NONE',  ( -12.92430874792265350, 121.9120276846612256, 1.237792553996327261 ) ) ;
#6248 = CARTESIAN_POINT ( 'NONE',  ( 14.74288075364456674, 121.6338672040446767, -0.8423781477486336211 ) ) ;
#6249 = CARTESIAN_POINT ( 'NONE',  ( 4.440276399826426967, -1.430929408009915083, -1.287880193523989636 ) ) ;
#6250 = CARTESIAN_POINT ( 'NONE',  ( -57.65317970594307440, 1.808445652233532597, -1.687761604364059309 ) ) ;
#6251 = ORIENTED_EDGE ( 'NONE', *, *, #32887, .F. ) ;
#6252 = CARTESIAN_POINT ( 'NONE',  ( -58.39415239746203667, -0.3126312442486959831, -0.4522786855619334023 ) ) ;
#6253 = CARTESIAN_POINT ( 'NONE',  ( -0.06282972276541670675, 111.5577547982949227, 3.144256248693278355 ) ) ;
#6254 = CARTESIAN_POINT ( 'NONE',  ( -17.21539028065174293, 147.4900653055648547, 1.363477025422525024 ) ) ;
#6255 = CARTESIAN_POINT ( 'NONE',  ( 5.010184479710102501, 117.3993854065330851, 0.7504461923096029663 ) ) ;
#6256 = CARTESIAN_POINT ( 'NONE',  ( 3.316780243214140889, 119.1333808041459577, -0.7607270569537704086 ) ) ;
#6257 = CARTESIAN_POINT ( 'NONE',  ( -2.699166815671299346, 158.5977336698458089, -1.597229775447004396 ) ) ;
#6258 = CARTESIAN_POINT ( 'NONE',  ( -58.11258158571958177, 1.603013069906233934, -1.501710181103033781 ) ) ;
#6259 = EDGE_LOOP ( 'NONE', ( #29322, #37213, #8376, #41871, #8928 ) ) ;
#6260 = CARTESIAN_POINT ( 'NONE',  ( 4.380560454800319192, 118.1845274366070129, -0.4312657318652557970 ) ) ;
#6261 = CARTESIAN_POINT ( 'NONE',  ( 9.625125523471051991, 124.0356975489027036, -0.4152212053287653304 ) ) ;
#6262 = ORIENTED_EDGE ( 'NONE', *, *, #11061, .T. ) ;
#6263 = CARTESIAN_POINT ( 'NONE',  ( -2.024284171598574655, 156.9412006218898057, -1.489060257140892407 ) ) ;
#6264 = CARTESIAN_POINT ( 'NONE',  ( 2.120377039319510715, -15.39027815159008128, 5.169171589912422426 ) ) ;
#6265 = VECTOR ( 'NONE', #18986, 1000.000000000000114 ) ;
#6266 = CARTESIAN_POINT ( 'NONE',  ( -4.111767271380013078, 118.2429491485453070, -0.3463599732680077148 ) ) ;
#6267 = AXIS2_PLACEMENT_3D ( 'NONE', #23486, #17110, #30111 ) ;
#6268 = CARTESIAN_POINT ( 'NONE',  ( -56.42856387642239469, 3.193865871111076338, -9.978765949893178940E-15 ) ) ;
#6269 = CARTESIAN_POINT ( 'NONE',  ( -4.825021315912614739, 117.6416127849941802, 0.9313223449158248846 ) ) ;
#6270 = CARTESIAN_POINT ( 'NONE',  ( 7.307041242074578058, 120.9764928074160082, 1.161154363956387492 ) ) ;
#6271 = LINE ( 'NONE', #16248, #16510 ) ;
#6272 = CARTESIAN_POINT ( 'NONE',  ( 1.580769961479467911, 28.79261460129497863, -4.363931058323818668 ) ) ;
#6273 = CARTESIAN_POINT ( 'NONE',  ( 7.868938471672396240, 154.6027768716304820, 0.5345728592648683053 ) ) ;
#6274 = DIRECTION ( 'NONE',  ( -0.3256999990547930768, -0.9454731675810308378, -6.956556933070078754E-15 ) ) ;
#6276 = ORIENTED_EDGE ( 'NONE', *, *, #37635, .T. ) ;
#6275 = CARTESIAN_POINT ( 'NONE',  ( -47.93564525088159201, 15.36257551998192916, -0.4079155175245698373 ) ) ;
#6277 = DIRECTION ( 'NONE',  ( 1.011795553208986377E-16, 1.000000000000000000, -0.000000000000000000 ) ) ;
#6278 = CARTESIAN_POINT ( 'NONE',  ( -46.73847652112046092, 25.90099053509251092, -1.386667892818581160 ) ) ;
#6279 = CARTESIAN_POINT ( 'NONE',  ( -53.84203694985585287, 9.550030682661965642, 3.786207223046024861 ) ) ;
#6280 = DIRECTION ( 'NONE',  ( -4.017660918040594346E-17, 1.000000000000000000, 2.376309959284834438E-19 ) ) ;
#6281 = CARTESIAN_POINT ( 'NONE',  ( -12.79279280188648116, 63.69337819391066091, 1.524000000000002242 ) ) ;
#6282 = CARTESIAN_POINT ( 'NONE',  ( -5.965356522962950159, 88.73331249999999670, -5.016499999999999737 ) ) ;
#6283 = CARTESIAN_POINT ( 'NONE',  ( -55.74683331106318462, 9.129907917338066170, 0.4890489271862150100 ) ) ;
#6284 = CARTESIAN_POINT ( 'NONE',  ( -0.9295402922912642252, 116.5712332538976455, 0.1496640007645970161 ) ) ;
#6285 = EDGE_LOOP ( 'NONE', ( #208, #36050, #31648, #20253 ) ) ;
#6286 = EDGE_LOOP ( 'NONE', ( #8296, #31096, #31369, #20347 ) ) ;
#6287 = CARTESIAN_POINT ( 'NONE',  ( -51.24266872689721453, 19.11669921072455836, -1.581762766848686885 ) ) ;
#6288 = CARTESIAN_POINT ( 'NONE',  ( -7.813505862531938462, 122.4480138429351683, -0.5609622212283363885 ) ) ;
#6289 = ORIENTED_EDGE ( 'NONE', *, *, #32124, .F. ) ;
#6290 = CARTESIAN_POINT ( 'NONE',  ( 1.199038730579973677, 115.7029469957295191, -1.697507966841996563 ) ) ;
#6291 = CARTESIAN_POINT ( 'NONE',  ( -9.611064403080925800, 124.8310256250372277, -0.2802631513932193896 ) ) ;
#6292 = CARTESIAN_POINT ( 'NONE',  ( 2.083301838685661878, -15.46665383083971257, 5.961979448439955753 ) ) ;
#6293 = CARTESIAN_POINT ( 'NONE',  ( -12.31483450803191104, 120.4651188882986759, 0.9715887866197354672 ) ) ;
#6294 = CARTESIAN_POINT ( 'NONE',  ( 5.809014734623085374, 78.89492211486508211, -5.027281507146220463 ) ) ;
#6295 = CIRCLE ( 'NONE', #30093, 0.5080000000000002292 ) ;
#6296 = CARTESIAN_POINT ( 'NONE',  ( 23.16647984970247620, 149.6103952014060212, 0.7935852015942148618 ) ) ;
#6297 = CARTESIAN_POINT ( 'NONE',  ( 7.537398615003564117, 122.4256905169532388, 0.2304582891925715249 ) ) ;
#6298 = CARTESIAN_POINT ( 'NONE',  ( -29.82321757229076908, 71.17901112636586447, -1.524000000000007349 ) ) ;
#6299 = CARTESIAN_POINT ( 'NONE',  ( -0.08934464221186895483, 15.61415217803747169, 0.9739947352787643453 ) ) ;
#6300 = CARTESIAN_POINT ( 'NONE',  ( -17.17229002331743004, 122.7237354506536491, -0.5096938506424069093 ) ) ;
#6301 = FACE_OUTER_BOUND ( 'NONE', #41934, .T. ) ;
#6302 = CARTESIAN_POINT ( 'NONE',  ( 12.21488373879589240, 12.96416000000000146, 4.381499999999999950 ) ) ;
#6303 = CARTESIAN_POINT ( 'NONE',  ( -8.715372737337569120, 118.1578756808219168, 0.5461737873414159727 ) ) ;
#6304 = ORIENTED_EDGE ( 'NONE', *, *, #33905, .F. ) ;
#6305 = CARTESIAN_POINT ( 'NONE',  ( -58.36849006653898897, -0.2888454140588792018, -0.04296944658959341024 ) ) ;
#6306 = CARTESIAN_POINT ( 'NONE',  ( 5.844526503020529340, 118.0670013439590491, 1.005764768584936686 ) ) ;
#6307 = CARTESIAN_POINT ( 'NONE',  ( 3.207104841129760242, 118.4902560533893592, -0.7629184910595987468 ) ) ;
#6308 = CARTESIAN_POINT ( 'NONE',  ( -6.647063868753328997, 9.619588520696709111, 5.217091374630535405 ) ) ;
#6309 = CARTESIAN_POINT ( 'NONE',  ( -21.32959265000934579, 150.3702682424204511, -2.003547396033109163 ) ) ;
#6310 = CARTESIAN_POINT ( 'NONE',  ( 4.646224276046603485, 117.9817966608726323, -0.7219288950694058293 ) ) ;
#6311 = CARTESIAN_POINT ( 'NONE',  ( 6.937169949972861183, 121.8132169909553966, 0.2949249740950675158 ) ) ;
#6312 = VECTOR ( 'NONE', #1616, 1000.000000000000000 ) ;
#6313 = CARTESIAN_POINT ( 'NONE',  ( -9.568355480995553108, 124.8108731098830049, -0.1557749891131962605 ) ) ;
#6314 = CARTESIAN_POINT ( 'NONE',  ( -0.4763900686813665741, 119.0154928070276412, -0.6070730232697146844 ) ) ;
#6315 = CARTESIAN_POINT ( 'NONE',  ( 3.081975983035755373, -15.74694164559999088, 5.217090789712465870 ) ) ;
#6316 = DIRECTION ( 'NONE',  ( -0.6294287539884059202, -0.7770581983690814099, -1.945484789722797322E-16 ) ) ;
#6317 = EDGE_CURVE ( 'NONE', #5065, #14379, #10490, .T. ) ;
#6318 = CARTESIAN_POINT ( 'NONE',  ( -46.82679756180435504, 21.08486709759267086, -4.907624977305287572 ) ) ;
#6319 = EDGE_LOOP ( 'NONE', ( #11536, #38368, #8509, #24109 ) ) ;
#6320 = CARTESIAN_POINT ( 'NONE',  ( 18.42282194684149133, 148.3462492009778373, 2.436111078577046118 ) ) ;
#6321 = DIRECTION ( 'NONE',  ( 0.9998004120163608288, 0.000000000000000000, 0.01997839162482749342 ) ) ;
#6322 = DIRECTION ( 'NONE',  ( 5.188838149069472160E-16, -1.699382548006136559E-16, -1.000000000000000000 ) ) ;
#6323 = CIRCLE ( 'NONE', #23964, 9.048749999999998295 ) ;
#6324 = CARTESIAN_POINT ( 'NONE',  ( -2.721163413801487518, 112.7379566594982663, 2.570110030560514680 ) ) ;
#6325 = CARTESIAN_POINT ( 'NONE',  ( -7.524129562762011503, 22.75916136179084859, 3.848622047589015160 ) ) ;
#6326 = CARTESIAN_POINT ( 'NONE',  ( 3.037839899925966147, 156.1243923452879017, 0.6481072647156853606 ) ) ;
#6327 = EDGE_CURVE ( 'NONE', #1883, #8736, #26921, .T. ) ;
#6328 = CARTESIAN_POINT ( 'NONE',  ( 15.53115535783863699, 121.4967652112180048, -0.4657050394012308692 ) ) ;
#6329 = DIRECTION ( 'NONE',  ( -0.01997839162482761832, -1.040247600000950455E-18, 0.9998004120163610509 ) ) ;
#6330 = CARTESIAN_POINT ( 'NONE',  ( -58.37002191173434795, -0.2919876190278939410, 0.009343179624763268964 ) ) ;
#6331 = AXIS2_PLACEMENT_3D ( 'NONE', #29319, #22690, #19507 ) ;
#6332 = AXIS2_PLACEMENT_3D ( 'NONE', #39010, #36607, #10604 ) ;
#6333 = CARTESIAN_POINT ( 'NONE',  ( -23.41930689910524421, 142.8308675865925181, -0.4425677471174259137 ) ) ;
#6334 = VERTEX_POINT ( 'NONE', #36910 ) ;
#6335 = CARTESIAN_POINT ( 'NONE',  ( 4.871727757954943172, 119.9531087571945136, -0.7028895344987076133 ) ) ;
#6336 = CARTESIAN_POINT ( 'NONE',  ( 4.210393360348192004, -15.14515747025066084, 4.947006310901637782 ) ) ;
#6337 = CARTESIAN_POINT ( 'NONE',  ( -15.96902210417531620, 146.0164801329953548, -1.048924711619906969 ) ) ;
#6338 = CARTESIAN_POINT ( 'NONE',  ( 4.295506980234458538, -13.52603301450379369, 3.694598940018447575 ) ) ;
#6339 = DIRECTION ( 'NONE',  ( 0.8745520943968235761, -0.4849315768086558398, 4.268512490100410909E-16 ) ) ;
#6340 = CARTESIAN_POINT ( 'NONE',  ( 9.819578298035914088, 117.9942579372833933, 0.2115136170467759036 ) ) ;
#6341 = ORIENTED_EDGE ( 'NONE', *, *, #25441, .T. ) ;
#6342 = CARTESIAN_POINT ( 'NONE',  ( 3.263621351691376571, 8.939281053574255509, -3.290156819607050753 ) ) ;
#6343 = ADVANCED_FACE ( 'NONE', ( #16877, #33505 ), #20694, .F. ) ;
#6344 = CARTESIAN_POINT ( 'NONE',  ( -2.123093575600416560, 105.1241855340452247, 4.902909873598239265 ) ) ;
#6345 = CARTESIAN_POINT ( 'NONE',  ( -4.976634676106532318, 117.4097617497457975, 0.8837896011837403920 ) ) ;
#6346 = LINE ( 'NONE', #35950, #30598 ) ;
#6347 = CARTESIAN_POINT ( 'NONE',  ( -5.036351857865265735, 117.3993844875897139, 0.5494637324817667201 ) ) ;
#6348 = CARTESIAN_POINT ( 'NONE',  ( -7.902730875908052788, 122.1217003200704028, 0.5555494452425332463 ) ) ;
#6349 = EDGE_CURVE ( 'NONE', #32297, #10071, #8639, .T. ) ;
#6350 = CARTESIAN_POINT ( 'NONE',  ( -4.422273941422524501, 8.986318502778324557, 1.404945367500548548 ) ) ;
#6351 = CARTESIAN_POINT ( 'NONE',  ( 7.681555067352521249, 158.5863655655865330, 1.054772010160867080 ) ) ;
#6352 = CARTESIAN_POINT ( 'NONE',  ( -0.03519895178523997636, 115.7029491485446613, 1.761499482104069703 ) ) ;
#6353 = CARTESIAN_POINT ( 'NONE',  ( 4.967439785005383968, 118.2512723699127832, -0.8146033317824222797 ) ) ;
#6354 = CARTESIAN_POINT ( 'NONE',  ( -4.468841950160419962, 8.124252568732815760, -1.173904233648782158 ) ) ;
#6355 = CARTESIAN_POINT ( 'NONE',  ( -15.49230080900824369, 121.3130774642648220, -1.004719031932798767 ) ) ;
#6356 = ADVANCED_FACE ( 'NONE', ( #1342 ), #27310, .T. ) ;
#6357 = ORIENTED_EDGE ( 'NONE', *, *, #2992, .F. ) ;
#6358 = CARTESIAN_POINT ( 'NONE',  ( -6.164480127824659483, 155.3548635187015350, 0.4492659787150439232 ) ) ;
#6359 = CARTESIAN_POINT ( 'NONE',  ( 2.081461833008368512, -15.42522581128935499, 5.972092850182497692 ) ) ;
#6360 = DIRECTION ( 'NONE',  ( -0.8745520943968235761, 0.4849315768086558953, -5.361993529360570985E-16 ) ) ;
#6361 = CARTESIAN_POINT ( 'NONE',  ( 15.77260762454789322, 146.5697412905949477, 0.2637713227210860545 ) ) ;
#6362 = ORIENTED_EDGE ( 'NONE', *, *, #14169, .F. ) ;
#6363 = CARTESIAN_POINT ( 'NONE',  ( 13.08242246048928514, 122.4605402651681487, 1.816276721775475611 ) ) ;
#6364 = CARTESIAN_POINT ( 'NONE',  ( 18.35410564743290962, 77.35382415001784295, 5.392902600000138769 ) ) ;
#6365 = CARTESIAN_POINT ( 'NONE',  ( 8.112862105095262066, 122.9271997657419604, 0.1621142923985558204 ) ) ;
#6366 = CARTESIAN_POINT ( 'NONE',  ( -14.73113557689553588, 120.8948172685174001, 0.5329945393104404960 ) ) ;
#6367 = FACE_OUTER_BOUND ( 'NONE', #2092, .T. ) ;
#6368 = CARTESIAN_POINT ( 'NONE',  ( 6.918545264603641165, 117.3320596397172721, -0.2494728033470789974 ) ) ;
#6369 = CARTESIAN_POINT ( 'NONE',  ( -4.800085724567980883, 115.7029491485352537, -1.472342921364584889 ) ) ;
#6370 = AXIS2_PLACEMENT_3D ( 'NONE', #32696, #16276, #28864 ) ;
#6371 = CARTESIAN_POINT ( 'NONE',  ( -47.96057925449625259, 19.24834700699408074, 5.203605657935928441 ) ) ;
#6372 = CARTESIAN_POINT ( 'NONE',  ( -47.29848140234559395, 25.70219632838243484, -8.387873617975133388E-15 ) ) ;
#6373 = CARTESIAN_POINT ( 'NONE',  ( -4.937504354476867086, 117.4086944262769237, -1.082066183473587850 ) ) ;
#6374 = ORIENTED_EDGE ( 'NONE', *, *, #27979, .F. ) ;
#6375 = CARTESIAN_POINT ( 'NONE',  ( -42.34481381083929818, 23.19759442052183473, 1.554397948409609542 ) ) ;
#6376 = DIRECTION ( 'NONE',  ( 0.9876665170007969952, -0.1565721916417935344, 5.390917751951444915E-16 ) ) ;
#6377 = CARTESIAN_POINT ( 'NONE',  ( -4.579105009936609960, 118.0741109548545467, 0.5987129210286493697 ) ) ;
#6378 = LINE ( 'NONE', #10406, #10431 ) ;
#6379 = EDGE_CURVE ( 'NONE', #22830, #2471, #27007, .T. ) ;
#6380 = VERTEX_POINT ( 'NONE', #34554 ) ;
#6381 = ORIENTED_EDGE ( 'NONE', *, *, #363, .F. ) ;
#6382 = CARTESIAN_POINT ( 'NONE',  ( -4.800388046789877627, 115.6909491485452719, -1.474219336061443952 ) ) ;
#6383 = CARTESIAN_POINT ( 'NONE',  ( 5.961890394766238721, 119.1281689002219082, -1.026328349456139488 ) ) ;
#6384 = CARTESIAN_POINT ( 'NONE',  ( -7.065765265293135755, 122.4340714744230496, -0.2508917249367680902 ) ) ;
#6385 = CARTESIAN_POINT ( 'NONE',  ( 4.707952333973207892, 117.9523840734817810, 0.8425572090526738389 ) ) ;
#6386 = CARTESIAN_POINT ( 'NONE',  ( -36.79765817521327165, 27.64956762128695900, -1.524000000000003574 ) ) ;
#6387 = CARTESIAN_POINT ( 'NONE',  ( -9.210551279805695657, 123.0263237342149978, -1.033454686166954017 ) ) ;
#6388 = VECTOR ( 'NONE', #33681, 1000.000000000000000 ) ;
#6389 =( NAMED_UNIT ( * ) SI_UNIT ( $, .STERADIAN. ) SOLID_ANGLE_UNIT ( ) );
#6390 = CARTESIAN_POINT ( 'NONE',  ( -0.4328386126936296097, 105.9953805924852333, 5.278113798800131207 ) ) ;
#6391 = CARTESIAN_POINT ( 'NONE',  ( -30.15642192025596202, 71.36377005712995469, 1.523999999999991806 ) ) ;
#6392 = CARTESIAN_POINT ( 'NONE',  ( 4.047044637104031395, 109.8183322527596602, -3.518666775989008677 ) ) ;
#6393 = CARTESIAN_POINT ( 'NONE',  ( -15.77815547270824936, 139.7295799824062499, -1.909820663798255103 ) ) ;
#6394 = CARTESIAN_POINT ( 'NONE',  ( -0.03256023585726924852, 157.9544661776888290, 1.629447346748784664 ) ) ;
#6395 = CARTESIAN_POINT ( 'NONE',  ( -9.795036404550218734, 65.29837086945681790, 1.270000000000003126 ) ) ;
#6396 = CARTESIAN_POINT ( 'NONE',  ( -3.594857975007920814, -7.703025367003809798, -2.923569511714296798 ) ) ;
#6398 = VERTEX_POINT ( 'NONE', #12170 ) ;
#6397 = CARTESIAN_POINT ( 'NONE',  ( 0.9591953284561349768, 116.7682604261274264, 0.2970936445032630879 ) ) ;
#6399 = DIRECTION ( 'NONE',  ( 0.01731298258488073519, -0.9998501190848635423, 1.788962107505278613E-16 ) ) ;
#6400 = CARTESIAN_POINT ( 'NONE',  ( 2.813987013336220144, -15.51818976969260255, 4.585835125202748053 ) ) ;
#6401 = TOROIDAL_SURFACE ( 'NONE', #18632, 3.111499999999999488, 0.2540000000000000036 ) ;
#6402 = CARTESIAN_POINT ( 'NONE',  ( -17.77426102521102536, 149.9241642446907292, 1.728420094174573318 ) ) ;
#6403 = CARTESIAN_POINT ( 'NONE',  ( -0.9660709935815289251, 7.903159174923253261, 0.1333004412508401459 ) ) ;
#6404 = EDGE_CURVE ( 'NONE', #10059, #25746, #24513, .T. ) ;
#6405 = CARTESIAN_POINT ( 'NONE',  ( -0.08510646190747463147, 11.08924109716144280, -0.9717149503703566005 ) ) ;
#6406 = ORIENTED_EDGE ( 'NONE', *, *, #20468, .T. ) ;
#6407 = VERTEX_POINT ( 'NONE', #8980 ) ;
#6408 = CARTESIAN_POINT ( 'NONE',  ( -41.41491986784954804, 22.70581808553406233, -4.778348942345147220E-15 ) ) ;
#6409 = CARTESIAN_POINT ( 'NONE',  ( 4.819599041176311438, 120.7138498849978987, 0.4051376471031730708 ) ) ;
#6410 = CARTESIAN_POINT ( 'NONE',  ( -0.01596947694136538129, 156.4635559983122448, 0.7991779281049289363 ) ) ;
#6411 = CARTESIAN_POINT ( 'NONE',  ( 3.231995002093183800, -14.34039573884512997, 4.866605245980782257 ) ) ;
#6412 = CARTESIAN_POINT ( 'NONE',  ( 7.412650754288764077, 120.7277362223577768, -0.9451843054385554721 ) ) ;
#6413 = AXIS2_PLACEMENT_3D ( 'NONE', #9612, #22581, #9822 ) ;
#6414 = CARTESIAN_POINT ( 'NONE',  ( -19.09066119453658317, 140.9752145814059645, -2.516632075137498870 ) ) ;
#6415 = DIRECTION ( 'NONE',  ( -0.8745520943968383420, 0.4849315768086291945, -4.268512490100416826E-16 ) ) ;
#6416 = CARTESIAN_POINT ( 'NONE',  ( 8.212088287371502204, 120.4194928741279256, 1.432818887811018405 ) ) ;
#6417 = CARTESIAN_POINT ( 'NONE',  ( -1.123920628080118167, 36.51502492732748095, 0.1267022063819566724 ) ) ;
#6418 = CARTESIAN_POINT ( 'NONE',  ( 9.747124062405188027, 124.8671652961716489, -0.04776528062357090348 ) ) ;
#6419 = ORIENTED_EDGE ( 'NONE', *, *, #34237, .F. ) ;
#6420 = DIRECTION ( 'NONE',  ( 0.8745520943968243532, -0.4849315768086547296, 6.829619984160642269E-16 ) ) ;
#6421 = CARTESIAN_POINT ( 'NONE',  ( 14.73199999999999932, 12.96416000000000146, 0.000000000000000000 ) ) ;
#6422 = CARTESIAN_POINT ( 'NONE',  ( 4.988558773217932618, 117.5914558864278519, -0.6981965400864760252 ) ) ;
#6423 = CARTESIAN_POINT ( 'NONE',  ( 12.48065534322204151, 152.0704867801853766, 1.458211671286262057 ) ) ;
#6424 = CARTESIAN_POINT ( 'NONE',  ( -7.994219716368544226, 68.36415334912796027, 1.524000000000003796 ) ) ;
#6425 = CARTESIAN_POINT ( 'NONE',  ( 10.82496502431732210, 157.9086237439880733, 0.1564342443379709291 ) ) ;
#6426 = CARTESIAN_POINT ( 'NONE',  ( -0.8805184999823391090, 105.9455060897651748, 5.280965183963572507 ) ) ;
#6427 = DIRECTION ( 'NONE',  ( 1.000000000000000000, -9.466894658874049451E-17, 0.000000000000000000 ) ) ;
#6428 = CARTESIAN_POINT ( 'NONE',  ( 12.69999999999999929, 14.60500000000000043, 0.000000000000000000 ) ) ;
#6429 = CARTESIAN_POINT ( 'NONE',  ( -4.273992351614648300, 31.99305554651359174, 0.5394102745547180167 ) ) ;
#6430 = CARTESIAN_POINT ( 'NONE',  ( 13.36424875645652932, 155.6061939908119882, 2.069718186823302108 ) ) ;
#6431 = CARTESIAN_POINT ( 'NONE',  ( 0.1277143096572389558, 15.67076514537015974, -4.628409624684062251 ) ) ;
#6432 = CARTESIAN_POINT ( 'NONE',  ( -2.078203845413400863, -12.60517393744602721, -8.197436486331740824 ) ) ;
#6433 = CARTESIAN_POINT ( 'NONE',  ( 8.743324216112098313, 118.0100196136648236, -0.4276613644598801223 ) ) ;
#6434 = CARTESIAN_POINT ( 'NONE',  ( -0.7422006451358510448, 119.7070660435176279, -0.6877902101425065196 ) ) ;
#6435 = PLANE ( 'NONE',  #5367 ) ;
#6436 = CARTESIAN_POINT ( 'NONE',  ( 0.6265181353984804469, 106.0244491581631223, -5.258298658868172382 ) ) ;
#6437 = CARTESIAN_POINT ( 'NONE',  ( -1.776898248692639903, 105.1238429332592688, 5.030869823623774550 ) ) ;
#6438 = CARTESIAN_POINT ( 'NONE',  ( -3.562413952978887632, 23.18266144714348798, 2.948169924785601470 ) ) ;
#6439 = CARTESIAN_POINT ( 'NONE',  ( -27.82636559844506152, 59.51700088791086074, 1.523999999999995136 ) ) ;
#6440 = DIRECTION ( 'NONE',  ( -1.000000000000000000, 0.000000000000000000, 0.000000000000000000 ) ) ;
#6441 = CARTESIAN_POINT ( 'NONE',  ( 2.994295736468014280, -14.77441112906794984, 3.968895097548184037 ) ) ;
#6442 = CARTESIAN_POINT ( 'NONE',  ( 1.600813358578667245, 118.7759820277219944, -0.7642889039740424773 ) ) ;
#6443 = CARTESIAN_POINT ( 'NONE',  ( -3.828842504638848787, 116.8938343318378088, 0.2916468201809274130 ) ) ;
#6444 = ORIENTED_EDGE ( 'NONE', *, *, #25155, .T. ) ;
#6445 = CARTESIAN_POINT ( 'NONE',  ( -29.94429436251954613, 71.80236127745905605, -1.270000000000007345 ) ) ;
#6446 = EDGE_CURVE ( 'NONE', #24827, #25703, #31076, .T. ) ;
#6447 = ORIENTED_EDGE ( 'NONE', *, *, #27512, .F. ) ;
#6448 = CYLINDRICAL_SURFACE ( 'NONE', #28786, 0.6349999999999966782 ) ;
#6449 = CARTESIAN_POINT ( 'NONE',  ( 4.647714231081432779, -15.48178215826023774, 3.998406189266252131 ) ) ;
#6450 = CARTESIAN_POINT ( 'NONE',  ( -12.47042458399958953, 121.5863879130357503, 1.220378502515000019 ) ) ;
#6451 = CARTESIAN_POINT ( 'NONE',  ( 21.51971352461169573, 150.2128557559047692, -1.148904605754655250 ) ) ;
#6452 = EDGE_CURVE ( 'NONE', #36699, #16976, #38569, .T. ) ;
#6453 = CARTESIAN_POINT ( 'NONE',  ( 1.968029828064305153, -3.592386099649644837, 4.203610184747879508 ) ) ;
#6454 = CARTESIAN_POINT ( 'NONE',  ( -58.17661517772558000, 0.6798812134844969268, -1.164281364473555236 ) ) ;
#6455 = VERTEX_POINT ( 'NONE', #34343 ) ;
#6456 = CARTESIAN_POINT ( 'NONE',  ( -58.33447198145992729, -0.2173903971933038859, -0.2351149084157238001 ) ) ;
#6457 = CARTESIAN_POINT ( 'NONE',  ( -0.08519874065850288614, 108.5751225745497948, 4.263693374914160117 ) ) ;
#6458 = CARTESIAN_POINT ( 'NONE',  ( 4.756911902486301358, 117.3993836135862949, 1.207145067066230038 ) ) ;
#6459 = CARTESIAN_POINT ( 'NONE',  ( -10.84737219364650329, 123.3109526380878833, 1.071866780254096208 ) ) ;
#6460 = CARTESIAN_POINT ( 'NONE',  ( -30.75918919842648336, 69.77432548395512413, -1.524000000000007793 ) ) ;
#6461 = CARTESIAN_POINT ( 'NONE',  ( 18.75354316333441673, 144.8948545501563103, -1.742436930347202040 ) ) ;
#6462 = CARTESIAN_POINT ( 'NONE',  ( -20.49864673575787677, 149.5144255282053223, -2.384675166241297273 ) ) ;
#6463 = CARTESIAN_POINT ( 'NONE',  ( -58.37241122568488549, -0.2962816677227753104, -1.034007718770489626E-14 ) ) ;
#6464 = VERTEX_POINT ( 'NONE', #40940 ) ;
#6465 = CARTESIAN_POINT ( 'NONE',  ( 4.569713780653100521, 118.0880689344100034, -0.5677796928598370929 ) ) ;
#6466 = CARTESIAN_POINT ( 'NONE',  ( 7.714568708787782114, 122.2455405838764335, -0.3552802434219701211 ) ) ;
#6467 = VERTEX_POINT ( 'NONE', #41578 ) ;
#6468 = CARTESIAN_POINT ( 'NONE',  ( -13.78929608597947620, 128.5353789189983900, -1.909663635655581393 ) ) ;
#6469 = CARTESIAN_POINT ( 'NONE',  ( 3.885732391871624447, -15.29168275415018741, 1.106840230638412192 ) ) ;
#6470 = DIRECTION ( 'NONE',  ( 4.017660918040594346E-17, -1.000000000000000000, -2.376309959284834438E-19 ) ) ;
#6471 = CARTESIAN_POINT ( 'NONE',  ( 18.35410564743290962, 77.35382415001784295, -1.904999999999999583 ) ) ;
#6472 = CARTESIAN_POINT ( 'NONE',  ( -4.805526376074356953, 117.7656062655381675, 0.8575794806940943982 ) ) ;
#6473 = CARTESIAN_POINT ( 'NONE',  ( -0.008945177888024442511, 119.9096241394016715, 0.4476532798976759486 ) ) ;
#6474 = CARTESIAN_POINT ( 'NONE',  ( -46.48504882798792437, 25.86691234155606267, 1.523999999999993804 ) ) ;
#6475 = CARTESIAN_POINT ( 'NONE',  ( -2.201963191602333225, 30.07953629247752758, -4.075912811544394998 ) ) ;
#6476 = CARTESIAN_POINT ( 'NONE',  ( 14.23422759389726977, 138.9464670490549452, 0.5149110934774582260 ) ) ;
#6477 = CARTESIAN_POINT ( 'NONE',  ( -17.14500000000466784, 71.11999999999886768, 1.269999999999998241 ) ) ;
#6479 = ORIENTED_EDGE ( 'NONE', *, *, #11106, .T. ) ;
#6478 = CARTESIAN_POINT ( 'NONE',  ( -46.29506748884625011, 20.38262349295737152, -4.279265904994571379 ) ) ;
#6480 = LINE ( 'NONE', #17102, #25058 ) ;
#6481 = CARTESIAN_POINT ( 'NONE',  ( -28.92060043785469503, 77.33101988233063651, -1.270000000000007789 ) ) ;
#6482 = DIRECTION ( 'NONE',  ( 4.017660918040594346E-17, -1.000000000000000000, -2.376309959284834438E-19 ) ) ;
#6483 = DIRECTION ( 'NONE',  ( -0.1565721916417901483, -0.9876665170007974393, 0.000000000000000000 ) ) ;
#6484 = DIRECTION ( 'NONE',  ( 1.011795553208986377E-16, 1.000000000000000000, -0.000000000000000000 ) ) ;
#6485 = CARTESIAN_POINT ( 'NONE',  ( -55.24575511360199442, 11.19612964283759560, -1.042979010729945558E-14 ) ) ;
#6486 = CARTESIAN_POINT ( 'NONE',  ( -56.71132732703541990, 3.319205314284062958, 2.191228219141345246 ) ) ;
#6487 = CARTESIAN_POINT ( 'NONE',  ( -23.39020171064290210, 146.7932648766621639, -0.1331748977937666500 ) ) ;
#6488 = ORIENTED_EDGE ( 'NONE', *, *, #35842, .T. ) ;
#6489 = CARTESIAN_POINT ( 'NONE',  ( -55.59033409382031721, 8.645621179197947370, -1.431546819705167284 ) ) ;
#6490 = CARTESIAN_POINT ( 'NONE',  ( -6.948590427472591813, 121.9371117883950006, -0.2862137248287923152 ) ) ;
#6491 = ORIENTED_EDGE ( 'NONE', *, *, #28031, .T. ) ;
#6492 = CARTESIAN_POINT ( 'NONE',  ( 1.039317103187317404, 115.7029401488263147, -1.708817239941311295 ) ) ;
#6493 = CARTESIAN_POINT ( 'NONE',  ( -15.73804366022566548, 146.9052959264698757, -0.5443085878246288756 ) ) ;
#6494 = CARTESIAN_POINT ( 'NONE',  ( 5.936869294410564990, -12.97241973064336484, 1.608696005067407953 ) ) ;
#6495 = CARTESIAN_POINT ( 'NONE',  ( -7.954494586186919847, 118.5968412048868288, 0.8561882949445159818 ) ) ;
#6496 = CARTESIAN_POINT ( 'NONE',  ( -5.152689475313444234, 116.8412042432202185, -0.1029630068797482562 ) ) ;
#6497 = CARTESIAN_POINT ( 'NONE',  ( 22.62002883431060596, 150.6357905964555925, 0.7802727354960533601 ) ) ;
#6498 = CARTESIAN_POINT ( 'NONE',  ( 9.460061892327653155, 124.7787809139916106, 0.2814990181333890118 ) ) ;
#6499 = CARTESIAN_POINT ( 'NONE',  ( 4.765531619307481925, 118.5266822147775940, -0.8412287920200557378 ) ) ;
#6500 = CARTESIAN_POINT ( 'NONE',  ( 0.05603342037570913786, 10.86776798020533086, -0.9749832093204870986 ) ) ;
#6501 = CARTESIAN_POINT ( 'NONE',  ( -21.54627550604365638, 132.6250929350426020, -0.6335863061179134448 ) ) ;
#6502 = CARTESIAN_POINT ( 'NONE',  ( 14.39766717389552220, 60.02151067229126369, 1.904999999999990923 ) ) ;
#6503 = EDGE_CURVE ( 'NONE', #40008, #34211, #3667, .T. ) ;
#6504 = DIRECTION ( 'NONE',  ( 0.1565721916418034709, 0.9876665170007954409, -8.659954811667512579E-17 ) ) ;
#6505 = ORIENTED_EDGE ( 'NONE', *, *, #37792, .F. ) ;
#6506 = AXIS2_PLACEMENT_3D ( 'NONE', #26986, #10788, #3583 ) ;
#6507 = CARTESIAN_POINT ( 'NONE',  ( 8.685978770867098575, 118.1606796386214455, 0.8960457658865661479 ) ) ;
#6508 = VERTEX_POINT ( 'NONE', #21734 ) ;
#6509 = CARTESIAN_POINT ( 'NONE',  ( -23.69188486464780752, 78.08202335040543574, -1.270000000000005347 ) ) ;
#6510 = CARTESIAN_POINT ( 'NONE',  ( 9.779442063456341927, 157.5983698538113629, 1.672576317993901496 ) ) ;
#6511 = CARTESIAN_POINT ( 'NONE',  ( 11.29660330931799450, 121.3367100885591015, -1.243740200939188911 ) ) ;
#6512 = CARTESIAN_POINT ( 'NONE',  ( 0.9749890475506259868, 2.950361319068162569, -0.03356295239053608964 ) ) ;
#6513 = CARTESIAN_POINT ( 'NONE',  ( -2.748994976520039213, 10.49642266832308124, 7.958378898918418543 ) ) ;
#6514 = CARTESIAN_POINT ( 'NONE',  ( -15.42726980375961965, 123.0316835747794642, -1.591438994230370829 ) ) ;
#6515 = CARTESIAN_POINT ( 'NONE',  ( 4.662377642780485942, 117.9838022724669457, -0.7074655422033281349 ) ) ;
#6516 = CARTESIAN_POINT ( 'NONE',  ( 1.987587706212191385, 106.6795586461009009, 4.969950645211479667 ) ) ;
#6517 = CARTESIAN_POINT ( 'NONE',  ( -4.599243292695419427, 121.2024757821991159, -0.09190382657876447481 ) ) ;
#6518 = VERTEX_POINT ( 'NONE', #38166 ) ;
#6519 = CARTESIAN_POINT ( 'NONE',  ( -18.35995883219828073, 144.7751241387205425, -2.452750363274776468 ) ) ;
#6520 = CARTESIAN_POINT ( 'NONE',  ( 5.215289103204772125, -15.32183344268082870, 2.967178555186370303 ) ) ;
#6521 = FACE_OUTER_BOUND ( 'NONE', #23576, .T. ) ;
#6522 = CARTESIAN_POINT ( 'NONE',  ( -46.81005371095109524, 25.73327194510133253, -1.583310528698488984 ) ) ;
#6523 = ORIENTED_EDGE ( 'NONE', *, *, #27979, .T. ) ;
#6524 = CARTESIAN_POINT ( 'NONE',  ( 5.554730375462953340, 156.7050554705274408, 1.852363956736410744 ) ) ;
#6525 = DIRECTION ( 'NONE',  ( 0.4849315768086535638, 0.8745520943968251304, 1.030032898892975065E-16 ) ) ;
#6526 = CARTESIAN_POINT ( 'NONE',  ( -17.31000046771894318, 62.32679794340116786, -1.523999999999999577 ) ) ;
#6527 = CARTESIAN_POINT ( 'NONE',  ( -4.418733742721505209, 119.2572634999566930, 0.4175613206465203509 ) ) ;
#6528 = CARTESIAN_POINT ( 'NONE',  ( -8.293629857537270667, 31.38027257336059250, -1.381021427861755635 ) ) ;
#6529 = CARTESIAN_POINT ( 'NONE',  ( 15.96686920080697725, 146.6619865182943272, 1.046663894505766912 ) ) ;
#6530 = AXIS2_PLACEMENT_3D ( 'NONE', #20616, #33647, #30429 ) ;
#6531 = CARTESIAN_POINT ( 'NONE',  ( 3.161282452094233975, 159.3671203531505114, -0.6484678655804383407 ) ) ;
#6532 = EDGE_CURVE ( 'NONE', #27477, #19390, #27672, .T. ) ;
#6533 = CARTESIAN_POINT ( 'NONE',  ( 5.317570146058844038, 115.7029491485453150, -0.5111954518035258799 ) ) ;
#6534 = DIRECTION ( 'NONE',  ( 0.9454731675810360558, -0.3256999990547780888, 5.459396135145339171E-16 ) ) ;
#6535 = PRODUCT_DEFINITION_CONTEXT ( 'detailed design', #25946, 'design' ) ;
#6536 = EDGE_CURVE ( 'NONE', #40785, #9160, #1185, .T. ) ;
#6537 = CARTESIAN_POINT ( 'NONE',  ( -22.53594553814350832, 150.7843406352268687, -0.4248312833800680921 ) ) ;
#6538 = ORIENTED_EDGE ( 'NONE', *, *, #7707, .T. ) ;
#6539 = CARTESIAN_POINT ( 'NONE',  ( 5.026392434963103284, 120.1182786053553002, -0.6754308463122872253 ) ) ;
#6540 = CARTESIAN_POINT ( 'NONE',  ( 4.032974650908811576, -15.19488190071041345, 5.088841723123956662 ) ) ;
#6541 = CARTESIAN_POINT ( 'NONE',  ( -12.24221062544605942, 130.6044139104978115, -0.7866602228194182755 ) ) ;
#6542 = CARTESIAN_POINT ( 'NONE',  ( 2.527534073033691708, -14.76126024938119485, 5.399385249886175409 ) ) ;
#6543 = FACE_OUTER_BOUND ( 'NONE', #11218, .T. ) ;
#6544 = CARTESIAN_POINT ( 'NONE',  ( -0.0002511744761471925336, 116.4254662015457171, 0.01256979787922185565 ) ) ;
#6545 = ADVANCED_FACE ( 'NONE', ( #24735 ), #37737, .T. ) ;
#6546 = VERTEX_POINT ( 'NONE', #2182 ) ;
#6547 = CARTESIAN_POINT ( 'NONE',  ( 1.719524320724281852, 5.915668354077112667, 4.300554535892874064 ) ) ;
#6548 = CARTESIAN_POINT ( 'NONE',  ( 5.140088096925614636, 105.1220910292376800, 1.436521125592880255 ) ) ;
#6549 = CARTESIAN_POINT ( 'NONE',  ( -4.976778051443659479, 117.4086891970763560, 0.8838977329282806661 ) ) ;
#6550 = DIRECTION ( 'NONE',  ( -5.188838149069472160E-16, 1.699382548006136559E-16, 1.000000000000000000 ) ) ;
#6551 = CARTESIAN_POINT ( 'NONE',  ( -6.107213356235562607, 121.2381221225252830, 0.3743496410843655808 ) ) ;
#6552 = CARTESIAN_POINT ( 'NONE',  ( 4.233688895176465294, 13.94658232072815807, -1.861163356065342001 ) ) ;
#6553 = CARTESIAN_POINT ( 'NONE',  ( 22.22261828963529595, 149.8733841865972920, 1.744734864234219085 ) ) ;
#6554 = DIRECTION ( 'NONE',  ( -0.8745520943968235761, 0.4849315768086558398, -4.268512490100410909E-16 ) ) ;
#6556 = CARTESIAN_POINT ( 'NONE',  ( 7.892561109811804698, 118.8455990504009492, -0.9355921144164880410 ) ) ;
#6555 = CARTESIAN_POINT ( 'NONE',  ( 3.369285701246146569, 109.1383298698278566, 3.951686121084368342 ) ) ;
#6557 = CARTESIAN_POINT ( 'NONE',  ( 4.099978103716023448, 4.450953565018914482, -2.131961072590273343 ) ) ;
#6558 = CARTESIAN_POINT ( 'NONE',  ( -15.38653228232040782, 121.5363848317736739, -1.155577132538254448 ) ) ;
#6559 = TOROIDAL_SURFACE ( 'NONE', #15395, 0.7620000000000000107, 0.2540000000000000036 ) ;
#6560 = EDGE_LOOP ( 'NONE', ( #35466, #6968, #21840, #38731 ) ) ;
#6561 = B_SPLINE_CURVE_WITH_KNOTS ( 'NONE', 3,
 ( #6369, #15936, #12953, #32141, #28932, #41950 ),
 .UNSPECIFIED., .F., .F.,
 ( 4, 2, 4 ),
 ( 0.000000000000000000, 0.5000000000000000000, 1.000000000000000000 ),
 .UNSPECIFIED. ) ;
#6562 = EDGE_CURVE ( 'NONE', #13695, #23403, #28570, .T. ) ;
#6563 = AXIS2_PLACEMENT_3D ( 'NONE', #9056, #22021, #38659 ) ;
#6564 = CARTESIAN_POINT ( 'NONE',  ( -3.712124141557985979, 121.0264708767875561, 0.07522066808841054719 ) ) ;
#6565 = VECTOR ( 'NONE', #2140, 1000.000000000000227 ) ;
#6566 = CARTESIAN_POINT ( 'NONE',  ( 4.852936394019410571, -14.31369683153947747, 4.236952399839363892 ) ) ;
#6567 = CARTESIAN_POINT ( 'NONE',  ( -20.21600168833980149, 80.16988503754176065, -1.524000000000003796 ) ) ;
#6568 = ORIENTED_EDGE ( 'NONE', *, *, #26593, .T. ) ;
#6569 = EDGE_CURVE ( 'NONE', #39307, #38156, #9192, .T. ) ;
#6570 = CARTESIAN_POINT ( 'NONE',  ( 10.57181108402524039, 155.7851685111067184, 2.170362527570921962 ) ) ;
#6571 = DIRECTION ( 'NONE',  ( 0.7284927773988482125, 0.6850534820564830873, 0.000000000000000000 ) ) ;
#6572 = DIRECTION ( 'NONE',  ( -0.9336303900108808840, -0.3582377630124027879, -2.618564950574899336E-15 ) ) ;
#6573 = CARTESIAN_POINT ( 'NONE',  ( -11.30743779403340277, 119.0414093155750379, 0.5171725168954618423 ) ) ;
#6574 = EDGE_CURVE ( 'NONE', #2316, #35792, #37892, .T. ) ;
#6575 = CARTESIAN_POINT ( 'NONE',  ( 6.918378865934368349, 117.2797055272990292, -0.1815168674402108384 ) ) ;
#6576 = CARTESIAN_POINT ( 'NONE',  ( -5.638212235186761845, 57.15000000000000568, -5.060089761242226203 ) ) ;
#6577 = CIRCLE ( 'NONE', #22977, 0.2539999999999942859 ) ;
#6578 = CARTESIAN_POINT ( 'NONE',  ( -46.60530155212503445, 26.17382724835477958, 1.269999999999988916 ) ) ;
#6579 = CARTESIAN_POINT ( 'NONE',  ( 2.407412430484044816E-32, 1.626303258728256651E-15, 0.000000000000000000 ) ) ;
#6580 = CARTESIAN_POINT ( 'NONE',  ( 2.164775582100227247, -15.10189236760869846, 5.710855967119448096 ) ) ;
#6581 = EDGE_CURVE ( 'NONE', #39868, #22781, #3208, .T. ) ;
#6582 = CARTESIAN_POINT ( 'NONE',  ( -43.49527490626578441, 22.26612824116996237, 2.150709692269567874 ) ) ;
#6583 = CARTESIAN_POINT ( 'NONE',  ( -23.16987411132078378, 77.52691185402750307, -1.270000000000004903 ) ) ;
#6584 = CARTESIAN_POINT ( 'NONE',  ( -4.531800530025674512, 118.0871158275990069, 0.6067528179264731758 ) ) ;
#6585 = CARTESIAN_POINT ( 'NONE',  ( -58.37241122568487128, -0.2962816677227753104, -0.2416009568454013656 ) ) ;
#6586 = VECTOR ( 'NONE', #9513, 1000.000000000000000 ) ;
#6587 = ORIENTED_EDGE ( 'NONE', *, *, #21078, .F. ) ;
#6588 = FACE_OUTER_BOUND ( 'NONE', #31664, .T. ) ;
#6589 = CARTESIAN_POINT ( 'NONE',  ( -8.337209054434152833, 119.8086030055221869, -1.438699114785731537 ) ) ;
#6590 = CARTESIAN_POINT ( 'NONE',  ( -5.571761382372367066, 117.9391977826196296, -0.7470240521525300936 ) ) ;
#6591 = CARTESIAN_POINT ( 'NONE',  ( 4.675781884360660001, 117.9791009951701000, 0.8445612169912808387 ) ) ;
#6592 = CARTESIAN_POINT ( 'NONE',  ( 3.047145566129288330, -14.72663143740328806, 3.823360744794035870 ) ) ;
#6593 = CARTESIAN_POINT ( 'NONE',  ( -8.534279067096813165, 122.4751019636825049, -0.9739960529120706978 ) ) ;
#6594 = CARTESIAN_POINT ( 'NONE',  ( -4.800085724567980883, 115.7029491485352537, -1.472342921364584889 ) ) ;
#6595 = CARTESIAN_POINT ( 'NONE',  ( -1.351554245314562586, 106.2775040229277153, 5.112464471456568127 ) ) ;
#6596 = CARTESIAN_POINT ( 'NONE',  ( -4.711190372662979797, 117.8992862897405871, -0.9551895239324142972 ) ) ;
#6597 = CARTESIAN_POINT ( 'NONE',  ( 4.488494058616853799, 111.2667756541687538, -2.954587190001159325 ) ) ;
#6598 = CARTESIAN_POINT ( 'NONE',  ( -11.67499187284231610, 153.3684197651487580, -1.838730530730911861 ) ) ;
#6599 = CARTESIAN_POINT ( 'NONE',  ( -0.02874415600673332558, 157.0795416643300939, 1.438475106415294302 ) ) ;
#6600 = CARTESIAN_POINT ( 'NONE',  ( -3.658134704041837271, 115.7029491485453434, 1.477887315928634759 ) ) ;
#6601 = CARTESIAN_POINT ( 'NONE',  ( -3.781325196301324354, 121.0927823605408662, -0.005689350045973306028 ) ) ;
#6602 = CARTESIAN_POINT ( 'NONE',  ( 0.05711764529616595448, 0.5181683540770933849, -4.631227783250111862 ) ) ;
#6604 = ORIENTED_EDGE ( 'NONE', *, *, #32666, .F. ) ;
#6603 = CARTESIAN_POINT ( 'NONE',  ( 22.11976774214178931, 136.9573810088325843, 1.270382039940954222 ) ) ;
#6605 = DIRECTION ( 'NONE',  ( 0.9998004120163609398, 0.000000000000000000, 0.01997839162482749689 ) ) ;
#6606 = CARTESIAN_POINT ( 'NONE',  ( 3.431757876926103012, -15.17734022545018391, 2.935651181724953318 ) ) ;
#6607 = CARTESIAN_POINT ( 'NONE',  ( -11.47069961394323201, 122.2847249198043471, 1.269327653809199985 ) ) ;
#6608 = CARTESIAN_POINT ( 'NONE',  ( 0.3177745610913299545, 14.38516025884261929, -0.9235644396001725376 ) ) ;
#6609 = CIRCLE ( 'NONE', #30402, 0.6350000000000006750 ) ;
#6610 = CARTESIAN_POINT ( 'NONE',  ( -23.16247218334359559, 146.6831645211815101, -1.199661776592803264 ) ) ;
#6611 = AXIS2_PLACEMENT_3D ( 'NONE', #39520, #3747, #13526 ) ;
#6612 = CARTESIAN_POINT ( 'NONE',  ( -0.7366970693195243891, 2.667464547469879488, -0.6395729927624468347 ) ) ;
#6613 = ORIENTED_EDGE ( 'NONE', *, *, #10010, .F. ) ;
#6614 = ORIENTED_EDGE ( 'NONE', *, *, #37079, .F. ) ;
#6615 = CARTESIAN_POINT ( 'NONE',  ( -42.04356058215219605, 22.06167541775167606, 0.4953331422233907544 ) ) ;
#6616 = CARTESIAN_POINT ( 'NONE',  ( 1.966029823418392608, 106.7001829816230725, 4.962286218837188123 ) ) ;
#6617 = CARTESIAN_POINT ( 'NONE',  ( 0.000000000000000000, 0.000000000000000000, 0.000000000000000000 ) ) ;
#6618 = CARTESIAN_POINT ( 'NONE',  ( -15.06908741399251817, 148.9283877096812034, 0.6536164350837786463 ) ) ;
#6619 = CARTESIAN_POINT ( 'NONE',  ( 3.464659682708206123, -14.15734315221130224, 4.609430909834149048 ) ) ;
#6620 = CARTESIAN_POINT ( 'NONE',  ( 17.55799248491146614, 146.4615580561186050, -1.465990265564338646 ) ) ;
#6621 =( GEOMETRIC_REPRESENTATION_CONTEXT ( 3 ) GLOBAL_UNCERTAINTY_ASSIGNED_CONTEXT ( ( #39338 ) ) GLOBAL_UNIT_ASSIGNED_CONTEXT ( ( #25692, #25899, #6740 ) ) REPRESENTATION_CONTEXT ( 'NONE', 'WORKASPACE' ) );
#6622 = CARTESIAN_POINT ( 'NONE',  ( -4.132678194918598003, 118.9132445967212419, -1.007338114003851315 ) ) ;
#6623 = CARTESIAN_POINT ( 'NONE',  ( -47.87720502863936645, 19.40776447661573911, -5.264800451520500246 ) ) ;
#6624 = CARTESIAN_POINT ( 'NONE',  ( 8.261346106638972842, 120.1775813921023399, 1.448714831781537260 ) ) ;
#6625 = CARTESIAN_POINT ( 'NONE',  ( -5.231323785280036276, 32.40695963756544273, 1.837218211224142861 ) ) ;
#6626 = B_SPLINE_CURVE_WITH_KNOTS ( 'NONE', 3,
 ( #4421, #35573, #6596, #219, #26976, #38974 ),
 .UNSPECIFIED., .F., .F.,
 ( 4, 2, 4 ),
 ( 0.000000000000000000, 0.0001566688501089290775, 0.0003133377002178581549 ),
 .UNSPECIFIED. ) ;
#6627 = CARTESIAN_POINT ( 'NONE',  ( 2.792630161979468006, 120.9517662584847102, -0.08501465617163896094 ) ) ;
#6628 = ADVANCED_FACE ( 'NONE', ( #37949 ), #23580, .T. ) ;
#6629 = AXIS2_PLACEMENT_3D ( 'NONE', #28429, #25017, #30985 ) ;
#6630 = ORIENTED_EDGE ( 'NONE', *, *, #40223, .F. ) ;
#6631 = CARTESIAN_POINT ( 'NONE',  ( -0.1064799869811820787, 105.7853621660184444, 5.332934571178567396 ) ) ;
#6632 = LINE ( 'NONE', #36237, #40900 ) ;
#6633 = CARTESIAN_POINT ( 'NONE',  ( -58.65598178207972779, -0.3163282088989305407, 0.3245478190976838206 ) ) ;
#6634 = DIRECTION ( 'NONE',  ( 0.9734199927291312671, 0.2290273297124563179, 2.762079339012820083E-15 ) ) ;
#6635 = CARTESIAN_POINT ( 'NONE',  ( 18.62524206359421086, 154.1412379532633850, 0.2279367985168735955 ) ) ;
#6636 = EDGE_CURVE ( 'NONE', #14176, #37301, #34756, .T. ) ;
#6637 = CARTESIAN_POINT ( 'NONE',  ( -6.519249125050614602, 120.6419738463991536, 0.1350556763279783523 ) ) ;
#6638 = CIRCLE ( 'NONE', #12072, 3.175000000000001155 ) ;
#6639 = EDGE_CURVE ( 'NONE', #16922, #6508, #18546, .T. ) ;
#6640 = CARTESIAN_POINT ( 'NONE',  ( -3.259680568650582977, 115.6909491485508852, 1.531580627320187293 ) ) ;
#6641 = CARTESIAN_POINT ( 'NONE',  ( 2.862861873098513588, -10.07698056833738320, -3.640125809621840069 ) ) ;
#6642 = CARTESIAN_POINT ( 'NONE',  ( -5.212520885064538589, 31.45212241211192605, -0.4657032193360505778 ) ) ;
#6643 = CARTESIAN_POINT ( 'NONE',  ( 6.769736154946609297, 118.6475953829349379, 1.187203428762516388 ) ) ;
#6644 = CARTESIAN_POINT ( 'NONE',  ( 2.551181839206869917, 14.82117702134586779, -3.857898856385788999 ) ) ;
#6645 = CARTESIAN_POINT ( 'NONE',  ( 6.556273983038449771, -14.34328088419217728, -5.323198733142235461 ) ) ;
#6646 = CARTESIAN_POINT ( 'NONE',  ( -8.731353435635694993, 117.9558915041894522, -0.7268751822057367695 ) ) ;
#6647 = CARTESIAN_POINT ( 'NONE',  ( -0.2286055872010028245, 108.3383513567250986, -4.353007566726654787 ) ) ;
#6648 = CARTESIAN_POINT ( 'NONE',  ( -23.36121599383904623, 148.8756354987168606, -0.4668126921610641911 ) ) ;
#6649 = CARTESIAN_POINT ( 'NONE',  ( 3.222817655156935412, 108.4800784852299955, -4.089130794945939229 ) ) ;
#6650 = CARTESIAN_POINT ( 'NONE',  ( -2.420033166307097972, 104.6144662015456959, 4.756650020785883726 ) ) ;
#6651 = CARTESIAN_POINT ( 'NONE',  ( -4.460028654926622593, 22.53297844546955631, 1.214995109042491528 ) ) ;
#6652 = FACE_OUTER_BOUND ( 'NONE', #30275, .T. ) ;
#6653 = FACE_OUTER_BOUND ( 'NONE', #23340, .T. ) ;
#6654 = CARTESIAN_POINT ( 'NONE',  ( 3.162791966164926638, -14.44121541014482801, 3.416220915275241854 ) ) ;
#6655 = CARTESIAN_POINT ( 'NONE',  ( 2.219425127536471809, 123.7320667226965867, -0.04105829392232412944 ) ) ;
#6656 = CARTESIAN_POINT ( 'NONE',  ( -16.70010949199491179, 122.7093839631038463, 0.3053630257279365545 ) ) ;
#6657 = VECTOR ( 'NONE', #12141, 1000.000000000000000 ) ;
#6658 = EDGE_LOOP ( 'NONE', ( #13680, #4709, #27962, #14755 ) ) ;
#6659 = CARTESIAN_POINT ( 'NONE',  ( 5.664977208693799504, 88.73331249999999670, 5.033228321271210781 ) ) ;
#6660 = VERTEX_POINT ( 'NONE', #15354 ) ;
#6661 = CARTESIAN_POINT ( 'NONE',  ( -0.7387659178326329013, 32.94979111317254450, 0.8178967711910589689 ) ) ;
#6662 = CARTESIAN_POINT ( 'NONE',  ( 6.000997576644805598, -14.76005184138509740, 0.6970346396957283197 ) ) ;
#6663 = CARTESIAN_POINT ( 'NONE',  ( -11.27973791692654260, 156.1341193432522800, 1.681596738997434892 ) ) ;
#6664 = CARTESIAN_POINT ( 'NONE',  ( 14.51588022701130676, 121.7426775721902175, -0.9381456983900905433 ) ) ;
#6665 = CARTESIAN_POINT ( 'NONE',  ( 3.746277899330032302, -0.8937244826341392834, -2.755274729908455900 ) ) ;
#6666 = CARTESIAN_POINT ( 'NONE',  ( -58.61347569670156332, -0.2600004252125417414, -0.4230615130465681939 ) ) ;
#6667 = ORIENTED_EDGE ( 'NONE', *, *, #2714, .F. ) ;
#6668 = CARTESIAN_POINT ( 'NONE',  ( 5.078986093043053707, 85.18346620154574111, 0.1014902294541244060 ) ) ;
#6669 = CARTESIAN_POINT ( 'NONE',  ( 0.3746108773302438966, 122.5569158606515003, 0.2627672029693577382 ) ) ;
#6670 = CARTESIAN_POINT ( 'NONE',  ( 0.000000000000000000, 0.000000000000000000, 0.000000000000000000 ) ) ;
#6671 = CARTESIAN_POINT ( 'NONE',  ( -9.584070499013474631, 122.7780075402122151, 0.8664194973949997935 ) ) ;
#6672 = CARTESIAN_POINT ( 'NONE',  ( -8.210443557797230341, 69.68696903609419735, 1.270000000000003348 ) ) ;
#6673 = CARTESIAN_POINT ( 'NONE',  ( 5.067974813687860625, 119.5555251685854330, -0.8659238720033421988 ) ) ;
#6674 = CARTESIAN_POINT ( 'NONE',  ( -19.44881300980853922, 136.0480396440595996, -2.307899331309747559 ) ) ;
#6675 = CARTESIAN_POINT ( 'NONE',  ( -57.24023649071029496, 3.661034843983918208, -2.195083147259570211 ) ) ;
#6676 = ORIENTED_EDGE ( 'NONE', *, *, #2235, .F. ) ;
#6677 = CARTESIAN_POINT ( 'NONE',  ( 4.496309931980947638, 118.1299276439104631, -0.5226211628217811711 ) ) ;
#6678 = CARTESIAN_POINT ( 'NONE',  ( 15.94526953466029973, 147.3275361421020193, -0.5311500221062649407 ) ) ;
#6679 = ORIENTED_EDGE ( 'NONE', *, *, #22807, .T. ) ;
#6680 = CARTESIAN_POINT ( 'NONE',  ( -17.64033768477188246, 147.6919162452172145, -2.236185705752640196 ) ) ;
#6681 = CARTESIAN_POINT ( 'NONE',  ( 2.294714809908028119, -15.51018114022951977, 5.078884642465592236 ) ) ;
#6682 = CARTESIAN_POINT ( 'NONE',  ( 3.682264917456193665, 66.13346620154572975, 0.07358041635424013294 ) ) ;
#6683 = CARTESIAN_POINT ( 'NONE',  ( 8.515285667870289099E-16, 8.844871939465425825, 0.000000000000000000 ) ) ;
#6684 = CARTESIAN_POINT ( 'NONE',  ( -4.746868605287419385, 117.7551308511543198, 0.8963948101134247004 ) ) ;
#6685 = CARTESIAN_POINT ( 'NONE',  ( 13.52836484031751496, 128.5255724691869830, 1.838026323690954422 ) ) ;
#6686 = CARTESIAN_POINT ( 'NONE',  ( -2.190119082386309035, 30.63587144615187086, 1.931548619664235522 ) ) ;
#6687 = EDGE_CURVE ( 'NONE', #34378, #25039, #2607, .T. ) ;
#6688 = CARTESIAN_POINT ( 'NONE',  ( 2.598967704003971146, -9.625211180298204994, -8.041545772114961466 ) ) ;
#6689 = CARTESIAN_POINT ( 'NONE',  ( 0.6475778113725148000, 156.3069099058775748, 0.1429049811405687098 ) ) ;
#6690 = CARTESIAN_POINT ( 'NONE',  ( -28.69846420587789737, 77.20784726182124302, -1.524000000000007793 ) ) ;
#6691 = CARTESIAN_POINT ( 'NONE',  ( -48.74330358230356808, 18.21177412086844072, -5.147861347727202386 ) ) ;
#6692 = CARTESIAN_POINT ( 'NONE',  ( 2.185739921021631726, 116.1876150569675730, -0.001408202639197844719 ) ) ;
#6693 = CARTESIAN_POINT ( 'NONE',  ( -4.017108196799733300, 117.3993836135118158, 1.174877857344739596 ) ) ;
#6694 = CARTESIAN_POINT ( 'NONE',  ( -46.75070351170987237, 25.87126803027572564, -1.402526684451548267 ) ) ;
#6695 = CARTESIAN_POINT ( 'NONE',  ( 3.174366308151880922, 104.6144662015457243, 0.06343139340882769650 ) ) ;
#6696 = DIRECTION ( 'NONE',  ( 0.9998004120163608288, 0.000000000000000000, 0.01997839162482760791 ) ) ;
#6697 = CARTESIAN_POINT ( 'NONE',  ( -5.177913976931305839, 88.73331249999998249, 5.372100000000000541 ) ) ;
#6698 = CARTESIAN_POINT ( 'NONE',  ( 5.078986093043053707, 87.97746620154572383, 0.1014902294541237954 ) ) ;
#6699 = DIRECTION ( 'NONE',  ( -0.8745520943968240202, 0.4849315768086553402, -5.361993529360572958E-16 ) ) ;
#6700 = CARTESIAN_POINT ( 'NONE',  ( -57.73934301000005576, 2.737667398473711433, 1.050169850737047383 ) ) ;
#6701 = CARTESIAN_POINT ( 'NONE',  ( -58.23017998949752183, 0.6774554162835566551, 1.209604144815701554 ) ) ;
#6702 = CARTESIAN_POINT ( 'NONE',  ( -17.11470313646614727, 122.7072422303320707, -0.09880859551014491149 ) ) ;
#6703 = ORIENTED_EDGE ( 'NONE', *, *, #36211, .T. ) ;
#6704 = CARTESIAN_POINT ( 'NONE',  ( -50.15972161391663064, 17.13814111569222121, -4.955022299345084313 ) ) ;
#6705 = CARTESIAN_POINT ( 'NONE',  ( -6.048481876759730369, 121.4346570564865857, -0.1338841272842773988 ) ) ;
#6706 = AXIS2_PLACEMENT_3D ( 'NONE', #13070, #39920, #26060 ) ;
#6707 = ORIENTED_EDGE ( 'NONE', *, *, #20858, .F. ) ;
#6708 = PLANE ( 'NONE',  #30775 ) ;
#6709 = CARTESIAN_POINT ( 'NONE',  ( -7.044165191775566548, 122.0728772437221323, -0.1705051815768210965 ) ) ;
#6710 = CARTESIAN_POINT ( 'NONE',  ( 3.428369065731536658, -15.18705194980916851, 5.515041984116586526 ) ) ;
#6711 = CARTESIAN_POINT ( 'NONE',  ( -21.08161885447505313, 149.3892802667211868, 1.460526482899864531 ) ) ;
#6712 = CARTESIAN_POINT ( 'NONE',  ( 8.196043946343802844, 117.5568930537867800, 0.4237257472399769131 ) ) ;
#6713 = CARTESIAN_POINT ( 'NONE',  ( 0.6484723942714255562, 120.9972571750055579, 0.07908818383241446315 ) ) ;
#6714 = FACE_OUTER_BOUND ( 'NONE', #18886, .T. ) ;
#6715 = CARTESIAN_POINT ( 'NONE',  ( -0.7518944845272079736, 4.819152178039351142, 0.6255420797857809134 ) ) ;
#6716 = CARTESIAN_POINT ( 'NONE',  ( -22.81319227411009365, 150.4043717142618277, -0.6849243123989297022 ) ) ;
#6717 = CARTESIAN_POINT ( 'NONE',  ( -47.97335965025877869, 19.24887047013930541, -5.222717875959610900 ) ) ;
#6718 = CARTESIAN_POINT ( 'NONE',  ( -18.63562586887613648, 79.95981838582228818, 1.269999999999996243 ) ) ;
#6719 = ORIENTED_EDGE ( 'NONE', *, *, #34761, .T. ) ;
#6720 = CARTESIAN_POINT ( 'NONE',  ( 8.600551643892799802, 118.5561038629244592, 1.113272402564501995 ) ) ;
#6721 = ORIENTED_EDGE ( 'NONE', *, *, #27207, .F. ) ;
#6722 = CARTESIAN_POINT ( 'NONE',  ( -16.17691485933977091, 135.1141785778430346, 1.596016904437364881 ) ) ;
#6723 = DIRECTION ( 'NONE',  ( -1.000000000000000000, -6.353134868986659519E-16, 0.000000000000000000 ) ) ;
#6724 = CARTESIAN_POINT ( 'NONE',  ( 10.72975491961945593, 119.6772744462923157, 1.366487948980413369 ) ) ;
#6725 = CARTESIAN_POINT ( 'NONE',  ( 12.99265913520512683, 122.2940260782629451, -1.284300974089672920 ) ) ;
#6726 = CARTESIAN_POINT ( 'NONE',  ( 0.5559618826558695437, 1.427253112428326753, 0.7990736944121461516 ) ) ;
#6727 = VECTOR ( 'NONE', #267, 1000.000000000000000 ) ;
#6728 = CARTESIAN_POINT ( 'NONE',  ( -19.51124600060716929, 152.2820370773569323, -1.942483913431541920 ) ) ;
#6729 = CARTESIAN_POINT ( 'NONE',  ( 4.807494110098772921, 117.8776439329783017, -0.6745073813406683438 ) ) ;
#6730 = CARTESIAN_POINT ( 'NONE',  ( 6.733859895263996975, 121.2177056076135528, 0.3428974583126989661 ) ) ;
#6731 = CARTESIAN_POINT ( 'NONE',  ( 9.413719431533399629, 122.9055586947561522, -0.7725895697485186675 ) ) ;
#6732 = CARTESIAN_POINT ( 'NONE',  ( -15.64289809528671071, 147.2198192248932571, -0.2613308799247720526 ) ) ;
#6733 = EDGE_LOOP ( 'NONE', ( #18442, #39213, #1751, #34116 ) ) ;
#6734 = CARTESIAN_POINT ( 'NONE',  ( -2.214684683099673812, 157.4004113605966211, -1.675081295071568110 ) ) ;
#6735 = CARTESIAN_POINT ( 'NONE',  ( 4.376329468599289285, -15.53264713215277126, 4.356271056886698467 ) ) ;
#6736 = DIRECTION ( 'NONE',  ( -0.8572391118119510045, -0.5149185422762100339, -3.573031421855330583E-16 ) ) ;
#6737 = CARTESIAN_POINT ( 'NONE',  ( -48.21404017327530767, 19.06235592689615288, -5.351320745402601275 ) ) ;
#6738 = VERTEX_POINT ( 'NONE', #26204 ) ;
#6739 = CARTESIAN_POINT ( 'NONE',  ( 7.432183457866615051, 120.4750020944285609, 1.305203700904508546 ) ) ;
#6740 =( NAMED_UNIT ( * ) SI_UNIT ( $, .STERADIAN. ) SOLID_ANGLE_UNIT ( ) );
#6741 = AXIS2_PLACEMENT_3D ( 'NONE', #30105, #9873, #39708 ) ;
#6742 = VECTOR ( 'NONE', #39733, 1000.000000000000114 ) ;
#6743 = DIRECTION ( 'NONE',  ( 0.8572391118119522258, 0.5149185422762083686, -1.192944345661028856E-14 ) ) ;
#6744 = CARTESIAN_POINT ( 'NONE',  ( -1.593197492609443433, 110.3135721340718334, 3.506749948187484645 ) ) ;
#6745 = CARTESIAN_POINT ( 'NONE',  ( 7.636339006008190822, 27.50728337528610012, -3.595707551023701765 ) ) ;
#6746 = CARTESIAN_POINT ( 'NONE',  ( 11.59282501421104783, 128.2970750771678752, 0.8590849294959500559 ) ) ;
#6747 = CARTESIAN_POINT ( 'NONE',  ( 22.86776170061652280, 148.6346580502994073, -0.6251136566479097434 ) ) ;
#6748 = CARTESIAN_POINT ( 'NONE',  ( -14.73199999999999754, 61.59499999999999886, 5.016499999999999737 ) ) ;
#6749 = FACE_OUTER_BOUND ( 'NONE', #34102, .T. ) ;
#6750 = CARTESIAN_POINT ( 'NONE',  ( -15.72215902125780751, 120.8394623874526275, -0.2972128523334375272 ) ) ;
#6751 = ORIENTED_EDGE ( 'NONE', *, *, #14101, .F. ) ;
#6752 = CARTESIAN_POINT ( 'NONE',  ( -7.950921552827399985, 121.7269089819065329, -1.084193410159759452 ) ) ;
#6753 = CARTESIAN_POINT ( 'NONE',  ( 22.66375647020927531, 150.6386093215953395, 0.4528757910175285062 ) ) ;
#6754 = CARTESIAN_POINT ( 'NONE',  ( -13.78138926674715314, 150.2278160098252329, -0.9796190600867306086 ) ) ;
#6755 = CARTESIAN_POINT ( 'NONE',  ( 3.821280252649200460, -11.76149679029331274, 0.6556923638117722053 ) ) ;
#6756 = CARTESIAN_POINT ( 'NONE',  ( 14.24929227862422820, 61.25037559889039329, 5.016500000000000625 ) ) ;
#6757 = CARTESIAN_POINT ( 'NONE',  ( 23.41829197008351215, 142.8308675865925181, 0.4933589455792337652 ) ) ;
#6758 = ORIENTED_EDGE ( 'NONE', *, *, #14924, .F. ) ;
#6759 = CARTESIAN_POINT ( 'NONE',  ( -4.636761822055341042, 12.60011390031314349, 0.2095705037016724059 ) ) ;
#6760 = CARTESIAN_POINT ( 'NONE',  ( -4.612917339777265369, 105.1215402076766878, 2.701253017043198312 ) ) ;
#6761 = CARTESIAN_POINT ( 'NONE',  ( -4.855027809809237205, 117.4045417072194226, 0.9983932867329968763 ) ) ;
#6762 = CARTESIAN_POINT ( 'NONE',  ( 16.87828382557106721, 17.14499999999999957, -5.016499999999999737 ) ) ;
#6763 = CARTESIAN_POINT ( 'NONE',  ( -7.930528998391228157, 121.9940456953541741, 0.6366723744063579327 ) ) ;
#6764 = AXIS2_PLACEMENT_3D ( 'NONE', #10714, #27116, #36928 ) ;
#6765 = CARTESIAN_POINT ( 'NONE',  ( -2.065029617914060367, 6.824861272777455135, -4.134893973632223663 ) ) ;
#6766 = CARTESIAN_POINT ( 'NONE',  ( 15.11776246977249905, 121.4505734225448066, 1.235019191190165344 ) ) ;
#6768 = CIRCLE ( 'NONE', #14383, 0.6350000000000006750 ) ;
#6767 = CARTESIAN_POINT ( 'NONE',  ( 15.19943428492308080, 148.1072807477730748, 0.3037208696559882681 ) ) ;
#6770 = CARTESIAN_POINT ( 'NONE',  ( 5.882407806703735531, 118.3130479344264501, -0.8400364453129069986 ) ) ;
#6769 = CARTESIAN_POINT ( 'NONE',  ( -16.60960244842765121, 9.026346327358517385, 0.000000000000000000 ) ) ;
#6771 = CARTESIAN_POINT ( 'NONE',  ( 4.577905313181523717, 13.52175256873284326, -0.6256056815880789435 ) ) ;
#6772 = CARTESIAN_POINT ( 'NONE',  ( -8.098994982418762589, 117.9016134627522945, -0.8176261169560977704 ) ) ;
#6773 = ORIENTED_EDGE ( 'NONE', *, *, #6119, .T. ) ;
#6774 = CARTESIAN_POINT ( 'NONE',  ( -6.491509040565048849, 121.7133186976561205, 0.1169240713195678211 ) ) ;
#6775 = CARTESIAN_POINT ( 'NONE',  ( 3.596007053926196573, -14.96754207850672991, 5.407624617413868684 ) ) ;
#6776 = DIRECTION ( 'NONE',  ( -5.188838149069471174E-16, 1.699382548006136313E-16, 1.000000000000000000 ) ) ;
#6777 = CARTESIAN_POINT ( 'NONE',  ( 3.026662605148213725, -13.87242449132548217, 1.205013440933411228 ) ) ;
#6778 = ORIENTED_EDGE ( 'NONE', *, *, #20866, .F. ) ;
#6779 = CARTESIAN_POINT ( 'NONE',  ( -0.01152893261320977157, 118.7114655739656257, 0.5769549317675699562 ) ) ;
#6780 = CARTESIAN_POINT ( 'NONE',  ( -8.265412277504241345, 72.86149316418863009, 1.270000000000002682 ) ) ;
#6781 = CARTESIAN_POINT ( 'NONE',  ( 3.174366308151880922, 95.34346620154573770, 0.06343139340882768262 ) ) ;
#6782 = CARTESIAN_POINT ( 'NONE',  ( -10.46273137052137336, 157.8855781193960297, 0.6617911890761500882 ) ) ;
#6783 = EDGE_CURVE ( 'NONE', #6518, #38326, #6609, .T. ) ;
#6784 = CARTESIAN_POINT ( 'NONE',  ( -0.5057995593169576365, 15.89392266832286182, -8.404578209849391968 ) ) ;
#6785 = ADVANCED_FACE ( 'NONE', ( #13431 ), #35870, .F. ) ;
#6786 = CARTESIAN_POINT ( 'NONE',  ( 23.22389216488245722, 148.7951734159264561, -0.1326450332456384218 ) ) ;
#6787 = AXIS2_PLACEMENT_3D ( 'NONE', #33807, #17591, #20156 ) ;
#6788 = CARTESIAN_POINT ( 'NONE',  ( -5.638212235253867277, 56.51500000000000767, -5.060089761408552711 ) ) ;
#6789 = CARTESIAN_POINT ( 'NONE',  ( -46.76084739749286712, 25.84593537448104428, 1.416306353842238908 ) ) ;
#6790 = CARTESIAN_POINT ( 'NONE',  ( -47.62964748377234514, 25.45032632311202647, 0.1281092358103023410 ) ) ;
#6791 = CARTESIAN_POINT ( 'NONE',  ( -4.812686597042231895, 117.4055138428619784, -1.197175370899103752 ) ) ;
#6792 = CARTESIAN_POINT ( 'NONE',  ( -56.65231406860745977, 4.194353530936431262, 2.518504496425231221 ) ) ;
#6793 = DIRECTION ( 'NONE',  ( 0.9998004120163608288, 4.016384292689131511E-17, 0.01997839162482749342 ) ) ;
#6794 = CARTESIAN_POINT ( 'NONE',  ( -4.527558639897409698, 118.1161936615429084, 0.5308642384113577695 ) ) ;
#6795 = CARTESIAN_POINT ( 'NONE',  ( -58.35029634831491308, -0.2563984898762833309, -0.1830726351724966949 ) ) ;
#6796 = ORIENTED_EDGE ( 'NONE', *, *, #22369, .T. ) ;
#6797 = VERTEX_POINT ( 'NONE', #6210 ) ;
#6798 = CARTESIAN_POINT ( 'NONE',  ( -1.075895380385707201, 115.6909491485452577, -1.747627985865146227 ) ) ;
#6799 = CARTESIAN_POINT ( 'NONE',  ( 4.019189700197100201, 119.1285266303971753, -0.7637224803080886470 ) ) ;
#6800 = CARTESIAN_POINT ( 'NONE',  ( -7.618479139564731106, 124.7215218652630710, -0.1522353441811850894 ) ) ;
#6801 = CARTESIAN_POINT ( 'NONE',  ( 4.603208726993124777, 118.0397272544194180, 0.8064533428228448653 ) ) ;
#6802 = CARTESIAN_POINT ( 'NONE',  ( -46.86699512455117400, 25.83114541775341522, -0.4845221143632307825 ) ) ;
#6803 = CARTESIAN_POINT ( 'NONE',  ( -14.24959175664888633, 150.3563008155378213, -1.527850727897531291 ) ) ;
#6804 = CARTESIAN_POINT ( 'NONE',  ( 8.936628967501334841, 55.24500000000000455, 4.721553682181185430 ) ) ;
#6805 = DIRECTION ( 'NONE',  ( 1.000000000000000000, -9.627370216492862708E-17, 0.000000000000000000 ) ) ;
#6806 = CARTESIAN_POINT ( 'NONE',  ( 7.475619626241481797, 123.6620266863018855, 0.1149006695610369777 ) ) ;
#6807 = CARTESIAN_POINT ( 'NONE',  ( -16.40533521683946816, 148.4304801786341272, -1.905158959863711088 ) ) ;
#6808 = SURFACE_SIDE_STYLE ('',( #12976 ) ) ;
#6809 = CARTESIAN_POINT ( 'NONE',  ( -0.008148072696648066618, 156.3406798448389168, 0.4077628766201955579 ) ) ;
#6810 = CARTESIAN_POINT ( 'NONE',  ( 8.635102817405984510, 118.5712416014077206, -0.7746300195078601458 ) ) ;
#6811 = CARTESIAN_POINT ( 'NONE',  ( -10.39718957393781551, 153.1349757784973349, -0.1475885461366300277 ) ) ;
#6812 = CARTESIAN_POINT ( 'NONE',  ( 0.09481320634720795393, -4.229605868409334057, 4.636458411128852930 ) ) ;
#6813 = CARTESIAN_POINT ( 'NONE',  ( 20.39753840605626678, 152.5480347002736607, 1.233721349276552637 ) ) ;
#6814 = CARTESIAN_POINT ( 'NONE',  ( -17.14500000000466784, 71.11999999999886768, -1.270000000000000684 ) ) ;
#6815 = CARTESIAN_POINT ( 'NONE',  ( 3.239928030326187258, -14.81799142783181367, -0.3301716407829758948 ) ) ;
#6816 = CARTESIAN_POINT ( 'NONE',  ( -19.29290905409802903, 147.1635184732690220, 1.739861672056419728 ) ) ;
#6817 = CARTESIAN_POINT ( 'NONE',  ( -0.9360807938713975318, 7.254031735439380846, -0.2770855581244007215 ) ) ;
#6818 = CARTESIAN_POINT ( 'NONE',  ( -23.18613385382707648, 148.9919839608952827, -1.059503902452021418 ) ) ;
#6819 = CARTESIAN_POINT ( 'NONE',  ( 0.9751244372034794106, -10.72340290332181567, 0.05698045496536860433 ) ) ;
#6820 = EDGE_CURVE ( 'NONE', #537, #8461, #17478, .T. ) ;
#6821 = ORIENTED_EDGE ( 'NONE', *, *, #36185, .F. ) ;
#6822 = AXIS2_PLACEMENT_3D ( 'NONE', #5131, #34927, #11483 ) ;
#6823 = CARTESIAN_POINT ( 'NONE',  ( -41.40170217118274110, 22.71997040916441080, 0.2118088196526822786 ) ) ;
#6824 = CARTESIAN_POINT ( 'NONE',  ( 4.699507673534768948, 115.8251506319059843, 1.445723734630264046 ) ) ;
#6825 = PRODUCT_CONTEXT ( 'NONE', #9111, 'mechanical' ) ;
#6826 = CARTESIAN_POINT ( 'NONE',  ( -16.18586682243777020, 146.0959698922748942, 0.6488728679227169227 ) ) ;
#6827 = CARTESIAN_POINT ( 'NONE',  ( 3.811713748825880543, -11.77916328849872052, 0.6977653098966205558 ) ) ;
#6828 = CARTESIAN_POINT ( 'NONE',  ( 14.44833386134782316, 131.1674235819977241, -1.369607862251506436 ) ) ;
#6829 = CARTESIAN_POINT ( 'NONE',  ( -7.650403556475662725, 119.6133147451300971, -1.381840873585064688 ) ) ;
#6830 = DIRECTION ( 'NONE',  ( 5.188838149069472160E-16, -1.699382548006136559E-16, -1.000000000000000000 ) ) ;
#6831 = CARTESIAN_POINT ( 'NONE',  ( 2.969447359227861405, -13.80100253337253946, 0.9847735008004718793 ) ) ;
#6832 = CARTESIAN_POINT ( 'NONE',  ( -3.999880774356848523, 33.21692059697370070, 1.336717509662867620 ) ) ;
#6833 = CARTESIAN_POINT ( 'NONE',  ( 14.24343488940565194, 138.9464670490549452, 0.05414037600900938746 ) ) ;
#6834 = ORIENTED_EDGE ( 'NONE', *, *, #29629, .F. ) ;
#6835 = CARTESIAN_POINT ( 'NONE',  ( -5.024436415346294815, 113.9634239268893339, 1.916893372365422454 ) ) ;
#6836 = DIRECTION ( 'NONE',  ( 0.8745520943968235761, -0.4849315768086558398, 4.268512490100410909E-16 ) ) ;
#6837 = CARTESIAN_POINT ( 'NONE',  ( -11.17805678602830355, 77.92260723867444483, -1.269999999999998685 ) ) ;
#6838 = TOROIDAL_SURFACE ( 'NONE', #25284, 5.080000000000005400, 0.5080000000000000071 ) ;
#6839 = EDGE_CURVE ( 'NONE', #33608, #30025, #13380, .T. ) ;
#6840 = CARTESIAN_POINT ( 'NONE',  ( 12.21488373879589240, 17.14499999999999957, -5.016499999999999737 ) ) ;
#6841 = CARTESIAN_POINT ( 'NONE',  ( 11.70725067560570309, 118.7242475115495495, 0.1376448473428155683 ) ) ;
#6842 = CARTESIAN_POINT ( 'NONE',  ( -2.184544675938124403, 106.6795586461009009, 4.886581511092879637 ) ) ;
#6843 = TOROIDAL_SURFACE ( 'NONE', #23828, 3.683000000000000718, 0.5080000000000000071 ) ;
#6844 = CARTESIAN_POINT ( 'NONE',  ( -0.03523692298175334220, 115.6909491485452435, 1.763399716048406285 ) ) ;
#6845 = B_SPLINE_CURVE_WITH_KNOTS ( 'NONE', 3,
 ( #39253, #10060, #710, #13681, #19848, #501, #26462, #39466, #10269, #26673, #39681, #23453 ),
 .UNSPECIFIED., .F., .F.,
 ( 4, 2, 1, 2, 1, 2, 4 ),
 ( 0.000000000000000000, 0.1250000000000000000, 0.2500000000000000000, 0.5000000000000000000, 0.7500000000000000000, 0.8750000000000000000, 1.000000000000000000 ),
 .UNSPECIFIED. ) ;
#6846 = LINE ( 'NONE', #30255, #21488 ) ;
#6847 = CARTESIAN_POINT ( 'NONE',  ( -3.633364037744279074, 31.58192510899068850, 0.2531645344678472020 ) ) ;
#6848 = EDGE_CURVE ( 'NONE', #8022, #32592, #13222, .T. ) ;
#6849 = CARTESIAN_POINT ( 'NONE',  ( 13.53750608930579169, 121.6867650304669013, 1.656372850109685269 ) ) ;
#6850 = CARTESIAN_POINT ( 'NONE',  ( -0.2796867633624597893, 20.41853924017881283, 4.627572958784220702 ) ) ;
#6851 = CARTESIAN_POINT ( 'NONE',  ( -1.087716277807347254, 29.42523365726748708, -8.383486966309323662 ) ) ;
#6852 = CARTESIAN_POINT ( 'NONE',  ( -2.169812748839434313, 116.7701370764819586, -0.5085666708809641889 ) ) ;
#6853 = CARTESIAN_POINT ( 'NONE',  ( 0.02647280040252846661, 106.0860833631645193, -5.252669131072539521 ) ) ;
#6854 = DIRECTION ( 'NONE',  ( -5.188838149069472160E-16, 1.699382548006136559E-16, 1.000000000000000000 ) ) ;
#6855 = CARTESIAN_POINT ( 'NONE',  ( -10.18297664959815663, 77.66688486464208552, 1.270000000000000906 ) ) ;
#6856 = CARTESIAN_POINT ( 'NONE',  ( 2.891928348976603225, 104.6144662015456959, 3.864987668791159070 ) ) ;
#6857 = CARTESIAN_POINT ( 'NONE',  ( 1.111903444298625754, 15.29877551736591812, 4.515507465039587665 ) ) ;
#6858 = DIRECTION ( 'NONE',  ( -5.188838149069471174E-16, 1.699382548006136313E-16, 1.000000000000000000 ) ) ;
#6859 = DIRECTION ( 'NONE',  ( -0.000000000000000000, -1.000000000000000000, -0.000000000000000000 ) ) ;
#6860 = CARTESIAN_POINT ( 'NONE',  ( 2.104008947125556528, -15.14483647969354330, 5.217645225406672971 ) ) ;
#6861 = CARTESIAN_POINT ( 'NONE',  ( 2.298002300860023439, 118.5759350612125900, -0.7369678581462181244 ) ) ;
#6862 = CARTESIAN_POINT ( 'NONE',  ( -22.93637923037195137, 149.5023856264156450, 0.3943874666890925806 ) ) ;
#6863 = CARTESIAN_POINT ( 'NONE',  ( 7.383526128983457504, 117.2783386326274524, 0.1475404238727041073 ) ) ;
#6864 = ORIENTED_EDGE ( 'NONE', *, *, #39363, .F. ) ;
#6865 = CARTESIAN_POINT ( 'NONE',  ( -4.085839532347240066, 71.06758511999679229, 1.270000000000005125 ) ) ;
#6866 = EDGE_LOOP ( 'NONE', ( #30246, #2506, #24545, #15629 ) ) ;
#6867 = LINE ( 'NONE', #3900, #24692 ) ;
#6868 = CARTESIAN_POINT ( 'NONE',  ( 4.276943344491330734, -15.69687736684960377, 3.951204673509490117 ) ) ;
#6869 = CARTESIAN_POINT ( 'NONE',  ( -20.15738656758755099, 148.0303212619860744, 1.701566911850819208 ) ) ;
#6870 = AXIS2_PLACEMENT_3D ( 'NONE', #34227, #5056, #31216 ) ;
#6871 = CARTESIAN_POINT ( 'NONE',  ( 1.273577801943096999, 159.1407128229522527, -1.197834500974594096 ) ) ;
#6872 = CARTESIAN_POINT ( 'NONE',  ( 0.7580923926444932404, 28.79380631387826028, -0.6184068814828035388 ) ) ;
#6873 = EDGE_CURVE ( 'NONE', #32351, #38361, #482, .T. ) ;
#6874 = CARTESIAN_POINT ( 'NONE',  ( -58.53126320289103290, -0.08783021930335940808, -0.6231558322867893907 ) ) ;
#6875 = ORIENTED_EDGE ( 'NONE', *, *, #3821, .F. ) ;
#6876 = CARTESIAN_POINT ( 'NONE',  ( -24.50334120614357047, 81.61487340491997600, -1.270000000000006457 ) ) ;
#6877 = CARTESIAN_POINT ( 'NONE',  ( -0.02887436318431864379, 106.7790779034713324, 4.972892908546473478 ) ) ;
#6878 = SURFACE_STYLE_USAGE ( .BOTH. , #36064 ) ;
#6879 = PRODUCT_DEFINITION_SHAPE ( 'NONE', 'NONE',  #31572 ) ;
#6880 = CARTESIAN_POINT ( 'NONE',  ( -16.46834812293206340, 148.4304801786341272, 1.248264531716813508 ) ) ;
#6881 = CARTESIAN_POINT ( 'NONE',  ( -5.946078212987909062, 28.42590610009758478, 0.3016625663984517924 ) ) ;
#6882 = EDGE_CURVE ( 'NONE', #21011, #15033, #35167, .T. ) ;
#6883 = CARTESIAN_POINT ( 'NONE',  ( 11.50890483677792453, 122.9335272575421669, -1.234163556480095014 ) ) ;
#6884 = AXIS2_PLACEMENT_3D ( 'NONE', #29412, #23420, #25789 ) ;
#6885 = CARTESIAN_POINT ( 'NONE',  ( -13.83539046132058203, 122.2371923977168109, -1.727333621972642064 ) ) ;
#6886 = CARTESIAN_POINT ( 'NONE',  ( -57.85534701229748578, 0.8496279762696679061, -1.203237356453227047 ) ) ;
#6887 = EDGE_CURVE ( 'NONE', #16766, #35632, #16600, .T. ) ;
#6888 = ORIENTED_EDGE ( 'NONE', *, *, #6536, .F. ) ;
#6889 = CARTESIAN_POINT ( 'NONE',  ( 4.404749925360578189, 118.1622680122423077, -0.4911679557709572874 ) ) ;
#6890 = CARTESIAN_POINT ( 'NONE',  ( 15.47786622725289973, 148.0679034673509875, -0.4116497765502034611 ) ) ;
#6891 = VERTEX_POINT ( 'NONE', #33 ) ;
#6892 = CARTESIAN_POINT ( 'NONE',  ( -10.89299388415068037, 123.1276765127550021, -1.556224048961160733 ) ) ;
#6893 = CARTESIAN_POINT ( 'NONE',  ( 3.043194142253923928, -14.61827878651010515, -0.2680077959190000358 ) ) ;
#6894 = CARTESIAN_POINT ( 'NONE',  ( -3.156656716243205096, 105.1239622688229645, -4.301121616660518399 ) ) ;
#6895 = CARTESIAN_POINT ( 'NONE',  ( -44.40685758373556524, 19.43703734468909516, -6.894256627225939810E-15 ) ) ;
#6896 = CARTESIAN_POINT ( 'NONE',  ( -2.734508853367146219, 0.3528594962865297391, 3.724956791467788353 ) ) ;
#6897 = CARTESIAN_POINT ( 'NONE',  ( 0.5409540667463921260, 119.9180165495073283, 0.4819738915938378554 ) ) ;
#6898 = CARTESIAN_POINT ( 'NONE',  ( 1.544194705859216921, 35.01746917326339315, 0.8070499108633334417 ) ) ;
#6899 = AXIS2_PLACEMENT_3D ( 'NONE', #27846, #34667, #18457 ) ;
#6900 = CARTESIAN_POINT ( 'NONE',  ( 7.741462187161934239, -10.92447321953606654, -3.338652055795839679 ) ) ;
#6901 = CARTESIAN_POINT ( 'NONE',  ( 10.25892126925246295, 126.0184183664171655, 0.2980827979995014365 ) ) ;
#6902 = CARTESIAN_POINT ( 'NONE',  ( -30.37855815223275258, 71.48694267763936239, 1.269999999999992246 ) ) ;
#6903 = CARTESIAN_POINT ( 'NONE',  ( -52.42931032121356338, 11.92852722686772005, -4.179465640474091970 ) ) ;
#6904 = CARTESIAN_POINT ( 'NONE',  ( 6.608367952640213261, 78.82866613109550258, 3.480504251946402228 ) ) ;
#6905 = CARTESIAN_POINT ( 'NONE',  ( 3.174366308151881366, 82.64346620154573486, 0.06343139340882768262 ) ) ;
#6906 = VECTOR ( 'NONE', #20175, 1000.000000000000000 ) ;
#6907 = DIRECTION ( 'NONE',  ( 4.017660918040594346E-17, -1.000000000000000000, -2.376309959284834438E-19 ) ) ;
#6908 = CARTESIAN_POINT ( 'NONE',  ( -31.37023363772181028, 53.64958092169537451, 1.269999999999992912 ) ) ;
#6909 = CARTESIAN_POINT ( 'NONE',  ( -8.133186750442957802, 120.8103564082440613, -1.375394817141416981 ) ) ;
#6910 = CARTESIAN_POINT ( 'NONE',  ( 3.164706401634689303, 50.63946620154572997, 1.543954388298181213 ) ) ;
#6911 = CARTESIAN_POINT ( 'NONE',  ( -6.059261036834477920, 56.51499999999997925, 5.016500000000000625 ) ) ;
#6912 = DIRECTION ( 'NONE',  ( -0.9998004120163610509, -4.016384292689131511E-17, -0.01997839162482749689 ) ) ;
#6913 = CARTESIAN_POINT ( 'NONE',  ( -56.26154134542980501, 7.775270144418685803, -1.045335966129298087E-14 ) ) ;
#6914 = CARTESIAN_POINT ( 'NONE',  ( -57.52317756609133426, 3.014644041894651405, 1.981665235817938076 ) ) ;
#6915 = CARTESIAN_POINT ( 'NONE',  ( -8.212232005054575623, 117.5299140688306352, 0.02651185805045446278 ) ) ;
#6916 = EDGE_CURVE ( 'NONE', #2842, #35121, #28861, .T. ) ;
#6917 = ORIENTED_EDGE ( 'NONE', *, *, #16774, .T. ) ;
#6918 = CARTESIAN_POINT ( 'NONE',  ( -51.41777536269126614, 18.15702087101736595, -2.173118852595011141 ) ) ;
#6919 = CARTESIAN_POINT ( 'NONE',  ( -6.056369948572695172, 121.4335403551348804, -0.1264477557253972650 ) ) ;
#6920 = ORIENTED_EDGE ( 'NONE', *, *, #35461, .T. ) ;
#6921 = DIRECTION ( 'NONE',  ( 0.01997839162482749689, 1.040247600000945640E-18, -0.9998004120163610509 ) ) ;
#6922 = CARTESIAN_POINT ( 'NONE',  ( -11.83578944268997724, 152.0103986367769551, -0.2843524715992693519 ) ) ;
#6923 = CARTESIAN_POINT ( 'NONE',  ( 6.383535934857802907, -12.90002020050165576, 0.3830569482466484321 ) ) ;
#6924 = CARTESIAN_POINT ( 'NONE',  ( -14.04756362465215247, 122.1591959312462592, 1.132115996748545239 ) ) ;
#6925 = CARTESIAN_POINT ( 'NONE',  ( 3.043391175932955495, 18.63480288530714191, -3.501419995799015528 ) ) ;
#6926 = CARTESIAN_POINT ( 'NONE',  ( 23.32660363739032761, 146.7646281656787437, 0.9249455126139315420 ) ) ;
#6927 = CARTESIAN_POINT ( 'NONE',  ( 15.71643150686912627, 145.6795463615453059, 0.5158341164768996956 ) ) ;
#6928 = CARTESIAN_POINT ( 'NONE',  ( 18.35410564743290607, 77.35382415001784295, 1.904999999999988480 ) ) ;
#6929 = CARTESIAN_POINT ( 'NONE',  ( 0.9169382621377788478, -11.15192339915171793, 0.3232733857163304081 ) ) ;
#6930 = CARTESIAN_POINT ( 'NONE',  ( -22.64824804725711971, 137.2763855621842026, -0.6699328029008018159 ) ) ;
#6931 = CARTESIAN_POINT ( 'NONE',  ( -6.651972016613293606E-14, 104.1064662015457287, 7.011588703784780528E-31 ) ) ;
#6932 = DIRECTION ( 'NONE',  ( 1.000000000000000000, -9.627370216492862708E-17, 0.000000000000000000 ) ) ;
#6933 = EDGE_LOOP ( 'NONE', ( #25025, #23634, #38060, #5306 ) ) ;
#6934 = CARTESIAN_POINT ( 'NONE',  ( -2.190925350822380047, 116.2108782439287467, -0.0004523116112769919148 ) ) ;
#6935 = ORIENTED_EDGE ( 'NONE', *, *, #36185, .T. ) ;
#6936 = CARTESIAN_POINT ( 'NONE',  ( -18.08730999440964027, 147.8422069945528108, 1.617706263729447924 ) ) ;
#6937 = CARTESIAN_POINT ( 'NONE',  ( 7.213960532367366341, 78.77618639008778700, 1.904999999999999583 ) ) ;
#6938 = CARTESIAN_POINT ( 'NONE',  ( 12.00897459848969007, 120.6765805525287334, 1.550193712165491178 ) ) ;
#6939 = CARTESIAN_POINT ( 'NONE',  ( 19.17595810167853898, 140.9752145814059645, -1.751973952106583576 ) ) ;
#6940 = CARTESIAN_POINT ( 'NONE',  ( -0.2928493810785644524, 9.627489959316354984, 0.9317482488014678932 ) ) ;
#6941 = AXIS2_PLACEMENT_3D ( 'NONE', #5138, #18717, #31940 ) ;
#6942 = CARTESIAN_POINT ( 'NONE',  ( -21.45663756426511526, 150.2128557559047692, -2.007674378541678628 ) ) ;
#6943 = CARTESIAN_POINT ( 'NONE',  ( 4.572607118633827739, 118.0342741157669053, -0.6784189215572231646 ) ) ;
#6944 = AXIS2_PLACEMENT_3D ( 'NONE', #3299, #13507, #6699 ) ;
#6945 = ADVANCED_FACE ( 'NONE', ( #3021 ), #39058, .T. ) ;
#6946 = CARTESIAN_POINT ( 'NONE',  ( 6.134665891606675636, 119.5049778551863682, 0.5179261928985369190 ) ) ;
#6947 = ADVANCED_FACE ( 'NONE', ( #15977 ), #6401, .T. ) ;
#6948 = CARTESIAN_POINT ( 'NONE',  ( 5.877307974080531849, 120.8872308857076519, -0.5842564153471765387 ) ) ;
#6949 = CARTESIAN_POINT ( 'NONE',  ( -15.76486438913732613, 145.9085485750152316, -0.2635089261703655317 ) ) ;
#6950 = ORIENTED_EDGE ( 'NONE', *, *, #9615, .F. ) ;
#6951 = CARTESIAN_POINT ( 'NONE',  ( -5.042934966769651695, 119.7208665877771665, -1.041708725922360523 ) ) ;
#6952 = CARTESIAN_POINT ( 'NONE',  ( 4.389818247250405037, -15.68135102926887470, 3.766867903159812681 ) ) ;
#6953 = CARTESIAN_POINT ( 'NONE',  ( -4.590154465017951324, 118.0230796030913893, -0.8584153040694411096 ) ) ;
#6954 = CARTESIAN_POINT ( 'NONE',  ( -43.24646561529713296, 21.63922848039483071, -2.381786957946274264 ) ) ;
#6955 = DIRECTION ( 'NONE',  ( -1.000000000000000000, 0.000000000000000000, 0.000000000000000000 ) ) ;
#6956 = CARTESIAN_POINT ( 'NONE',  ( 11.42611330002548087, 154.6851215890897038, 2.167138196937119066 ) ) ;
#6957 = CARTESIAN_POINT ( 'NONE',  ( -0.5321123018419734452, 37.22158963861809156, -0.7300149017649124605 ) ) ;
#6958 = DIRECTION ( 'NONE',  ( -0.9998004120163608288, 0.000000000000000000, -0.01997839162482749342 ) ) ;
#6959 = CARTESIAN_POINT ( 'NONE',  ( -4.802295984089328229, 116.4582014290525507, 0.9960034115346418915 ) ) ;
#6960 = CARTESIAN_POINT ( 'NONE',  ( -0.9765287272027848298, 24.25689591457997452, 8.364652468500624494 ) ) ;
#6961 = CARTESIAN_POINT ( 'NONE',  ( 10.72508252498916725, 126.1521286088116369, 0.7954780730053834237 ) ) ;
#6962 = CARTESIAN_POINT ( 'NONE',  ( 22.81445126409626667, 149.1304179266472261, -0.6239350898115070265 ) ) ;
#6963 = CARTESIAN_POINT ( 'NONE',  ( -15.50061618130081165, 62.14374591690594940, -1.904999999999999583 ) ) ;
#6965 = B_SPLINE_CURVE_WITH_KNOTS ( 'NONE', 3,
 ( #8112, #40710, #21086, #7497, #4315, #17062, #40304, #17897, #30899, #4732, #17684, #4519, #17279, #1739, #30268, #14698, #27703, #13876 ),
 .UNSPECIFIED., .F., .F.,
 ( 4, 2, 2, 2, 2, 2, 2, 2, 4 ),
 ( 0.0003740348303357290786, 0.003617653094789048760, 0.006861271359242368875, 0.008483080491469027415, 0.009293985057582358419, 0.01010488962369568942, 0.01172669875592231847, 0.01253760332203563213, 0.01334850788814894752 ),
 .UNSPECIFIED. ) ;
#6964 = FACE_OUTER_BOUND ( 'NONE', #22805, .T. ) ;
#6966 = UNCERTAINTY_MEASURE_WITH_UNIT (LENGTH_MEASURE( 1.000000000000000082E-05 ), #37731, 'distance_accuracy_value', 'NONE');
#6967 = CARTESIAN_POINT ( 'NONE',  ( -9.820189317990269728, 117.9942579372833933, -0.1809356799706721142 ) ) ;
#6968 = ORIENTED_EDGE ( 'NONE', *, *, #25636, .T. ) ;
#6969 = CARTESIAN_POINT ( 'NONE',  ( -6.748423061888915164, 121.1153472631275179, -0.9535781417299137308 ) ) ;
#6970 = CARTESIAN_POINT ( 'NONE',  ( 5.718778735283957637, -14.43046299137125388, 2.876564826015278520 ) ) ;
#6971 = CARTESIAN_POINT ( 'NONE',  ( -14.74011517316811215, 148.8440819608433969, -0.7404754567584957980 ) ) ;
#6972 = CARTESIAN_POINT ( 'NONE',  ( 3.826441825042426359, -13.78667705120290066, 4.058770776067232688 ) ) ;
#6973 = CARTESIAN_POINT ( 'NONE',  ( -13.66011217756167184, 120.8017016962898396, 0.8211468655896804192 ) ) ;
#6974 = CARTESIAN_POINT ( 'NONE',  ( -15.19943428492320869, 148.1072807477730748, -0.3037208696559880461 ) ) ;
#6975 = CARTESIAN_POINT ( 'NONE',  ( 8.075047650969494839, 158.6620026115301698, 0.1796671307923023986 ) ) ;
#6976 = ORIENTED_EDGE ( 'NONE', *, *, #35539, .F. ) ;
#6977 = CARTESIAN_POINT ( 'NONE',  ( -1.504723661876595786, -8.552649586842417051, -4.374500482163298898 ) ) ;
#6978 = CARTESIAN_POINT ( 'NONE',  ( -6.894732321505390615, 117.1676844715483270, -0.1377731603346601386 ) ) ;
#6979 = DIRECTION ( 'NONE',  ( 0.6594218222380416883, 0.7517731442105793915, 0.000000000000000000 ) ) ;
#6980 = VECTOR ( 'NONE', #41214, 1000.000000000000000 ) ;
#6981 = FACE_OUTER_BOUND ( 'NONE', #40190, .T. ) ;
#6982 = CARTESIAN_POINT ( 'NONE',  ( 6.614212317611555925, 120.0220961648606561, 1.233748940741835609 ) ) ;
#6983 = ADVANCED_FACE ( 'NONE', ( #9810 ), #14560, .T. ) ;
#6984 = CARTESIAN_POINT ( 'NONE',  ( 3.019445949670579665, 11.99742794009110014, 3.522755186455234000 ) ) ;
#6985 = CARTESIAN_POINT ( 'NONE',  ( 14.16249321059112809, 121.1589565784038456, 1.397539518993202723 ) ) ;
#6986 = CARTESIAN_POINT ( 'NONE',  ( -0.03707542933699707610, 115.3931862868688398, 1.855406091731380824 ) ) ;
#6988 = CARTESIAN_POINT ( 'NONE',  ( 6.823161219633183450, 118.5360090424673274, -0.8871979454111537100 ) ) ;
#6987 = CARTESIAN_POINT ( 'NONE',  ( -23.91048590848665967, 81.84235438443283783, 1.523999999999993138 ) ) ;
#6989 = CARTESIAN_POINT ( 'NONE',  ( 2.298459491326434900, 5.325542553220859787, -4.024866414273244430 ) ) ;
#6990 = CARTESIAN_POINT ( 'NONE',  ( -6.882329627759522062, 117.5897289630162987, -0.7523600398187278993 ) ) ;
#6991 = EDGE_CURVE ( 'NONE', #6464, #20372, #38582, .T. ) ;
#6992 = EDGE_LOOP ( 'NONE', ( #28561, #6587, #30343, #18853 ) ) ;
#6993 = FACE_OUTER_BOUND ( 'NONE', #33239, .T. ) ;
#6994 = EDGE_LOOP ( 'NONE', ( #345, #8187, #28575 ) ) ;
#6995 = CARTESIAN_POINT ( 'NONE',  ( -5.257554009420361218, 121.2670714900434206, 0.1164621724739934722 ) ) ;
#6996 = CARTESIAN_POINT ( 'NONE',  ( 5.987854329437395151, -12.83555092537783082, 1.339350064115379935 ) ) ;
#6997 = CARTESIAN_POINT ( 'NONE',  ( -47.19240717248583650, 20.04893757306883018, 5.078271723504655277 ) ) ;
#6998 = AXIS2_PLACEMENT_3D ( 'NONE', #26504, #6921, #39508 ) ;
#6999 = DIRECTION ( 'NONE',  ( -0.8745520943968240202, 0.4849315768086551737, -5.361993529360572958E-16 ) ) ;
#7000 = VERTEX_POINT ( 'NONE', #39000 ) ;
#7001 = CARTESIAN_POINT ( 'NONE',  ( 12.70837813489428569, 122.8260676081006153, 1.843161107213562966 ) ) ;
#7002 = CARTESIAN_POINT ( 'NONE',  ( -18.35410564743290962, 77.35382415001784295, 1.904999999999988258 ) ) ;
#7003 = CARTESIAN_POINT ( 'NONE',  ( 12.85860202769631755, 133.7716054015561156, 0.2569454702854388484 ) ) ;
#7004 = VECTOR ( 'NONE', #9931, 1000.000000000000000 ) ;
#7005 = CARTESIAN_POINT ( 'NONE',  ( -18.09030135340804435, 154.0913862843578670, 0.7524810965364959747 ) ) ;
#7006 = CARTESIAN_POINT ( 'NONE',  ( 3.518211725887771202, 24.73955407011506935, -7.658871095584262711 ) ) ;
#7007 = AXIS2_PLACEMENT_3D ( 'NONE', #35820, #30407, #1256 ) ;
#7008 = CARTESIAN_POINT ( 'NONE',  ( 5.670663496353971489, 159.1134716836843381, -0.2862304005612824054 ) ) ;
#7009 = DIRECTION ( 'NONE',  ( 5.206863593109713661E-17, -1.000000000000000000, 1.077750396879097183E-30 ) ) ;
#7010 = CARTESIAN_POINT ( 'NONE',  ( -46.69016964900118438, 26.00918483878763254, 1.334034565177987242 ) ) ;
#7011 = CARTESIAN_POINT ( 'NONE',  ( -47.48049929620759002, 23.18975938597035125, 2.730405167055922178 ) ) ;
#7012 = CARTESIAN_POINT ( 'NONE',  ( 2.097955312704908870, -15.07800414366253250, 5.719157372618502322 ) ) ;
#7014 = CARTESIAN_POINT ( 'NONE',  ( -51.73272837791831336, 13.19950324185369794, 4.393710239503571202 ) ) ;
#7013 = B_SPLINE_CURVE_WITH_KNOTS ( 'NONE', 3,
 ( #24294, #37928, #37501, #18526, #40716, #8751, #8327, #34325, #1950, #18315, #40920, #1743, #37300, #21297, #34534, #21713, #5154, #1538, #25143, #18108, #34737, #40515, #8542, #41349, #21091, #31531, #8117, #38147, #21501, #30688, #2161, #12151, #30904, #14910, #15120, #2375, #31113, #28123, #27506, #27914, #15335, #11726, #24714, #41133, #11939, #24930, #34115, #28340, #8960, #11307, #33908, #4942, #14702, #17901, #27707, #4736, #17689, #14493, #9173, #5780, #41558, #35788, #41973, #35361, #41769, #28550, #25557, #12978, #39187, #38561, #25971, #224, #35159, #12, #16379, #19160, #9374, #2999, #31745, #9580, #28756, #2588, #18949, #22338, #19365, #26183, #6600, #3200, #38358, #6191, #5986, #18735 ),
 .UNSPECIFIED., .F., .F.,
 ( 4, 2, 2, 2, 2, 2, 1, 1, 2, 2, 2, 2, 2, 2, 2, 2, 2, 1, 1, 2, 2, 2, 2, 1, 1, 2, 2, 2, 1, 2, 2, 1, 1, 2, 2, 2, 1, 1, 1, 2, 2, 2, 2, 2, 2, 2, 1, 1, 1, 1, 2, 2, 2, 4 ),
 ( 0.000000000000000000, 0.03125000000000136002, 0.04687500000000204003, 0.06250000000000273392, 0.09375000000000413558, 0.1093750000000048711, 0.1171875000000052458, 0.1210937500000054123, 0.1230468750000054678, 0.1250000000000055234, 0.1406250000000056899, 0.1484375000000058009, 0.1523437500000058287, 0.1562500000000058564, 0.1718750000000059119, 0.1875000000000059952, 0.2187500000000059952, 0.2343750000000059674, 0.2421875000000059119, 0.2460937500000058842, 0.2500000000000058287, 0.3125000000000036637, 0.3437500000000024980, 0.3593750000000018874, 0.3671875000000014988, 0.3710937500000013323, 0.3750000000000011657, 0.4062499999999998890, 0.4140624999999997224, 0.4160156249999996114, 0.4169921874999994449, 0.4179687499999992784, 0.4218749999999984457, 0.4374999999999966693, 0.4687499999999931166, 0.4843749999999915068, 0.4921874999999907296, 0.4960937499999902855, 0.4980468749999899525, 0.4990234374999898415, 0.4999999999999897304, 0.5624999999999931166, 0.5937499999999948930, 0.6093749999999957812, 0.6249999999999966693, 0.6875000000000003331, 0.7187500000000024425, 0.7343750000000034417, 0.7421875000000041078, 0.7460937500000043299, 0.7480468750000043299, 0.7500000000000043299, 0.8750000000000022204, 1.000000000000000000 ),
 .UNSPECIFIED. ) ;
#7015 = CARTESIAN_POINT ( 'NONE',  ( -58.70326665360445872, -0.3146233719498078840, 0.2858976903834491434 ) ) ;
#7016 = CARTESIAN_POINT ( 'NONE',  ( -4.517639745569246301, 118.1171028094802011, 0.5418958579287725952 ) ) ;
#7017 = CARTESIAN_POINT ( 'NONE',  ( -5.777868923222812647, 78.89722547516474549, -5.030779815616708284 ) ) ;
#7018 = ORIENTED_EDGE ( 'NONE', *, *, #7400, .F. ) ;
#7019 = CARTESIAN_POINT ( 'NONE',  ( -42.34481381083929818, 23.19759442052183473, 1.554397948409609542 ) ) ;
#7020 = CARTESIAN_POINT ( 'NONE',  ( -3.773169269958028149, 118.9364908861665242, -0.9318311032467860855 ) ) ;
#7021 = CARTESIAN_POINT ( 'NONE',  ( -7.449435858333571581, 123.6645382909113664, -0.1834419053087674445 ) ) ;
#7022 = CARTESIAN_POINT ( 'NONE',  ( 4.564985497539753467, 118.0819797128260404, 0.7245633110350869766 ) ) ;
#7023 = CARTESIAN_POINT ( 'NONE',  ( -15.73537819279964900, 147.9505201145231865, -1.277015258756127647 ) ) ;
#7024 = CIRCLE ( 'NONE', #13821, 13.46199999999999442 ) ;
#7025 = CARTESIAN_POINT ( 'NONE',  ( -1.784412496506031065, 115.7029491485453434, -1.723391489024520107 ) ) ;
#7026 = CARTESIAN_POINT ( 'NONE',  ( -36.79765817521327165, 27.64956762128695900, -1.270000000000003570 ) ) ;
#7027 = CARTESIAN_POINT ( 'NONE',  ( 5.416379098809391834, 117.1811293437636721, -0.6832607176795200132 ) ) ;
#7028 = CARTESIAN_POINT ( 'NONE',  ( -9.541807374902315786, 122.7780075402122151, -1.248600054375463397 ) ) ;
#7029 = CARTESIAN_POINT ( 'NONE',  ( -5.332935397695336199, 116.0444662015457311, -0.1065647409268299234 ) ) ;
#7030 = CARTESIAN_POINT ( 'NONE',  ( -0.02768739821015298377, 156.9833357668885014, 1.385590625008459087 ) ) ;
#7031 = CARTESIAN_POINT ( 'NONE',  ( -36.98328822617348521, 27.82293856516311692, -1.524000000000003796 ) ) ;
#7032 = CARTESIAN_POINT ( 'NONE',  ( -15.64366209671519670, 147.2213131111883513, -0.2456931987577644916 ) ) ;
#7033 = CARTESIAN_POINT ( 'NONE',  ( -0.5842699607273857954, -4.454521554441356557, 4.585487691134133570 ) ) ;
#7034 = CARTESIAN_POINT ( 'NONE',  ( 22.53452490051026658, 150.3096427868838987, 1.298398843693310267 ) ) ;
#7035 = CARTESIAN_POINT ( 'NONE',  ( -30.19451713491628198, 70.61549828015995445, 1.523999999999992028 ) ) ;
#7036 = CARTESIAN_POINT ( 'NONE',  ( 3.228916932056940858, -14.69740968606676823, 0.4668019137946345376 ) ) ;
#7037 = CARTESIAN_POINT ( 'NONE',  ( -19.00246547725227231, 147.5601278813269914, 1.724645192979526565 ) ) ;
#7038 = CARTESIAN_POINT ( 'NONE',  ( -0.2870776928289196506, 5.753151106566044781, -0.9307745581249481370 ) ) ;
#7039 = CARTESIAN_POINT ( 'NONE',  ( -15.27623507474957876, 120.8527393138689376, -0.8201955439070724996 ) ) ;
#7040 = TOROIDAL_SURFACE ( 'NONE', #11759, 17.68910244842765778, 0.6350000000000000089 ) ;
#7041 = CARTESIAN_POINT ( 'NONE',  ( 0.1071387893147941056, 24.31912984647217968, -0.9680276682219529638 ) ) ;
#7042 = ORIENTED_EDGE ( 'NONE', *, *, #39334, .F. ) ;
#7043 = CARTESIAN_POINT ( 'NONE',  ( -42.12253153191133492, 21.94389511927448311, -4.944039522370902375E-15 ) ) ;
#7044 = CARTESIAN_POINT ( 'NONE',  ( 5.237871118309306517, 118.7524313932052991, 0.6368175916084592991 ) ) ;
#7045 = CONTEXT_DEPENDENT_SHAPE_REPRESENTATION ( #3389, #32727 ) ;
#7046 = CARTESIAN_POINT ( 'NONE',  ( -10.78632646169022280, 153.0872561326487187, 0.6669751843662028445 ) ) ;
#7047 = CARTESIAN_POINT ( 'NONE',  ( 3.889980283446199838, -12.05568003970028457, 1.127423567058935205 ) ) ;
#7048 = CARTESIAN_POINT ( 'NONE',  ( 11.13866856781917392, 123.6647009725989648, -1.091370626813936706 ) ) ;
#7049 = CARTESIAN_POINT ( 'NONE',  ( -19.49537437117590599, 147.7952244890416296, -2.518105945687704406 ) ) ;
#7050 = CARTESIAN_POINT ( 'NONE',  ( 3.486869749213982406, 104.6144662015456959, 3.351517259169598528 ) ) ;
#7051 = CARTESIAN_POINT ( 'NONE',  ( 3.116451998213339625, -14.00698646007624149, 1.619014592372306716 ) ) ;
#7052 = CARTESIAN_POINT ( 'NONE',  ( -5.656553017150170781, 31.30584249932583774, -0.4062832063744321043 ) ) ;
#7053 = CARTESIAN_POINT ( 'NONE',  ( 5.292481242635903804, 121.3432423864224177, 0.03610140192510987583 ) ) ;
#7054 = ORIENTED_EDGE ( 'NONE', *, *, #5258, .F. ) ;
#7055 = CARTESIAN_POINT ( 'NONE',  ( -2.507392566506281728, 107.3035951680821967, 4.608238627831032552 ) ) ;
#7056 = DIRECTION ( 'NONE',  ( -0.9998004120163610509, -4.016384292689131511E-17, -0.01997839162482749689 ) ) ;
#7057 = AXIS2_PLACEMENT_3D ( 'NONE', #25916, #13141, #22911 ) ;
#7058 = CARTESIAN_POINT ( 'NONE',  ( -23.97640303682767993, 76.49434496853974963, 1.523999999999994026 ) ) ;
#7059 = DIRECTION ( 'NONE',  ( -4.017660918040594346E-17, 1.000000000000000000, 2.376309959284834438E-19 ) ) ;
#7060 = AXIS2_PLACEMENT_3D ( 'NONE', #2918, #31872, #28674 ) ;
#7061 = CARTESIAN_POINT ( 'NONE',  ( 1.829002187088338838, 116.5125207362610951, -0.06620492630546132018 ) ) ;
#7062 = CARTESIAN_POINT ( 'NONE',  ( -7.639359131133931946, 124.2918010433613745, -0.1437932647211236370 ) ) ;
#7063 = TOROIDAL_SURFACE ( 'NONE', #11124, 6.826249999999999929, 0.6350000000000000089 ) ;
#7064 = CARTESIAN_POINT ( 'NONE',  ( -0.4392745730724126330, 115.6909491485452435, 1.750092874769185070 ) ) ;
#7065 = CARTESIAN_POINT ( 'NONE',  ( 11.66725022231030628, 55.24499999999999744, 5.016500000000000625 ) ) ;
#7066 = CARTESIAN_POINT ( 'NONE',  ( -3.884074962540208897, 32.38989619462120828, 0.9675453285884029198 ) ) ;
#7067 = CARTESIAN_POINT ( 'NONE',  ( 6.788760123629391074, 157.9234729166680040, 1.828055096104673760 ) ) ;
#7068 = CARTESIAN_POINT ( 'NONE',  ( 4.466176584706416541, 22.48015689762229030, 1.290832665783417488 ) ) ;
#7069 = CARTESIAN_POINT ( 'NONE',  ( 7.942258639034435852, 16.71227948022357523, 2.857158061122382353 ) ) ;
#7070 = CARTESIAN_POINT ( 'NONE',  ( 8.664868210595660258, 118.4192301925127566, -0.7007756955166910551 ) ) ;
#7071 = CARTESIAN_POINT ( 'NONE',  ( 0.1065646865915094443, 105.8844662015457203, -5.332932678536313809 ) ) ;
#7072 = CIRCLE ( 'NONE', #13205, 0.6350000000000001199 ) ;
#7073 = CARTESIAN_POINT ( 'NONE',  ( -5.767947771862510287, 78.89823565723088450, 5.032924692340702499 ) ) ;
#7074 = CARTESIAN_POINT ( 'NONE',  ( -10.94257363143045936, 56.35470871607773091, -4.428493390991015133 ) ) ;
#7075 = CARTESIAN_POINT ( 'NONE',  ( 1.151590580803910635, 105.1234912291904209, 5.218814051747787452 ) ) ;
#7076 = CARTESIAN_POINT ( 'NONE',  ( -2.359559261509405204, 14.11188314818778267, 3.974389579228013503 ) ) ;
#7077 = CARTESIAN_POINT ( 'NONE',  ( -48.28978369826177186, 19.63653578263564015, -5.206999999995405304 ) ) ;
#7078 = FACE_OUTER_BOUND ( 'NONE', #9304, .T. ) ;
#7079 = CARTESIAN_POINT ( 'NONE',  ( 3.387566103704702236, -13.77904243453481570, 2.987699908524332759 ) ) ;
#7080 = CARTESIAN_POINT ( 'NONE',  ( 1.795323270064338006, 111.6436615656963909, -3.008962535700986152 ) ) ;
#7081 = CARTESIAN_POINT ( 'NONE',  ( -10.53014098995834225, 157.9057380314836223, 0.5653498989572930400 ) ) ;
#7082 = EDGE_CURVE ( 'NONE', #37511, #33280, #21428, .T. ) ;
#7083 = CARTESIAN_POINT ( 'NONE',  ( 4.999405081406732343, 117.4046814563082819, -0.8308242854346027384 ) ) ;
#7084 = VERTEX_POINT ( 'NONE', #16398 ) ;
#7085 = CARTESIAN_POINT ( 'NONE',  ( -5.885917553499152355, 77.12042444889114279, -1.269999999999996021 ) ) ;
#7086 = ORIENTED_EDGE ( 'NONE', *, *, #1140, .T. ) ;
#7087 = CARTESIAN_POINT ( 'NONE',  ( -2.317791448294674428, 31.60761946039689718, 1.124105164688197211 ) ) ;
#7088 = TOROIDAL_SURFACE ( 'NONE', #20680, 0.7620000000000000107, 0.2540000000000000036 ) ;
#7089 = CARTESIAN_POINT ( 'NONE',  ( 3.016856305723133236, -15.72087675955979869, 4.784217253217923016 ) ) ;
#7090 = CARTESIAN_POINT ( 'NONE',  ( -17.73303733098149593, 151.6044147853587845, 1.711203799303050888 ) ) ;
#7091 = CARTESIAN_POINT ( 'NONE',  ( 21.57210427006330278, 149.5883454796168621, -1.274511887596344817 ) ) ;
#7092 = CARTESIAN_POINT ( 'NONE',  ( 4.560281875334545099, -11.68902278883368595, 0.6958564903332965512 ) ) ;
#7093 = EDGE_CURVE ( 'NONE', #20396, #32690, #29404, .T. ) ;
#7094 = CARTESIAN_POINT ( 'NONE',  ( -58.58102607532369888, -0.1934477224862401756, -0.5095094156256858575 ) ) ;
#7095 = ORIENTED_EDGE ( 'NONE', *, *, #30382, .F. ) ;
#7096 = CARTESIAN_POINT ( 'NONE',  ( -58.34682947232719386, -0.2434262655763713701, -0.1887554165967095521 ) ) ;
#7097 = CARTESIAN_POINT ( 'NONE',  ( 0.1328480158795370403, 107.4969721965504021, 4.685401909699153045 ) ) ;
#7098 = CARTESIAN_POINT ( 'NONE',  ( -5.070296302330613791, 156.2174774745075183, 1.306674740328298334 ) ) ;
#7099 = DIRECTION ( 'NONE',  ( 0.9998004120163608288, 0.000000000000000000, 0.01997839162482736852 ) ) ;
#7100 = CARTESIAN_POINT ( 'NONE',  ( 11.76378629788668384, 123.2143981803894093, -1.250304744737055218 ) ) ;
#7101 = CARTESIAN_POINT ( 'NONE',  ( -20.68324476251077115, 149.5879773183856685, -2.343194491808722191 ) ) ;
#7102 = CARTESIAN_POINT ( 'NONE',  ( -57.22363667057550884, 2.289652018204080264, -1.875138655370660379 ) ) ;
#7103 = CIRCLE ( 'NONE', #26116, 0.2539999999999990599 ) ;
#7104 = ORIENTED_EDGE ( 'NONE', *, *, #9655, .F. ) ;
#7105 = CARTESIAN_POINT ( 'NONE',  ( 4.413039900744538890, 118.1641392279842364, -0.4832662010003311859 ) ) ;
#7106 = ADVANCED_FACE ( 'NONE', ( #23412 ), #4705, .T. ) ;
#7107 = CARTESIAN_POINT ( 'NONE',  ( 8.835859712557383006, 123.2701452714374568, -0.3110363621490745967 ) ) ;
#7108 = VERTEX_POINT ( 'NONE', #874 ) ;
#7109 = CARTESIAN_POINT ( 'NONE',  ( 3.118150858982619233, -14.63350761981947734, -0.02509704758125085033 ) ) ;
#7110 = CIRCLE ( 'NONE', #28160, 5.588000000000006295 ) ;
#7111 = DIRECTION ( 'NONE',  ( 1.011795553208986377E-16, 1.000000000000000000, -0.000000000000000000 ) ) ;
#7112 = CARTESIAN_POINT ( 'NONE',  ( -58.34556966141487067, -0.2407783058111234720, 0.1938516799453078032 ) ) ;
#7113 = CARTESIAN_POINT ( 'NONE',  ( 4.585212383536918956, 13.09695617864405470, 0.6580430208065696229 ) ) ;
#7115 = EDGE_CURVE ( 'NONE', #20737, #35057, #7110, .T. ) ;
#7114 = CARTESIAN_POINT ( 'NONE',  ( 3.428210029137735759, 119.9243055703230851, 0.7605957222121786376 ) ) ;
#7116 = CARTESIAN_POINT ( 'NONE',  ( -2.443897349042808642, 30.72383818298906988, 1.256468113927755148 ) ) ;
#7117 = TOROIDAL_SURFACE ( 'NONE', #2349, 6.985000000000000320, 0.6350000000000000089 ) ;
#7118 = CARTESIAN_POINT ( 'NONE',  ( -1.178223178616622402, 14.53665720681882689, 4.476207649055042204 ) ) ;
#7119 = CARTESIAN_POINT ( 'NONE',  ( 8.876935545690592733, 123.7004864364556909, 0.3337242414277969971 ) ) ;
#7120 = DIRECTION ( 'NONE',  ( -0.5064479475276348897, 0.8622111466057285067, -0.01012003527073121814 ) ) ;
#7121 = EDGE_CURVE ( 'NONE', #33175, #10936, #23398, .T. ) ;
#7122 = EDGE_CURVE ( 'NONE', #38903, #30579, #11799, .T. ) ;
#7123 = CARTESIAN_POINT ( 'NONE',  ( -53.80167111242602118, 9.145755618221249605, -3.362987294923143633 ) ) ;
#7124 = CARTESIAN_POINT ( 'NONE',  ( 5.552440004966861409, 116.7968546181220120, -0.2240355716773803907 ) ) ;
#7125 = DIRECTION ( 'NONE',  ( -0.9998004120163608288, 0.000000000000000000, -0.01997839162482747608 ) ) ;
#7126 = CARTESIAN_POINT ( 'NONE',  ( -14.60499999999999865, 71.11999999999999034, 5.079999999999997407 ) ) ;
#7127 = CARTESIAN_POINT ( 'NONE',  ( -17.09698261757901960, 84.43312239790384410, -1.524000000000002908 ) ) ;
#7128 = CARTESIAN_POINT ( 'NONE',  ( -7.772068811996249771, 69.25462295839062676, 1.270000000000003570 ) ) ;
#7129 = CARTESIAN_POINT ( 'NONE',  ( -5.860205464978564649, 56.51500000000000057, 5.019550312247363699 ) ) ;
#7130 = DIRECTION ( 'NONE',  ( -0.8745520943968247973, 0.4849315768086537304, -5.361993529360573944E-16 ) ) ;
#7131 = CARTESIAN_POINT ( 'NONE',  ( -57.87117896969294861, 2.397448601660856493, 0.9757051360025592590 ) ) ;
#7132 = CARTESIAN_POINT ( 'NONE',  ( -57.92346726745822849, 0.7446056814934959300, 1.206286704679851107 ) ) ;
#7133 = CARTESIAN_POINT ( 'NONE',  ( -16.92419414914125753, 122.6916909566506320, 0.1062714098145889491 ) ) ;
#7134 = ORIENTED_EDGE ( 'NONE', *, *, #27688, .T. ) ;
#7135 = CARTESIAN_POINT ( 'NONE',  ( -56.90927647567382763, 5.206763508130138440, -0.7605795637955022892 ) ) ;
#7136 = CARTESIAN_POINT ( 'NONE',  ( -6.974621529130486053, 121.9482818037246972, -0.2056693399646919718 ) ) ;
#7137 = EDGE_LOOP ( 'NONE', ( #28874, #22453, #40225, #13213 ) ) ;
#7138 = CARTESIAN_POINT ( 'NONE',  ( -14.60888863026623952, 79.54114996201613508, -1.524000000000001132 ) ) ;
#7139 = CARTESIAN_POINT ( 'NONE',  ( -1.569753016146457014, 156.2570369995211479, -0.1094014671735938637 ) ) ;
#7140 = CARTESIAN_POINT ( 'NONE',  ( 6.030629465787032295, -12.69248357272054228, 1.053518048143269548 ) ) ;
#7141 = CARTESIAN_POINT ( 'NONE',  ( -19.98084523315773353, 136.1824594150436383, 1.423751267309647739 ) ) ;
#7142 = CARTESIAN_POINT ( 'NONE',  ( 2.739727753987758252, 28.35525327666260864, -3.728201022356329553 ) ) ;
#7143 = CARTESIAN_POINT ( 'NONE',  ( 9.754222058523195571, 118.0373187826741486, 0.4689489433136689311 ) ) ;
#7144 = CARTESIAN_POINT ( 'NONE',  ( 1.999148240431267487, -15.70856037145330930, 5.662001806903932177 ) ) ;
#7145 = CARTESIAN_POINT ( 'NONE',  ( -2.768688662514669385, 30.30441277318858795, -3.700580903672975541 ) ) ;
#7146 = CARTESIAN_POINT ( 'NONE',  ( -0.9222101193809760789, -5.324732007522724686, 0.3213417913276819249 ) ) ;
#7147 = CARTESIAN_POINT ( 'NONE',  ( -15.38042280020276387, 120.6961994932685798, -0.5371754898667547851 ) ) ;
#7148 = FACE_OUTER_BOUND ( 'NONE', #16218, .T. ) ;
#7149 = CYLINDRICAL_SURFACE ( 'NONE', #30908, 3.175000000000001155 ) ;
#7150 = CARTESIAN_POINT ( 'NONE',  ( 8.764204663043864585, 117.8121725143452778, 0.5577289095695550092 ) ) ;
#7151 = ORIENTED_EDGE ( 'NONE', *, *, #26356, .T. ) ;
#7152 = CARTESIAN_POINT ( 'NONE',  ( -12.49185498700849806, 153.6617311634574037, 1.629683330142263520 ) ) ;
#7153 = CARTESIAN_POINT ( 'NONE',  ( -57.49410450365485303, 1.597103417522111934, -1.403138785175781944 ) ) ;
#7154 = CARTESIAN_POINT ( 'NONE',  ( 13.51395941584908478, 155.6725583577350278, 2.021746995258101975 ) ) ;
#7155 = CARTESIAN_POINT ( 'NONE',  ( 19.86924145434953815, 147.9128418260961837, -1.725515945229960213 ) ) ;
#7156 = CARTESIAN_POINT ( 'NONE',  ( 0.9053751552131774627, -6.120233167431497812, -0.3594991891349857416 ) ) ;
#7157 = CARTESIAN_POINT ( 'NONE',  ( -21.19565729220489203, 150.1117090729339623, -2.124842235463313855 ) ) ;
#7158 = CARTESIAN_POINT ( 'NONE',  ( 4.566904246663979983, 118.0741002040653171, -0.6113164951592977570 ) ) ;
#7159 = CARTESIAN_POINT ( 'NONE',  ( 4.973583767373020770, 117.3966162183443203, 0.9753880922370259388 ) ) ;
#7160 = CARTESIAN_POINT ( 'NONE',  ( 14.10444703556369817, 134.4521314832425389, -0.9547003412267361933 ) ) ;
#7161 = CARTESIAN_POINT ( 'NONE',  ( -2.836071964827412639, 121.0300505300837415, -0.05667146733340970577 ) ) ;
#7162 = ORIENTED_EDGE ( 'NONE', *, *, #7451, .T. ) ;
#7163 = CARTESIAN_POINT ( 'NONE',  ( -16.73131056987035237, 135.2943057719725459, -2.348795921478700421 ) ) ;
#7164 = CARTESIAN_POINT ( 'NONE',  ( 1.975136073220363553, -15.70315947173593685, 5.621751108460156132 ) ) ;
#7165 =( BOUNDED_SURFACE ( )  B_SPLINE_SURFACE ( 3, 2, ( 
 ( #34066, #14028, #17639 ),
 ( #7450, #17432, #4893 ),
 ( #17848, #5102, #23820 ),
 ( #24240, #30430, #30848 ),
 ( #1484, #10627, #27034 ),
 ( #36629, #40043, #27240 ),
 ( #18054, #27652, #37249 ),
 ( #854, #20407, #10836 ),
 ( #11255, #36840, #7660 ),
 ( #26825, #20618, #40255 ),
 ( #11049, #24035, #40664 ),
 ( #37050, #30641, #40465 ),
 ( #1694, #7868, #20829 ),
 ( #4682, #14440, #27450 ),
 ( #8066, #11455, #24446 ),
 ( #37450, #33437, #34274 ),
 ( #39832, #18683, #22288 ),
 ( #15069, #8696, #41080 ),
 ( #28703, #24658, #15496 ),
 ( #41292, #37872, #15698 ),
 ( #34684, #2741, #14858 ),
 ( #8490, #40870, #28285 ),
 ( #31692, #25298, #31263 ),
 ( #11671, #11888, #27862 ) ),
 .UNSPECIFIED., .F., .F., .F. ) 
 B_SPLINE_SURFACE_WITH_KNOTS ( ( 4, 2, 2, 2, 2, 2, 2, 2, 2, 2, 2, 4 ),
 ( 3, 3 ),
 ( 0.000000000000000000, 0.0005614604826171184235, 0.001122920965234236847, 0.001684381447851355379, 0.002245841930468473694, 0.003368762895702710758, 0.004491683860936947388, 0.005614604826171184018, 0.006737525791405421516, 0.007298986274022539397, 0.007860446756639657279, 0.008983367721873894776 ),
 ( 0.000000000000000000, 1.000000000000000000 ),
 .UNSPECIFIED. ) 
 GEOMETRIC_REPRESENTATION_ITEM ( )  RATIONAL_B_SPLINE_SURFACE ( (
 ( 1.000000000000000000, 0.9987193938133381854, 1.000000000000000000),
 ( 1.000000000000000000, 0.9982000373937082172, 1.000000000000000000),
 ( 1.000000000000000000, 0.9975619604998443579, 1.000000000000000000),
 ( 1.000000000000000000, 0.9916939477420071425, 1.000000000000000000),
 ( 1.000000000000000000, 0.9861209039942885335, 1.000000000000000000),
 ( 1.000000000000000000, 0.9617740169773764114, 1.000000000000000000),
 ( 1.000000000000000000, 0.9448443023870999324, 1.000000000000000000),
 ( 1.000000000000000000, 0.9146158020826528068, 1.000000000000000000),
 ( 1.000000000000000000, 0.9004045293498704750, 1.000000000000000000),
 ( 1.000000000000000000, 0.8619933248295105210, 1.000000000000000000),
 ( 1.000000000000000000, 0.8427343359447093674, 1.000000000000000000),
 ( 1.000000000000000000, 0.8121850874613311122, 1.000000000000000000),
 ( 1.000000000000000000, 0.8005416906224276374, 1.000000000000000000),
 ( 1.000000000000000000, 0.7821458849522040513, 1.000000000000000000),
 ( 1.000000000000000000, 0.7751654015739020132, 1.000000000000000000),
 ( 1.000000000000000000, 0.7626205617125327851, 1.000000000000000000),
 ( 1.000000000000000000, 0.7574054414875175389, 1.000000000000000000),
 ( 1.000000000000000000, 0.7453179101210614110, 1.000000000000000000),
 ( 1.000000000000000000, 0.7405197175301533319, 1.000000000000000000),
 ( 1.000000000000000000, 0.7299770405535720430, 1.000000000000000000),
 ( 1.000000000000000000, 0.7243132446550970549, 1.000000000000000000),
 ( 1.000000000000000000, 0.7087302219116619062, 1.000000000000000000),
 ( 1.000000000000000000, 0.7007553748513319913, 1.000000000000000000),
 ( 1.000000000000000000, 0.7072256012392703628, 1.000000000000000000) ) ) 
 REPRESENTATION_ITEM ( '' )  SURFACE ( )  );
#7166 = CARTESIAN_POINT ( 'NONE',  ( -19.68500000000000227, 71.11999999999999034, 5.079999999999997407 ) ) ;
#7167 = CARTESIAN_POINT ( 'NONE',  ( -4.636526327029984351, 118.0184740840416282, -0.8096187216592474201 ) ) ;
#7168 = CARTESIAN_POINT ( 'NONE',  ( -51.54051843738712080, 14.84038450301108192, -4.692172599169433411 ) ) ;
#7169 = EDGE_CURVE ( 'NONE', #20726, #27974, #26519, .T. ) ;
#7170 = CARTESIAN_POINT ( 'NONE',  ( 4.105025596253708997, 118.2429491485453354, 0.3532957070722724802 ) ) ;
#7171 = CARTESIAN_POINT ( 'NONE',  ( 18.14277298170000563, 148.2327041560005512, 2.387153687107330668 ) ) ;
#7172 = CARTESIAN_POINT ( 'NONE',  ( -19.68500000000000938, 71.11999999999999034, -5.080000000000000959 ) ) ;
#7173 = EDGE_CURVE ( 'NONE', #37741, #35331, #11829, .T. ) ;
#7174 = CARTESIAN_POINT ( 'NONE',  ( 23.29144772315967771, 149.3526176766912101, 0.4654185560736371352 ) ) ;
#7175 = CARTESIAN_POINT ( 'NONE',  ( -0.5381045032992836097, 19.73597684265961050, -8.428375251626778919 ) ) ;
#7176 = CARTESIAN_POINT ( 'NONE',  ( 3.646880827531659985, 120.8687762150871379, 0.3676761613455565847 ) ) ;
#7177 = CARTESIAN_POINT ( 'NONE',  ( 22.55548643167949052, 142.2972183020237367, -0.7396483830486684230 ) ) ;
#7178 = EDGE_CURVE ( 'NONE', #4929, #26503, #978, .T. ) ;
#7179 = CARTESIAN_POINT ( 'NONE',  ( -43.06611735332000279, 21.60822042109159824, -2.043235477782531007 ) ) ;
#7180 = B_SPLINE_CURVE_WITH_KNOTS ( 'NONE', 3,
 ( #29530, #26323, #368, #35931, #25491, #12498 ),
 .UNSPECIFIED., .F., .F.,
 ( 4, 2, 4 ),
 ( 0.000000000000000000, 0.5000000000000000000, 1.000000000000000000 ),
 .UNSPECIFIED. ) ;
#7181 = ORIENTED_EDGE ( 'NONE', *, *, #29229, .T. ) ;
#7182 = LINE ( 'NONE', #11185, #2505 ) ;
#7183 = EDGE_CURVE ( 'NONE', #38737, #32933, #35658, .T. ) ;
#7184 = CARTESIAN_POINT ( 'NONE',  ( -20.69815783549640642, 152.5608647341385335, -0.3383848979192931039 ) ) ;
#7185 = ORIENTED_EDGE ( 'NONE', *, *, #28499, .T. ) ;
#7186 = CARTESIAN_POINT ( 'NONE',  ( 8.076851222567801969, 121.3085770623402624, -0.9248642372525653910 ) ) ;
#7187 = CARTESIAN_POINT ( 'NONE',  ( -46.60530155212504155, 26.17382724835477958, -1.270000000000008455 ) ) ;
#7188 = CARTESIAN_POINT ( 'NONE',  ( -11.90976107009722362, 151.9662372315928280, -0.6611612027286482007 ) ) ;
#7189 = CARTESIAN_POINT ( 'NONE',  ( 4.284293204009990141, -11.98693494109343050, 1.176118521537933725 ) ) ;
#7190 = EDGE_CURVE ( 'NONE', #22599, #25412, #11165, .T. ) ;
#7191 = CARTESIAN_POINT ( 'NONE',  ( -21.81261666999477100, 141.9756885651356413, 1.158660305423542924 ) ) ;
#7192 = DIRECTION ( 'NONE',  ( 0.9998004120163608288, 0.000000000000000000, 0.01997839162482749342 ) ) ;
#7193 = CARTESIAN_POINT ( 'NONE',  ( -0.0008202526018423079166, 159.6052337359418800, 0.04104879434819973250 ) ) ;
#7194 = ORIENTED_EDGE ( 'NONE', *, *, #24223, .T. ) ;
#7195 = CARTESIAN_POINT ( 'NONE',  ( 0.05711764529616595448, 0.5181683540770932739, -4.631227783250111862 ) ) ;
#7196 = CARTESIAN_POINT ( 'NONE',  ( 2.745104810890289126, 105.1243892088056100, 4.583589704686842126 ) ) ;
#7197 = CARTESIAN_POINT ( 'NONE',  ( -13.85159022459153988, 59.63164443796365077, -5.016499999999999737 ) ) ;
#7198 = CARTESIAN_POINT ( 'NONE',  ( -6.484670282503085616E-14, 71.97546620154574271, 3.533028205012241021E-29 ) ) ;
#7199 = CARTESIAN_POINT ( 'NONE',  ( -8.289732393230972107, 120.2889636526078903, 1.114899670313132862 ) ) ;
#7200 = CARTESIAN_POINT ( 'NONE',  ( -4.598078022480850180, -10.86695742004451404, -0.5832510952623800593 ) ) ;
#7201 = CARTESIAN_POINT ( 'NONE',  ( 15.04114430247500245, 121.6710330000183546, 1.338242383117114853 ) ) ;
#7202 = CARTESIAN_POINT ( 'NONE',  ( -58.60951264191635346, -0.2527965749311716914, -0.4344104473673510713 ) ) ;
#7204 = CARTESIAN_POINT ( 'NONE',  ( 4.077592138694859258, 118.2594131075661608, -0.7845094026950484301 ) ) ;
#7203 = CARTESIAN_POINT ( 'NONE',  ( 5.860279866612397193, 56.51500000000084611, 5.019549989587896555 ) ) ;
#7205 = CARTESIAN_POINT ( 'NONE',  ( -3.538659794179211726, -11.74154716455626257, -2.972011832598964176 ) ) ;
#7206 = CARTESIAN_POINT ( 'NONE',  ( -7.741078003750668124, 158.6130819278358501, -0.9685178112996217781 ) ) ;
#7207 = EDGE_LOOP ( 'NONE', ( #14436, #2489, #22808, #3113 ) ) ;
#7208 = CARTESIAN_POINT ( 'NONE',  ( -6.107944937931588214, 155.3491548655973133, 0.3423801154807231684 ) ) ;
#7209 = CARTESIAN_POINT ( 'NONE',  ( 2.853125897180512460, -15.37704012655945185, 5.752692477956393269 ) ) ;
#7210 = DIRECTION ( 'NONE',  ( -0.8745520943968253524, 0.4849315768086530087, -8.537024980200771528E-16 ) ) ;
#7211 = CARTESIAN_POINT ( 'NONE',  ( -10.84307050033138431, 78.30450799593342026, -1.269999999999998685 ) ) ;
#7213 = EDGE_LOOP ( 'NONE', ( #16501, #27693, #30758, #5843 ) ) ;
#7212 = CIRCLE ( 'NONE', #6530, 0.5080000000000000071 ) ;
#7214 = CARTESIAN_POINT ( 'NONE',  ( 18.97962326299249014, 149.2349160008635351, 2.496544457321506094 ) ) ;
#7215 = CARTESIAN_POINT ( 'NONE',  ( 0.000000000000000000, -2.099656937138137170E-16, 0.000000000000000000 ) ) ;
#7216 = CARTESIAN_POINT ( 'NONE',  ( -46.78618054628500289, 25.31127283853226828, -1.744542934675088919 ) ) ;
#7217 = CARTESIAN_POINT ( 'NONE',  ( -19.19817178191696172, 128.6826163344482268, 0.7403421610261617936 ) ) ;
#7218 = CARTESIAN_POINT ( 'NONE',  ( -7.074087999897446188, 26.91573472731666783, -4.615267515785972385 ) ) ;
#7219 = CARTESIAN_POINT ( 'NONE',  ( 15.17477609654683590, 139.4722935914273307, 1.590378199732649822 ) ) ;
#7220 = CARTESIAN_POINT ( 'NONE',  ( 14.60357043488709650, 120.3300541288867862, -0.1192926189779471569 ) ) ;
#7221 = FACE_OUTER_BOUND ( 'NONE', #15518, .T. ) ;
#7222 = CARTESIAN_POINT ( 'NONE',  ( -57.91918631225849623, 0.6797522236637953963, 0.9623354101195258359 ) ) ;
#7223 = CARTESIAN_POINT ( 'NONE',  ( -47.07934102874912696, 22.98505637820354153, 3.579966862081923828 ) ) ;
#7225 = ADVANCED_FACE ( 'NONE', ( #35541 ), #5076, .T. ) ;
#7224 = CARTESIAN_POINT ( 'NONE',  ( 3.372434712493016296, 108.0380779545110812, -4.123874089241533980 ) ) ;
#7226 = CARTESIAN_POINT ( 'NONE',  ( -55.65298819915649631, 5.540485941798511504, 2.823722248809245272 ) ) ;
#7227 = CARTESIAN_POINT ( 'NONE',  ( -57.86763781102449400, 1.347252755066737473, 1.494140885802228924 ) ) ;
#7228 = CARTESIAN_POINT ( 'NONE',  ( -4.486143021922693208, 118.1136361874718688, 0.5725959421912928393 ) ) ;
#7229 = CARTESIAN_POINT ( 'NONE',  ( -58.37241122568488549, -0.2962816677227753104, -1.028586707908062104E-14 ) ) ;
#7230 = ORIENTED_EDGE ( 'NONE', *, *, #17045, .F. ) ;
#7231 = CARTESIAN_POINT ( 'NONE',  ( -24.23745918283205114, 82.38670122043342303, -1.270000000000006457 ) ) ;
#7232 = CARTESIAN_POINT ( 'NONE',  ( 3.927402275990105718, 119.0434425390719326, -0.7708394141866733440 ) ) ;
#7233 = CARTESIAN_POINT ( 'NONE',  ( -0.6688473404179187121, 105.9455060897651748, -5.311925200740537534 ) ) ;
#7234 = CARTESIAN_POINT ( 'NONE',  ( 4.642283747215392609, 118.0244654425472959, 0.7555977772639859147 ) ) ;
#7235 = CARTESIAN_POINT ( 'NONE',  ( -16.27374876192092401, 146.7930872653447523, -1.439762483169732432 ) ) ;
#7236 = CARTESIAN_POINT ( 'NONE',  ( -0.6864567890905972636, 115.7029491485453718, -1.757685328908172195 ) ) ;
#7237 = CARTESIAN_POINT ( 'NONE',  ( 2.010775290776205981, 117.9496054473550402, -1.283640624249119622 ) ) ;
#7238 = CARTESIAN_POINT ( 'NONE',  ( 5.239928853181306856, 115.4398124677065596, -1.307349544149847720 ) ) ;
#7239 = CARTESIAN_POINT ( 'NONE',  ( -0.5523667267585495866, 120.0661220204379305, -0.4484973920728141938 ) ) ;
#7240 = CARTESIAN_POINT ( 'NONE',  ( -0.1506890447697080415, 104.6144662015457527, 6.108955356427616223 ) ) ;
#7241 = CARTESIAN_POINT ( 'NONE',  ( -13.99440778436217592, 79.95103047660883533, 1.269999999999998241 ) ) ;
#7242 = VECTOR ( 'NONE', #37795, 1000.000000000000000 ) ;
#7243 = CARTESIAN_POINT ( 'NONE',  ( 7.895606690698700802, 122.1535174891448321, -0.5249436039529056242 ) ) ;
#7244 = CARTESIAN_POINT ( 'NONE',  ( -10.91351724380642096, 127.9361551302125832, -0.05936199999560100304 ) ) ;
#7245 = DIRECTION ( 'NONE',  ( 0.9998004120163610509, 4.016384292689131511E-17, 0.01997839162482749689 ) ) ;
#7246 = CARTESIAN_POINT ( 'NONE',  ( 16.55455218413301210, 122.7279807066903032, 1.056987703419675961 ) ) ;
#7247 = CARTESIAN_POINT ( 'NONE',  ( 5.284239755522298410, 105.1224178746987121, -0.8069738050709613919 ) ) ;
#7248 = CARTESIAN_POINT ( 'NONE',  ( 3.238076882636043763, -14.77659300283332122, 2.967476587227507956 ) ) ;
#7249 = CARTESIAN_POINT ( 'NONE',  ( -10.78346871132534979, 121.7859837122882283, 1.235232998807844096 ) ) ;
#7250 = CARTESIAN_POINT ( 'NONE',  ( -0.8533247626149625953, -2.668348290978065140, -0.4694259674561338525 ) ) ;
#7251 = CARTESIAN_POINT ( 'NONE',  ( -9.693497654998228796, 118.1218853900603136, -0.6301662642801911796 ) ) ;
#7252 = CARTESIAN_POINT ( 'NONE',  ( -0.9742996550080020857, -5.754034560434002188, 0.05241923913101136784 ) ) ;
#7253 = VERTEX_POINT ( 'NONE', #39155 ) ;
#7254 = CARTESIAN_POINT ( 'NONE',  ( -41.35393432493753352, 22.77111593294431913, 0.9171044195162014745 ) ) ;
#7255 = CARTESIAN_POINT ( 'NONE',  ( 5.090087584496979289, 118.2545999410811106, 0.7183934583778605054 ) ) ;
#7256 = CARTESIAN_POINT ( 'NONE',  ( -8.258026456251933212, 154.6505398758502849, 0.7900859392159014227 ) ) ;
#7257 = CARTESIAN_POINT ( 'NONE',  ( 4.342152980699533593, -13.79257992285246104, 4.116713196511041950 ) ) ;
#7258 = CARTESIAN_POINT ( 'NONE',  ( 6.588241325444229801, 120.6599796251122427, -0.8186057014055779790 ) ) ;
#7259 = CARTESIAN_POINT ( 'NONE',  ( -1.258058525836236230, 118.8689652838214244, -0.6902481975293248695 ) ) ;
#7260 = CARTESIAN_POINT ( 'NONE',  ( -0.8468149500740962399, 104.6144662015457243, 4.761320282458491704 ) ) ;
#7261 = CARTESIAN_POINT ( 'NONE',  ( 3.221735024265227398, -14.36526069886394730, 2.718910799868354378 ) ) ;
#7262 = CARTESIAN_POINT ( 'NONE',  ( -4.771056762337200219, 117.4047813638584188, -1.203986021773440385 ) ) ;
#7263 = CARTESIAN_POINT ( 'NONE',  ( 10.33307603652738038, 126.0505730134521230, 0.02860894079130328269 ) ) ;
#7264 = EDGE_LOOP ( 'NONE', ( #36160, #19631, #15253, #31115 ) ) ;
#7265 = CARTESIAN_POINT ( 'NONE',  ( -3.324521368350398909, 108.2676741415845640, 4.163358009128126369 ) ) ;
#7266 = CARTESIAN_POINT ( 'NONE',  ( 2.372169177973964871, 106.9236017804880134, 4.772346225205962966 ) ) ;
#7267 = DIRECTION ( 'NONE',  ( 0.9998004120163609398, 0.000000000000000000, 0.01997839162482749689 ) ) ;
#7268 = CARTESIAN_POINT ( 'NONE',  ( 12.21488373879589240, 55.24500000000000455, 5.016499999999999737 ) ) ;
#7269 = VECTOR ( 'NONE', #22840, 1000.000000000000000 ) ;
#7270 = CARTESIAN_POINT ( 'NONE',  ( 6.904872195170157489, 117.1762911274595496, 0.05199240921585736308 ) ) ;
#7271 = CARTESIAN_POINT ( 'NONE',  ( -5.239928853181434754, 115.4398124677065596, 1.307349544149847942 ) ) ;
#7272 = CARTESIAN_POINT ( 'NONE',  ( 1.847049442607983316, -15.63718699515584376, 5.492472997249506328 ) ) ;
#7273 = CARTESIAN_POINT ( 'NONE',  ( -17.65389921742010060, 84.42347906515803402, -1.270000000000003348 ) ) ;
#7274 = CARTESIAN_POINT ( 'NONE',  ( -3.137464277621155873, 31.48680077624217688, 0.6829839861511678434 ) ) ;
#7275 = CARTESIAN_POINT ( 'NONE',  ( 12.61233984701546440, 121.4495935343099688, 1.683034450629873779 ) ) ;
#7276 = CARTESIAN_POINT ( 'NONE',  ( -4.556403025205056245, 17.84477460162305107, -0.8067276567318153457 ) ) ;
#7277 = CARTESIAN_POINT ( 'NONE',  ( -8.190863557275731566, 21.65400946394957060, -2.068261358883292989 ) ) ;
#7278 = CARTESIAN_POINT ( 'NONE',  ( 2.507300275874562168, 117.4827359074439670, -0.6436947651051395658 ) ) ;
#7279 = CARTESIAN_POINT ( 'NONE',  ( -2.311675797007805677, 124.5312663981120380, -0.07107509915817145085 ) ) ;
#7280 = CARTESIAN_POINT ( 'NONE',  ( 4.880791232649782430, 117.4111470503218584, 1.144768225355988545 ) ) ;
#7281 = DIRECTION ( 'NONE',  ( -5.188838149069472160E-16, 1.699382548006136559E-16, 1.000000000000000000 ) ) ;
#7282 = CARTESIAN_POINT ( 'NONE',  ( -0.008700780990417026142, 121.2597428844645293, 0.4354226598342535448 ) ) ;
#7283 = AXIS2_PLACEMENT_3D ( 'NONE', #39689, #10902, #4124 ) ;
#7284 = CARTESIAN_POINT ( 'NONE',  ( 3.263621351691376571, 8.939281053574255509, -3.290156819607050753 ) ) ;
#7285 = DIRECTION ( 'NONE',  ( -1.000000000000000000, 0.000000000000000000, 0.000000000000000000 ) ) ;
#7286 = CARTESIAN_POINT ( 'NONE',  ( 2.120958618816386920, -15.04726689571640819, 5.287964242625700528 ) ) ;
#7287 = CARTESIAN_POINT ( 'NONE',  ( 0.5697667371461264674, 106.2969274751293938, -5.150121607182108541 ) ) ;
#7288 = CARTESIAN_POINT ( 'NONE',  ( -15.21238092238761297, 121.1469641333237917, 0.4626880538419669842 ) ) ;
#7289 = DIRECTION ( 'NONE',  ( 5.188838149069472160E-16, -1.699382548006136559E-16, -1.000000000000000000 ) ) ;
#7290 = DIRECTION ( 'NONE',  ( 0.3256999990547897461, 0.9454731675810318370, 0.000000000000000000 ) ) ;
#7291 = VECTOR ( 'NONE', #19971, 999.9999999999998863 ) ;
#7292 = ORIENTED_EDGE ( 'NONE', *, *, #14987, .F. ) ;
#7293 = CARTESIAN_POINT ( 'NONE',  ( -5.266611731650901795, 115.7029491485453434, 0.8691344147197622716 ) ) ;
#7294 = CARTESIAN_POINT ( 'NONE',  ( 2.197863461560763287, -15.74995721546218519, 5.600911867769769792 ) ) ;
#7295 = CARTESIAN_POINT ( 'NONE',  ( -19.99643065938096598, 145.3736917597469471, 1.717600817134501856 ) ) ;
#7296 = CARTESIAN_POINT ( 'NONE',  ( 20.26345141861404642, 136.2683111393718320, -1.346723181737012442 ) ) ;
#7297 = CARTESIAN_POINT ( 'NONE',  ( 0.9303216910925710126, 27.28174836166085981, 0.2932329443217298603 ) ) ;
#7298 = CARTESIAN_POINT ( 'NONE',  ( -58.61721026093515263, -0.2672633658392670197, -0.4124697875294594529 ) ) ;
#7299 = EDGE_LOOP ( 'NONE', ( #2818, #30961, #41985, #9159 ) ) ;
#7300 = DIRECTION ( 'NONE',  ( 0.000000000000000000, 0.000000000000000000, 1.000000000000000000 ) ) ;
#7301 = CIRCLE ( 'NONE', #36553, 0.6349999999999970113 ) ;
#7302 = CARTESIAN_POINT ( 'NONE',  ( 0.2537530607703858410, 113.0327356262573915, 2.627782494400416002 ) ) ;
#7303 = PRESENTATION_STYLE_ASSIGNMENT (( #36482 ) ) ;
#7304 = CARTESIAN_POINT ( 'NONE',  ( -16.73823235880720617, 147.9788754379930822, 1.246688593732825812 ) ) ;
#7305 = CARTESIAN_POINT ( 'NONE',  ( 0.7543369490868296889, 118.1473330535139041, 0.9261446413320308935 ) ) ;
#7306 = CARTESIAN_POINT ( 'NONE',  ( 17.49586834669421620, 149.8167423968465073, -1.704004628023328083 ) ) ;
#7307 = CARTESIAN_POINT ( 'NONE',  ( -20.51324802173768802, 148.8605967840894095, -2.436527653975322227 ) ) ;
#7308 = DIRECTION ( 'NONE',  ( 0.9816537812491092918, 0.1906721105965052399, 1.574460549389967402E-15 ) ) ;
#7309 = CARTESIAN_POINT ( 'NONE',  ( 4.284053485260008287, 118.2131419831110577, -0.3606587761694292071 ) ) ;
#7310 = CARTESIAN_POINT ( 'NONE',  ( 3.061305989504062630, 156.1243923452879017, -0.5262318146843658617 ) ) ;
#7311 = ORIENTED_EDGE ( 'NONE', *, *, #23787, .T. ) ;
#7312 = CARTESIAN_POINT ( 'NONE',  ( 2.944601773672358203, -15.01875103642165499, 4.065120351795452613 ) ) ;
#7313 = CARTESIAN_POINT ( 'NONE',  ( 5.223521521431373493, 105.1221584262004143, -1.132698478535189901 ) ) ;
#7314 = CIRCLE ( 'NONE', #6611, 5.080000000000006288 ) ;
#7315 = CARTESIAN_POINT ( 'NONE',  ( -47.84756666395260538, 19.38928433903618043, 5.209054514891976240 ) ) ;
#7316 = CARTESIAN_POINT ( 'NONE',  ( -2.168033660621066172, 0.5777166996233511487, 4.103230905123370853 ) ) ;
#7317 = CARTESIAN_POINT ( 'NONE',  ( 14.96631152213282689, 150.5987129668814077, 1.974168424754894957 ) ) ;
#7318 = CARTESIAN_POINT ( 'NONE',  ( -1.750334050913927353, 31.14778888712128690, 2.093020893977926900 ) ) ;
#7319 = EDGE_CURVE ( 'NONE', #1073, #6137, #14271, .T. ) ;
#7320 = CARTESIAN_POINT ( 'NONE',  ( -2.136650056307613621, 10.86338872207680950, -4.114640003288728920 ) ) ;
#7321 = CARTESIAN_POINT ( 'NONE',  ( 7.577119205441340988, 122.4179301937671767, 0.2905534069474317582 ) ) ;
#7322 = CARTESIAN_POINT ( 'NONE',  ( -4.755271767586297216, 111.7583057171730729, 2.489475493475922452 ) ) ;
#7323 = VECTOR ( 'NONE', #17892, 1000.000000000000000 ) ;
#7324 = CARTESIAN_POINT ( 'NONE',  ( -53.87733401397680666, 8.744676589845553849, -2.811092830483142180 ) ) ;
#7325 = CARTESIAN_POINT ( 'NONE',  ( -8.790230331137980357, 117.7071499903595821, -0.3330531770478057929 ) ) ;
#7326 = DIRECTION ( 'NONE',  ( -0.5149185422762221354, 0.8572391118119438991, -4.128606161907600514E-16 ) ) ;
#7327 = FACE_OUTER_BOUND ( 'NONE', #15408, .T. ) ;
#7328 = DIRECTION ( 'NONE',  ( -5.188838149069472160E-16, 1.699382548006136559E-16, 1.000000000000000000 ) ) ;
#7329 = CARTESIAN_POINT ( 'NONE',  ( -29.24397885281356224, 65.27318422236749029, -1.270000000000006013 ) ) ;
#7330 = CARTESIAN_POINT ( 'NONE',  ( 2.958531772299235918, 50.13146620154573441, 1.329372033065076453 ) ) ;
#7331 = CYLINDRICAL_SURFACE ( 'NONE', #17121, 2.540000000000000480 ) ;
#7332 = LINE ( 'NONE', #39715, #26654 ) ;
#7333 = CARTESIAN_POINT ( 'NONE',  ( -58.33482727260580702, 1.278009831241974759, -1.064229179957365390E-14 ) ) ;
#7334 = CARTESIAN_POINT ( 'NONE',  ( 0.08519874065564590759, 108.5751225745497948, -4.263693374914214296 ) ) ;
#7335 = CARTESIAN_POINT ( 'NONE',  ( -15.11282490002057877, 156.1437908837410191, 0.09152821140687306123 ) ) ;
#7336 = ORIENTED_EDGE ( 'NONE', *, *, #17814, .T. ) ;
#7337 = CARTESIAN_POINT ( 'NONE',  ( -57.80399136194962040, 2.779771081967835400, -0.2452555687351754832 ) ) ;
#7338 = CARTESIAN_POINT ( 'NONE',  ( 6.980895880038317181, 121.9518852483956124, 0.06772288494938194514 ) ) ;
#7339 = ORIENTED_EDGE ( 'NONE', *, *, #9157, .F. ) ;
#7340 = CARTESIAN_POINT ( 'NONE',  ( -14.21338345945963688, 79.68069512491149453, -1.524000000000000909 ) ) ;
#7341 = CARTESIAN_POINT ( 'NONE',  ( -0.6411011158480280914, 120.9975462804897433, -0.03814546805551050079 ) ) ;
#7342 = CARTESIAN_POINT ( 'NONE',  ( 3.842082824490853810, -15.33115451161810938, 5.194229279690915746 ) ) ;
#7343 = CARTESIAN_POINT ( 'NONE',  ( -10.59408866556495532, 119.9085704333771787, 1.028430606607102948 ) ) ;
#7344 = CARTESIAN_POINT ( 'NONE',  ( -2.614655561276646889, 23.60746518810343630, 3.812863311767609620 ) ) ;
#7345 = CARTESIAN_POINT ( 'NONE',  ( 1.853717367163155050, 116.5907236856068181, 0.2192087907590279383 ) ) ;
#7346 = TOROIDAL_SURFACE ( 'NONE', #24999, 0.3810000000000001719, 0.2540000000000000036 ) ;
#7347 = CARTESIAN_POINT ( 'NONE',  ( 11.82635486671713743, 152.0554279321345064, 0.4236511662767659669 ) ) ;
#7348 = CARTESIAN_POINT ( 'NONE',  ( -33.42971872652992005, 49.93539301574497102, 1.269999999999992690 ) ) ;
#7349 = CARTESIAN_POINT ( 'NONE',  ( 0.2615529312792121419, 0.9453775857588032627, -0.9394305312888860948 ) ) ;
#7350 = CARTESIAN_POINT ( 'NONE',  ( -15.78464309758879835, 121.0087326939336378, -0.5477818752361016674 ) ) ;
#7351 = CARTESIAN_POINT ( 'NONE',  ( -18.35410564743290607, 77.35382415001784295, -1.904999999999999583 ) ) ;
#7352 = LINE ( 'NONE', #1177, #22047 ) ;
#7353 = CARTESIAN_POINT ( 'NONE',  ( -2.238353053745737231, 116.2832059125415896, 0.1037362710514463521 ) ) ;
#7354 = CARTESIAN_POINT ( 'NONE',  ( -15.94706863659619778, 135.0473088626721392, 1.554726643320765378 ) ) ;
#7355 = CARTESIAN_POINT ( 'NONE',  ( -57.78008333914727501, 0.9803893178324115665, -1.120514846177007584 ) ) ;
#7356 = CARTESIAN_POINT ( 'NONE',  ( 1.172210521474222666, 158.9035955689636523, 1.423060353815112311 ) ) ;
#7357 = CARTESIAN_POINT ( 'NONE',  ( 19.22223103763152352, 149.5120288530235655, -1.725574580128898639 ) ) ;
#7358 = CARTESIAN_POINT ( 'NONE',  ( -0.8332992110815757858, -10.66407516643697306, 0.5056687530665907593 ) ) ;
#7359 = CARTESIAN_POINT ( 'NONE',  ( -13.04750228320310157, 121.1598417376693533, -1.575122625318853053 ) ) ;
#7360 = CARTESIAN_POINT ( 'NONE',  ( 4.532710609442922589, 118.0666091547772396, -0.6408898899164870988 ) ) ;
#7361 = CARTESIAN_POINT ( 'NONE',  ( -48.21404017327530767, 19.06235592689615288, -5.351320745402601275 ) ) ;
#7362 = CARTESIAN_POINT ( 'NONE',  ( 5.032731182891235555, 105.1218460117307387, 1.777745822249493957 ) ) ;
#7363 = ADVANCED_FACE ( 'NONE', ( #38944 ), #4391, .T. ) ;
#7364 = CARTESIAN_POINT ( 'NONE',  ( 9.666892607209371491, 123.4354624054469980, -0.6853163995640744188 ) ) ;
#7365 = CARTESIAN_POINT ( 'NONE',  ( 7.805882608899723962, 122.5029464779834427, 0.4967789704017860908 ) ) ;
#7366 = ORIENTED_EDGE ( 'NONE', *, *, #27896, .F. ) ;
#7367 = CARTESIAN_POINT ( 'NONE',  ( -3.311752042447871691, 119.2933411826354728, -0.8767012952321083796 ) ) ;
#7368 = CARTESIAN_POINT ( 'NONE',  ( 4.076841989731768479, -15.73006006892005360, 3.802225825406736259 ) ) ;
#7369 = CARTESIAN_POINT ( 'NONE',  ( -24.32950799593924884, 77.42192949967211746, 1.269999999999993578 ) ) ;
#7370 = CARTESIAN_POINT ( 'NONE',  ( -4.572062116902815276, 118.0791223117457207, -0.7157013623424338666 ) ) ;
#7371 = CARTESIAN_POINT ( 'NONE',  ( -50.11792632901008915, 17.09067799859288783, -5.048577231237582730 ) ) ;
#7372 = CARTESIAN_POINT ( 'NONE',  ( 4.110706825855569235, 118.2429491485453497, 0.3474105799464941580 ) ) ;
#7373 = CARTESIAN_POINT ( 'NONE',  ( 14.16178827078151237, 152.6618899727951089, 2.241469232429742942 ) ) ;
#7374 = DIRECTION ( 'NONE',  ( -0.5149185422762221354, 0.8572391118119438991, -4.128606161907600514E-16 ) ) ;
#7375 = CARTESIAN_POINT ( 'NONE',  ( 15.96050253218456838, 121.0385544001969436, 0.3018840724360823957 ) ) ;
#7376 = CARTESIAN_POINT ( 'NONE',  ( 7.419718609332475623, 16.48482641057854892, 3.982871883899435250 ) ) ;
#7377 = CARTESIAN_POINT ( 'NONE',  ( 6.141611553833064896, 155.3548635187015350, 0.6951709773850852647 ) ) ;
#7378 = CARTESIAN_POINT ( 'NONE',  ( 0.006942562093227406909, 117.0978366787122127, -0.3474341964894883672 ) ) ;
#7379 = CARTESIAN_POINT ( 'NONE',  ( -45.05484530740422144, 21.03919035317145259, -3.644944174416286042 ) ) ;
#7380 = CARTESIAN_POINT ( 'NONE',  ( 0.6719655926374001886, 115.6909491485452719, 1.760269452045342131 ) ) ;
#7381 = PRODUCT_DEFINITION_CONTEXT ( 'detailed design', #9918, 'design' ) ;
#7382 = EDGE_CURVE ( 'NONE', #13050, #8692, #22932, .T. ) ;
#7383 = CARTESIAN_POINT ( 'NONE',  ( -16.85745507829919276, 155.2173118157008673, -0.2667832593600951707 ) ) ;
#7384 = ORIENTED_EDGE ( 'NONE', *, *, #8269, .T. ) ;
#7385 = CARTESIAN_POINT ( 'NONE',  ( 8.106904764074545966, 121.1661902519200282, -0.9676739013972032177 ) ) ;
#7386 = CARTESIAN_POINT ( 'NONE',  ( -46.84426172109978381, 25.74287342672571910, -1.326046531036418452 ) ) ;
#7387 = DIRECTION ( 'NONE',  ( -0.8745520943968243532, 0.4849315768086547296, -5.361993529360573944E-16 ) ) ;
#7388 = CARTESIAN_POINT ( 'NONE',  ( -5.901573779631426042, 121.4708175001875077, -0.3521552259516173566 ) ) ;
#7389 = CARTESIAN_POINT ( 'NONE',  ( 4.362034286260056071, -13.41731938665795276, 3.520857194803681534 ) ) ;
#7390 = CARTESIAN_POINT ( 'NONE',  ( -12.68208805480606394, 156.8164516032445306, 1.015108139269342624 ) ) ;
#7391 = CARTESIAN_POINT ( 'NONE',  ( -7.213960532367465817, 78.77618639008778700, -1.904999999999999583 ) ) ;
#7392 = CARTESIAN_POINT ( 'NONE',  ( 22.66113959641428366, 150.6410255081855212, 0.5295512721432398262 ) ) ;
#7393 = ORIENTED_EDGE ( 'NONE', *, *, #730, .F. ) ;
#7394 = CARTESIAN_POINT ( 'NONE',  ( -1.825063964020108065, -4.879331645356781877, 4.256838567046823840 ) ) ;
#7395 = CARTESIAN_POINT ( 'NONE',  ( -22.53492722140454774, 150.7843406352268687, -0.4757920170715050912 ) ) ;
#7396 = CARTESIAN_POINT ( 'NONE',  ( 13.34576682144454196, 17.14499999999997115, 5.016499999999998849 ) ) ;
#7397 = DIRECTION ( 'NONE',  ( 0.8745520943968235761, -0.4849315768086558398, 4.268512490100410909E-16 ) ) ;
#7398 = ORIENTED_EDGE ( 'NONE', *, *, #20106, .T. ) ;
#7399 = CARTESIAN_POINT ( 'NONE',  ( -6.473090125947880580, 119.6242553686945058, 1.000010245827238409 ) ) ;
#7400 = EDGE_CURVE ( 'NONE', #22739, #15866, #40434, .T. ) ;
#7401 =( BOUNDED_SURFACE ( )  B_SPLINE_SURFACE ( 3, 2, ( 
 ( #1767, #14728, #24521 ),
 ( #25384, #28152, #21741 ),
 ( #5387, #8989, #38387 ),
 ( #41375, #37743, #41587 ) ),
 .UNSPECIFIED., .F., .F., .T. ) 
 B_SPLINE_SURFACE_WITH_KNOTS ( ( 4, 4 ),
 ( 3, 3 ),
 ( -1.135597912584696071E-06, 0.0001904019166766824050 ),
 ( 0.000000000000000000, 0.2833440467634030790 ),
 .UNSPECIFIED. ) 
 GEOMETRIC_REPRESENTATION_ITEM ( )  RATIONAL_B_SPLINE_SURFACE ( (
 ( 1.000000000000000000, 0.9321124567126647387, 0.9026959759050480203),
 ( 1.000000000000000000, 0.9321124565380634053, 0.9026959756547898728),
 ( 1.000000000000000000, 0.9321125502981708610, 0.9026961100422681294),
 ( 1.000000000000000000, 0.9321126250856475171, 0.9026962172360489811) ) ) 
 REPRESENTATION_ITEM ( '' )  SURFACE ( )  );
#7402 = CARTESIAN_POINT ( 'NONE',  ( -1.722957355399680202, -2.895624787512894649, -4.295268622497145472 ) ) ;
#7403 = CARTESIAN_POINT ( 'NONE',  ( 21.70861548485252968, 150.3096123636779566, 1.869307503447338537 ) ) ;
#7404 = CARTESIAN_POINT ( 'NONE',  ( -50.01754050906186677, 16.20622680599536025, -4.878148848507119162 ) ) ;
#7406 = CARTESIAN_POINT ( 'NONE',  ( 20.75082247216783671, 147.7542213611591535, -1.617965925928341875 ) ) ;
#7405 = FACE_OUTER_BOUND ( 'NONE', #32257, .T. ) ;
#7407 = CARTESIAN_POINT ( 'NONE',  ( 2.459658384930404118, -7.418532284756778949, 3.912982838641719141 ) ) ;
#7408 = CARTESIAN_POINT ( 'NONE',  ( -10.42794149288038952, 157.8855781193960297, -1.079236549925195465 ) ) ;
#7409 = ORIENTED_EDGE ( 'NONE', *, *, #26494, .T. ) ;
#7410 = ORIENTED_EDGE ( 'NONE', *, *, #13888, .T. ) ;
#7411 = CARTESIAN_POINT ( 'NONE',  ( -7.598614292646969304, 122.4062900713904440, 0.04802449110505829788 ) ) ;
#7412 = EDGE_CURVE ( 'NONE', #41143, #4125, #35328, .T. ) ;
#7414 = CARTESIAN_POINT ( 'NONE',  ( 5.253792623460133981, -14.56763799980149976, 3.797339299194151696 ) ) ;
#7413 = CIRCLE ( 'NONE', #6706, 0.5080000000000002292 ) ;
#7415 = AXIS2_PLACEMENT_3D ( 'NONE', #9823, #22789, #18771 ) ;
#7416 = CARTESIAN_POINT ( 'NONE',  ( -3.590474171207809651E-14, 56.51499999999999346, 0.000000000000000000 ) ) ;
#7417 = ADVANCED_FACE ( 'NONE', ( #26153 ), #29350, .T. ) ;
#7418 = CARTESIAN_POINT ( 'NONE',  ( 1.400628584307200167E-15, 13.84300000000000352, 0.000000000000000000 ) ) ;
#7419 = ORIENTED_EDGE ( 'NONE', *, *, #22679, .T. ) ;
#7420 = CARTESIAN_POINT ( 'NONE',  ( 8.661198069469437044, 120.2102557752085232, 1.489220423754913369 ) ) ;
#7421 = CARTESIAN_POINT ( 'NONE',  ( 4.902823790339319032, 117.6536153060737320, 0.9411696025594519233 ) ) ;
#7422 = CARTESIAN_POINT ( 'NONE',  ( -6.564189886853176475E-14, 81.62746620154572952, -5.847435218134868453E-18 ) ) ;
#7423 = CARTESIAN_POINT ( 'NONE',  ( -22.59612908711474688, 148.7221180073953235, 0.8559155618276412802 ) ) ;
#7424 = CARTESIAN_POINT ( 'NONE',  ( 5.986726992493722754, 14.59627609256335923, -5.926391003037220884 ) ) ;
#7425 = CARTESIAN_POINT ( 'NONE',  ( 2.668671847104294947, 120.5579296053302727, 0.4429723278990745916 ) ) ;
#7426 = DIRECTION ( 'NONE',  ( 6.353134868986659519E-16, -1.000000000000000000, 0.000000000000000000 ) ) ;
#7427 = EDGE_CURVE ( 'NONE', #24767, #30889, #9795, .T. ) ;
#7428 = CARTESIAN_POINT ( 'NONE',  ( 14.42641459765130030, 120.3907653763288579, -0.3011401359519874088 ) ) ;
#7429 = DIRECTION ( 'NONE',  ( -0.1906721105965055174, 0.9816537812491091808, 0.000000000000000000 ) ) ;
#7430 = CARTESIAN_POINT ( 'NONE',  ( -53.60911972597136810, 9.592866957671235539, 3.621504120778383129 ) ) ;
#7431 = CARTESIAN_POINT ( 'NONE',  ( -47.36975192132250356, 22.26287704218617236, 3.814390537888098009 ) ) ;
#7432 = CARTESIAN_POINT ( 'NONE',  ( -4.006527145856388472, 117.9394519250054998, 1.074047527556786008 ) ) ;
#7433 = CARTESIAN_POINT ( 'NONE',  ( -49.93490050754573417, 16.96705409125581099, 5.170188367178237598 ) ) ;
#7434 = CARTESIAN_POINT ( 'NONE',  ( -57.44836869838920279, 2.247189469432294473, 1.860557060983530686 ) ) ;
#7435 = CARTESIAN_POINT ( 'NONE',  ( -4.371358227350733650, 118.1836130580517477, 0.4407715912306871542 ) ) ;
#7436 = CARTESIAN_POINT ( 'NONE',  ( 2.633027443571791970, 107.2200259174091315, -4.631959221834722307 ) ) ;
#7437 = ORIENTED_EDGE ( 'NONE', *, *, #20613, .T. ) ;
#7438 = CARTESIAN_POINT ( 'NONE',  ( -46.20552558087364758, 24.41938074005533466, 2.020549794458497139 ) ) ;
#7439 = CARTESIAN_POINT ( 'NONE',  ( -3.887428295838784464, 119.0433692556534737, -0.9258068317460230734 ) ) ;
#7440 = AXIS2_PLACEMENT_3D ( 'NONE', #16373, #32573, #32365 ) ;
#7441 = CARTESIAN_POINT ( 'NONE',  ( -2.923657115617448454, 107.8178375082508609, -4.476818208047827596 ) ) ;
#7442 = CARTESIAN_POINT ( 'NONE',  ( 4.509504427301486373, 118.1210246048803754, 0.6598204393874429474 ) ) ;
#7443 = CARTESIAN_POINT ( 'NONE',  ( -9.704918697729887356, 124.0009531390599591, -0.8840593909831663266 ) ) ;
#7444 = CARTESIAN_POINT ( 'NONE',  ( -1.183497919878635729, 115.7029491485453292, -1.742415236764897957 ) ) ;
#7445 = CARTESIAN_POINT ( 'NONE',  ( 3.928887737881764153, 118.1651004245801460, -0.5645064089330636969 ) ) ;
#7446 = CARTESIAN_POINT ( 'NONE',  ( 7.500421786656795042, 123.6595150816924047, 0.1155007223820210815 ) ) ;
#7447 = ADVANCED_FACE ( 'NONE', ( #29130 ), #22031, .T. ) ;
#7448 = CARTESIAN_POINT ( 'NONE',  ( -16.42797441217054910, 147.8801373804967341, -1.766026403434533876 ) ) ;
#7449 = CARTESIAN_POINT ( 'NONE',  ( -5.336420303164543633, 104.6144662015457101, 0.06783417913549341649 ) ) ;
#7450 = CARTESIAN_POINT ( 'NONE',  ( -47.72307967018315367, 19.52623448395708294, 5.191226814324476635 ) ) ;
#7451 = EDGE_CURVE ( 'NONE', #28646, #27727, #17968, .T. ) ;
#7452 = CARTESIAN_POINT ( 'NONE',  ( -5.586884702347495235, 75.27746620154573520, -0.1116392523995361763 ) ) ;
#7453 = CARTESIAN_POINT ( 'NONE',  ( -14.67956819919654343, 148.8681330163217922, -0.09511266571365764588 ) ) ;
#7454 = CARTESIAN_POINT ( 'NONE',  ( -10.00099186598785472, 77.19260062651656540, -1.269999999999998019 ) ) ;
#7455 = CARTESIAN_POINT ( 'NONE',  ( 8.135778112230736880, 117.7673425867732249, 0.7050676646501273792 ) ) ;
#7456 = CARTESIAN_POINT ( 'NONE',  ( 5.177913976931193041, 88.73331249999999670, -5.372100000000000541 ) ) ;
#7457 = CARTESIAN_POINT ( 'NONE',  ( 2.112177293979604187, -15.34403890755049815, 5.167321579062071457 ) ) ;
#7458 = CARTESIAN_POINT ( 'NONE',  ( -1.346530140709126133, 119.3298839580929638, 0.5995503221117501891 ) ) ;
#7459 = CARTESIAN_POINT ( 'NONE',  ( 0.1022289226565744474, -8.938468249466058779, 0.9708619238636220228 ) ) ;
#7460 = CARTESIAN_POINT ( 'NONE',  ( -22.76704383476090143, 150.0845277111093310, -1.179919005961814094 ) ) ;
#7461 = CARTESIAN_POINT ( 'NONE',  ( -0.8274880129334906131, 26.04165684986237039, -0.5117960016238547460 ) ) ;
#7462 = EDGE_LOOP ( 'NONE', ( #33089, #27813, #3991, #5407, #16878 ) ) ;
#7463 = CARTESIAN_POINT ( 'NONE',  ( -52.48304539424793091, 11.63526101311008354, 3.802211793135424678 ) ) ;
#7464 = CARTESIAN_POINT ( 'NONE',  ( 0.1497278248015747881, 105.8844662015457629, 5.338012126719978490 ) ) ;
#7465 = CARTESIAN_POINT ( 'NONE',  ( -7.125763582822579600, 121.8059686962219672, 0.4001172506815712793 ) ) ;
#7466 = CARTESIAN_POINT ( 'NONE',  ( 4.648743876849892764, -12.57259931633604388, 2.147031799546866182 ) ) ;
#7467 = CARTESIAN_POINT ( 'NONE',  ( 10.78650420462566828, 154.3566586077636487, -1.536168652981084293 ) ) ;
#7468 = ORIENTED_EDGE ( 'NONE', *, *, #31016, .F. ) ;
#7469 = CARTESIAN_POINT ( 'NONE',  ( -12.21694169560774768, 122.3148578561100948, -1.796258641216138541 ) ) ;
#7470 = CARTESIAN_POINT ( 'NONE',  ( 2.769004702249832750, 104.6144662015457811, 3.963074674433550992 ) ) ;
#7471 = EDGE_CURVE ( 'NONE', #38361, #41795, #31923, .T. ) ;
#7472 = CARTESIAN_POINT ( 'NONE',  ( 2.672745566561993247, -14.90124427853171873, 4.600530618394071070 ) ) ;
#7473 = FACE_OUTER_BOUND ( 'NONE', #25080, .T. ) ;
#7474 = CARTESIAN_POINT ( 'NONE',  ( 4.275377040554418251, 155.8374496918941077, -0.1508172661092591071 ) ) ;
#7475 = TOROIDAL_SURFACE ( 'NONE', #1356, 0.3810000000000001719, 0.2540000000000000036 ) ;
#7476 = ORIENTED_EDGE ( 'NONE', *, *, #20344, .F. ) ;
#7477 = CARTESIAN_POINT ( 'NONE',  ( -3.264132200829606312, 108.5668320698289477, 4.052510953551484718 ) ) ;
#7478 = CARTESIAN_POINT ( 'NONE',  ( 4.605371197558832286, 113.9923204192811994, 2.135305188882721694 ) ) ;
#7479 = VECTOR ( 'NONE', #18471, 1000.000000000000000 ) ;
#7480 = CARTESIAN_POINT ( 'NONE',  ( 4.756911902486301358, 117.3993836135862949, 1.207145067066230038 ) ) ;
#7481 = DIRECTION ( 'NONE',  ( 0.8745520943968235761, -0.4849315768086558398, 0.000000000000000000 ) ) ;
#7482 = CARTESIAN_POINT ( 'NONE',  ( 16.00576599164899605, 121.2237126890796191, 0.08595866332889597061 ) ) ;
#7483 = CARTESIAN_POINT ( 'NONE',  ( -20.21600168833980149, 80.16988503754176065, -1.270000000000003793 ) ) ;
#7484 = CARTESIAN_POINT ( 'NONE',  ( 2.001812122746663647, -15.27695281082187861, 5.988856565476218918 ) ) ;
#7485 = CARTESIAN_POINT ( 'NONE',  ( 11.37822013471386207, 56.06794068206382775, 5.016500000000000625 ) ) ;
#7486 = DIRECTION ( 'NONE',  ( -4.017660918040594346E-17, 1.000000000000000000, 2.376309959284834438E-19 ) ) ;
#7487 = CARTESIAN_POINT ( 'NONE',  ( 14.56794066961886358, 154.5799843816573684, 2.217559120334770650 ) ) ;
#7488 = ORIENTED_EDGE ( 'NONE', *, *, #11387, .F. ) ;
#7489 = CARTESIAN_POINT ( 'NONE',  ( 7.433834689873759061, 17.99627214424885580, -4.034796628604029323 ) ) ;
#7490 = CARTESIAN_POINT ( 'NONE',  ( -2.328736857929224691, 117.2194318322477642, -0.6714296531164799520 ) ) ;
#7491 = CARTESIAN_POINT ( 'NONE',  ( -2.840201032364617184, 114.3344743418335128, -2.128718819835312637 ) ) ;
#7492 = CARTESIAN_POINT ( 'NONE',  ( -14.01601067707388992, 79.52082022139843787, 1.269999999999998463 ) ) ;
#7493 = CARTESIAN_POINT ( 'NONE',  ( -4.576084639598200887, 113.7931665046256029, -2.209524532645662731 ) ) ;
#7494 = DIRECTION ( 'NONE',  ( -0.6294287539883864913, -0.7770581983690970640, 0.000000000000000000 ) ) ;
#7495 = CARTESIAN_POINT ( 'NONE',  ( 4.087030650986479330, 6.990161447142720696, 2.163025551504125232 ) ) ;
#7496 = DIRECTION ( 'NONE',  ( 0.000000000000000000, 0.000000000000000000, -1.000000000000000000 ) ) ;
#7497 = CARTESIAN_POINT ( 'NONE',  ( -4.651991910126532126, 111.7581736691619341, -2.677509894684430680 ) ) ;
#7498 = CARTESIAN_POINT ( 'NONE',  ( 3.258219809910011033, -14.04213616937880005, 2.843395319141139410 ) ) ;
#7499 = CARTESIAN_POINT ( 'NONE',  ( 2.174325380064840996, 109.8863472468248119, -3.630110603364346211 ) ) ;
#7500 = CARTESIAN_POINT ( 'NONE',  ( -2.899870334229920132, 116.9538966677400254, 0.3598414239652115709 ) ) ;
#7501 = AXIS2_PLACEMENT_3D ( 'NONE', #34300, #18286, #37900 ) ;
#7502 = CARTESIAN_POINT ( 'NONE',  ( -1.381525208824001538, 34.89533589863157204, 3.514877943587163767 ) ) ;
#7503 = CARTESIAN_POINT ( 'NONE',  ( -9.712308604790303335, 65.53852105402241079, 1.270000000000003126 ) ) ;
#7504 = ORIENTED_EDGE ( 'NONE', *, *, #11013, .F. ) ;
#7505 = CARTESIAN_POINT ( 'NONE',  ( -2.498980821681361153, 104.6144662015457243, -4.129459300827505785 ) ) ;
#7506 = CARTESIAN_POINT ( 'NONE',  ( 5.113606203424133412, -15.47995924129362599, 1.801594979316981204 ) ) ;
#7507 = CARTESIAN_POINT ( 'NONE',  ( -16.76200238010698129, 128.5636217276695561, 1.481418206722939335 ) ) ;
#7508 = CARTESIAN_POINT ( 'NONE',  ( 0.8793282038724897776, 27.06027571872007442, 0.4248793764785103177 ) ) ;
#7509 = EDGE_LOOP ( 'NONE', ( #14661, #32317 ) ) ;
#7510 = CYLINDRICAL_SURFACE ( 'NONE', #32775, 0.2539999999999998925 ) ;
#7511 = CARTESIAN_POINT ( 'NONE',  ( 0.8524833535542716278, 121.9014879524050343, 0.3240522193994319067 ) ) ;
#7512 =( LENGTH_UNIT ( ) NAMED_UNIT ( * ) SI_UNIT ( .MILLI., .METRE. ) );
#7513 = CARTESIAN_POINT ( 'NONE',  ( -16.95093959817323181, 147.3835828867039766, 1.246432153888628935 ) ) ;
#7514 = DIRECTION ( 'NONE',  ( -5.188838149069471174E-16, 1.699382548006136313E-16, 1.000000000000000000 ) ) ;
#7515 = CARTESIAN_POINT ( 'NONE',  ( 17.82416131750959210, 140.4837523222294351, -1.726486987461785860 ) ) ;
#7516 = CARTESIAN_POINT ( 'NONE',  ( -20.53125589898989389, 145.6130255286810495, -2.451886524809591350 ) ) ;
#7517 = CARTESIAN_POINT ( 'NONE',  ( -19.21741104974024594, 79.92823415920659613, 1.269999999999994911 ) ) ;
#7518 = CARTESIAN_POINT ( 'NONE',  ( 4.308178849057600956, 118.2138035341862405, -0.3345321977047149842 ) ) ;
#7519 = CARTESIAN_POINT ( 'NONE',  ( 10.70072142757958922, 153.0728289088170300, -0.5595718250706015473 ) ) ;
#7520 = ORIENTED_EDGE ( 'NONE', *, *, #24095, .F. ) ;
#7521 = CARTESIAN_POINT ( 'NONE',  ( 3.238076882636043763, -14.77659300283332122, 2.967476587227507956 ) ) ;
#7522 = VECTOR ( 'NONE', #20859, 1000.000000000000000 ) ;
#7523 = CARTESIAN_POINT ( 'NONE',  ( -4.854232772743657165, 117.4081466956269395, 0.9971777887500445914 ) ) ;
#7524 = CARTESIAN_POINT ( 'NONE',  ( -54.51629495445180140, 7.799846118209302404, 3.232377281230888855 ) ) ;
#7525 = CARTESIAN_POINT ( 'NONE',  ( -1.246715508051662535, 10.49814879194060069, 4.449005273994115939 ) ) ;
#7526 = CARTESIAN_POINT ( 'NONE',  ( 7.227551859934576939, 121.2980461901665308, 1.025750885112893807 ) ) ;
#7527 = CARTESIAN_POINT ( 'NONE',  ( -2.647869110835376016, 30.13907626823893082, -0.2047939377594477361 ) ) ;
#7528 = CONICAL_SURFACE ( 'NONE', #27261, 12.69999999999999751, 0.7853981633974485010 ) ;
#7529 = CARTESIAN_POINT ( 'NONE',  ( 4.636458409304901274, 17.36039413176390411, -0.09481320587925551324 ) ) ;
#7530 = CARTESIAN_POINT ( 'NONE',  ( 15.26129097679449131, 148.0152273645666980, 0.3559380457717283841 ) ) ;
#7531 = DIRECTION ( 'NONE',  ( -0.3582377630123915746, 0.9336303900108851028, -3.445432962228667069E-16 ) ) ;
#7532 = CARTESIAN_POINT ( 'NONE',  ( -55.81215269371604393, 4.390389611868092068, -0.4227292597524531792 ) ) ;
#7533 = CARTESIAN_POINT ( 'NONE',  ( 2.173876196063857513, 116.2747682467607575, -0.1408475702141917807 ) ) ;
#7534 = CARTESIAN_POINT ( 'NONE',  ( -15.42835734045148577, 79.74558783746837776, 1.269999999999998019 ) ) ;
#7535 = ORIENTED_EDGE ( 'NONE', *, *, #8734, .T. ) ;
#7536 = CARTESIAN_POINT ( 'NONE',  ( -12.69999999999999574, 14.60500000000000398, 1.555301434917138235E-15 ) ) ;
#7537 = DIRECTION ( 'NONE',  ( -0.7071067811865475727, -0.7071067811865474617, 8.659560562354931626E-17 ) ) ;
#7538 = CARTESIAN_POINT ( 'NONE',  ( -29.81988630912367455, 58.80898419537163591, -1.523999999998479460 ) ) ;
#7539 = AXIS2_PLACEMENT_3D ( 'NONE', #29452, #31813, #19225 ) ;
#7540 = CARTESIAN_POINT ( 'NONE',  ( 7.890306666665830804, -2.504341373917490898, 2.985612812370990632 ) ) ;
#7541 = CARTESIAN_POINT ( 'NONE',  ( -5.256643466096560857, 56.51499999999957424, 5.296410793414254137 ) ) ;
#7542 = CARTESIAN_POINT ( 'NONE',  ( -14.64596739026573857, 69.73430801926814127, -1.523999999999999355 ) ) ;
#7543 = CARTESIAN_POINT ( 'NONE',  ( -58.39046968809522298, 1.092456688167306567, 0.3056578461530140567 ) ) ;
#7544 = CARTESIAN_POINT ( 'NONE',  ( 0.001862839608491519139, 124.0591982226671490, -0.09322411149287214427 ) ) ;
#7545 = CARTESIAN_POINT ( 'NONE',  ( -23.16157447928876323, 142.6111785389246336, 0.1383437888640693669 ) ) ;
#7546 = ORIENTED_EDGE ( 'NONE', *, *, #10977, .T. ) ;
#7547 = CARTESIAN_POINT ( 'NONE',  ( -57.97744691355249813, 2.174673694799844625, -0.6577596567056189780 ) ) ;
#7548 = CARTESIAN_POINT ( 'NONE',  ( -4.968812502051799918, 56.51947257897022325, 4.801689445547930646 ) ) ;
#7549 = ORIENTED_EDGE ( 'NONE', *, *, #28197, .T. ) ;
#7550 = FACE_OUTER_BOUND ( 'NONE', #18933, .T. ) ;
#7552 = CARTESIAN_POINT ( 'NONE',  ( -4.590565121197838216, 121.2030596905490540, -0.1190299148670778545 ) ) ;
#7551 = VECTOR ( 'NONE', #32398, 1000.000000000000114 ) ;
#7553 = CARTESIAN_POINT ( 'NONE',  ( 3.435007001638270996, -15.26001923902611779, 5.499761658607620340 ) ) ;
#7554 = CARTESIAN_POINT ( 'NONE',  ( -20.68240061501462534, 141.5323519391372997, 1.529040698034871859 ) ) ;
#7555 = CARTESIAN_POINT ( 'NONE',  ( 0.2838385327444274964, 29.22985346960623332, -4.617364983570896086 ) ) ;
#7556 = CARTESIAN_POINT ( 'NONE',  ( 18.54318072098650561, 125.2038358216989735, 0.7288164436403702373 ) ) ;
#7557 = CARTESIAN_POINT ( 'NONE',  ( 4.192904522445743964, 155.8780965706680774, 0.2271539898920573453 ) ) ;
#7558 = DIRECTION ( 'NONE',  ( -0.8745520943968250194, 0.4849315768086532863, -5.361993529360574930E-16 ) ) ;
#7559 = CARTESIAN_POINT ( 'NONE',  ( -0.8651787172165069650, -5.103258934911358402, 0.4504873164067982327 ) ) ;
#7560 = CARTESIAN_POINT ( 'NONE',  ( -5.727173706516765606, 159.1225378944267845, -0.2665985390141680789 ) ) ;
#7561 = CARTESIAN_POINT ( 'NONE',  ( -29.91360363449003756, 70.04874496952835727, -1.524000000000007349 ) ) ;
#7562 = CARTESIAN_POINT ( 'NONE',  ( 4.756911902506432810, 117.3993836136063607, 1.207145067191207621 ) ) ;
#7563 = CARTESIAN_POINT ( 'NONE',  ( -8.753730273135673201, 117.9543236253998799, 0.3768632908176075547 ) ) ;
#7564 = CARTESIAN_POINT ( 'NONE',  ( -10.93624696698920751, 154.4230204216147513, 1.584134132468239420 ) ) ;
#7565 = CARTESIAN_POINT ( 'NONE',  ( -57.44712170204855539, 1.698054324899128220, -1.444792672776622267 ) ) ;
#7566 = CARTESIAN_POINT ( 'NONE',  ( 0.4013927055962251411, 117.8786474493541050, 0.5472391114537521473 ) ) ;
#7567 = CARTESIAN_POINT ( 'NONE',  ( 12.41883037655676247, 155.1253022143813496, -1.737092194502518394 ) ) ;
#7568 = CARTESIAN_POINT ( 'NONE',  ( -0.001188813386588473625, -13.89074316258246000, -0.9734844304884215926 ) ) ;
#7569 = CARTESIAN_POINT ( 'NONE',  ( -17.95761459997887144, 128.5942011134444272, -1.926528613670785095 ) ) ;
#7570 = CARTESIAN_POINT ( 'NONE',  ( -45.68084146533627177, 21.25878370237693815, -4.188014402015116211 ) ) ;
#7571 = CARTESIAN_POINT ( 'NONE',  ( 4.808131379913066716, 104.6144662015456959, -0.4149153342096277841 ) ) ;
#7572 = CARTESIAN_POINT ( 'NONE',  ( 16.36402192804832012, 147.4903123243063590, -0.9458667783343724933 ) ) ;
#7573 = CARTESIAN_POINT ( 'NONE',  ( 7.844435714580729524, 122.2806349566659065, 0.7396647843393954203 ) ) ;
#7574 = ORIENTED_EDGE ( 'NONE', *, *, #36259, .F. ) ;
#7575 = CARTESIAN_POINT ( 'NONE',  ( -3.364155546990544199, 119.5845705363850442, -0.8331338896180614517 ) ) ;
#7576 = CARTESIAN_POINT ( 'NONE',  ( 4.918985584458519966, -15.36470173770705649, 0.08744857223284302483 ) ) ;
#7577 = DIRECTION ( 'NONE',  ( -0.01997839162482737546, -1.040247600000940825E-18, 0.9998004120163610509 ) ) ;
#7578 = CARTESIAN_POINT ( 'NONE',  ( -4.395042894517541043, 118.1799360432506347, -0.5693510968962494090 ) ) ;
#7579 = CARTESIAN_POINT ( 'NONE',  ( -54.39768377094780760, 8.094885465611476150, -3.421923752996840928 ) ) ;
#7580 = DIRECTION ( 'NONE',  ( 0.1728608224830406603, 1.098208118798718614E-16, 0.9849462604886047856 ) ) ;
#7581 = PRODUCT_DEFINITION_SHAPE ( 'NONE', 'NONE',  #10216 ) ;
#7582 = CARTESIAN_POINT ( 'NONE',  ( 11.26837603645361341, 123.0403929720162495, 1.648478483780370540 ) ) ;
#7583 = CARTESIAN_POINT ( 'NONE',  ( 3.019425909971710009, 50.13146620154573441, -1.718019622760792009 ) ) ;
#7584 = CARTESIAN_POINT ( 'NONE',  ( 1.421603664355671315, 159.6054662015457666, 0.02840702444251847966 ) ) ;
#7585 = CARTESIAN_POINT ( 'NONE',  ( 8.101632580580826470, 8.064395906452419993, -2.298819013970823999 ) ) ;
#7586 = CARTESIAN_POINT ( 'NONE',  ( 15.91353055065138022, 146.3070982487133165, 0.9133378546330941372 ) ) ;
#7587 = CARTESIAN_POINT ( 'NONE',  ( 4.866704567515524715, 117.3073154462328063, -0.4935321157908418299 ) ) ;
#7588 = LINE ( 'NONE', #39552, #26048 ) ;
#7589 = CARTESIAN_POINT ( 'NONE',  ( 13.46199999999999619, 13.84300000000000175, 0.000000000000000000 ) ) ;
#7590 = CARTESIAN_POINT ( 'NONE',  ( -58.37241122568487128, -0.2962816677227614326, -1.047861413196692856E-14 ) ) ;
#7591 = CARTESIAN_POINT ( 'NONE',  ( -0.001319893060213154059, 116.4580521601689185, 0.06605284600166372311 ) ) ;
#7592 = ORIENTED_EDGE ( 'NONE', *, *, #18795, .F. ) ;
#7593 = CARTESIAN_POINT ( 'NONE',  ( -48.05879467440716013, 25.10120116127142964, -0.1605504162684674441 ) ) ;
#7594 = CARTESIAN_POINT ( 'NONE',  ( 5.425175176548000522, 120.5927626492978249, -0.5604424002130801163 ) ) ;
#7595 = CARTESIAN_POINT ( 'NONE',  ( -46.87302333144432254, 25.14943835890254675, -1.855287453902875416 ) ) ;
#7596 = ORIENTED_EDGE ( 'NONE', *, *, #24853, .F. ) ;
#7597 = DIRECTION ( 'NONE',  ( 0.9998004120163608288, 5.205824365704081956E-17, 0.01997839162482748995 ) ) ;
#7598 = CARTESIAN_POINT ( 'NONE',  ( -3.687801383043832981, 120.9852966486377710, -0.2688355818071223591 ) ) ;
#7599 = CARTESIAN_POINT ( 'NONE',  ( 3.797208283716756227, -14.50848223276941873, 5.080264250175951624 ) ) ;
#7600 = AXIS2_PLACEMENT_3D ( 'NONE', #25079, #38085, #27645 ) ;
#7601 = CARTESIAN_POINT ( 'NONE',  ( -21.93433297169883289, 150.0588410196355937, 0.9994452811612329901 ) ) ;
#7602 = CARTESIAN_POINT ( 'NONE',  ( 5.078986093043054595, 69.43546620154572224, 0.1014902294541237815 ) ) ;
#7603 = VECTOR ( 'NONE', #28270, 1000.000000000000114 ) ;
#7604 = CARTESIAN_POINT ( 'NONE',  ( 15.93236088550697716, 121.0320206851898206, 0.3693416020086465190 ) ) ;
#7605 = ORIENTED_EDGE ( 'NONE', *, *, #39968, .F. ) ;
#7606 = CARTESIAN_POINT ( 'NONE',  ( 4.560281875334545099, -11.68902278883368595, 0.6958564903332965512 ) ) ;
#7607 = B_SPLINE_CURVE_WITH_KNOTS ( 'NONE', 3,
 ( #16647, #39034, #10260, #36268, #703, #26665, #6661, #33281, #7087, #20050, #13674, #13035, #4110, #26026, #22602, #30073, #38823 ),
 .UNSPECIFIED., .F., .F.,
 ( 4, 1, 1, 1, 1, 1, 1, 1, 1, 1, 1, 1, 1, 1, 4 ),
 ( 0.000000000000000000, 0.08300113939718137268, 0.1732806554784933895, 0.2717672377176819087, 0.3752096606209606167, 0.4787223716043260135, 0.5772295444745598747, 0.6668133826162351285, 0.7470991451079272982, 0.7815930070524458317, 0.8169452614683294644, 0.8547689062991584708, 0.8968063284581728745, 0.9447228702782888288, 1.000000000000000000 ),
 .UNSPECIFIED. ) ;
#7608 = CARTESIAN_POINT ( 'NONE',  ( -15.19604463793445959, 156.0859089222169587, -0.3036531364422413448 ) ) ;
#7609 = CARTESIAN_POINT ( 'NONE',  ( 9.638062024671789629, 56.51500000000000057, 4.786355703798467734E-15 ) ) ;
#7610 = DIRECTION ( 'NONE',  ( -5.188838149069471174E-16, 1.699382548006136313E-16, 1.000000000000000000 ) ) ;
#7611 = ORIENTED_EDGE ( 'NONE', *, *, #21370, .F. ) ;
#7612 = CARTESIAN_POINT ( 'NONE',  ( -8.213274639754041928, 120.6581850290335609, 1.077640066613805070 ) ) ;
#7613 = CARTESIAN_POINT ( 'NONE',  ( 4.264856162967361364, -5.269518785209044154, -1.792273654951743067 ) ) ;
#7614 = CARTESIAN_POINT ( 'NONE',  ( 6.860783072103382452, 117.8105958006179890, 0.8866969874101000570 ) ) ;
#7615 = CARTESIAN_POINT ( 'NONE',  ( -57.70126415073581683, 1.705439686540813238, -1.647193596428901285 ) ) ;
#7617 = CARTESIAN_POINT ( 'NONE',  ( 20.82688902969335487, 148.9555414352193168, -1.562960617212841186 ) ) ;
#7616 = CARTESIAN_POINT ( 'NONE',  ( -46.60530155212502024, 26.17382724835479735, -8.515758108943001820E-15 ) ) ;
#7618 = CIRCLE ( 'NONE', #36872, 6.905625000000000568 ) ;
#7619 = CARTESIAN_POINT ( 'NONE',  ( -2.900346660479264482, -2.445871450894649968, -3.618988008572288972 ) ) ;
#7620 = CARTESIAN_POINT ( 'NONE',  ( -7.681555067352650035, 158.5863655655865330, -1.054772010160866857 ) ) ;
#7621 = EDGE_CURVE ( 'NONE', #36646, #38078, #9140, .T. ) ;
#7622 = ORIENTED_EDGE ( 'NONE', *, *, #26920, .T. ) ;
#7623 = CARTESIAN_POINT ( 'NONE',  ( -1.597555633484793125, 120.9451058151398399, 0.06333991727891977175 ) ) ;
#7624 = CARTESIAN_POINT ( 'NONE',  ( 3.842082824490853810, -15.33115451161810938, 5.194229279690915746 ) ) ;
#7625 = CARTESIAN_POINT ( 'NONE',  ( -45.05484530740381643, 21.03919035317155206, 3.644944174415911675 ) ) ;
#7626 = DIRECTION ( 'NONE',  ( 1.011795553208986377E-16, 1.000000000000000000, -0.000000000000000000 ) ) ;
#7627 = EDGE_CURVE ( 'NONE', #8692, #25310, #20004, .T. ) ;
#7628 = ORIENTED_EDGE ( 'NONE', *, *, #8361, .F. ) ;
#7629 = CARTESIAN_POINT ( 'NONE',  ( 11.88796246241977883, 122.6721150436042223, 1.770419579776735697 ) ) ;
#7630 = CARTESIAN_POINT ( 'NONE',  ( -6.606344270946872901E-14, 95.34346620154573770, 1.014423412895214384E-29 ) ) ;
#7631 = DIRECTION ( 'NONE',  ( -0.1469470846586743706, 1.414713986243376972E-17, 0.9891443546370348727 ) ) ;
#7632 = AXIS2_PLACEMENT_3D ( 'NONE', #31582, #15166, #28595 ) ;
#7633 = CARTESIAN_POINT ( 'NONE',  ( -8.071933480009693795, 118.1206512225135015, 0.6391883341457642587 ) ) ;
#7634 = CARTESIAN_POINT ( 'NONE',  ( -5.321447747238043036, 7.245273219182337243, -6.556399146060885919 ) ) ;
#7635 = CARTESIAN_POINT ( 'NONE',  ( 16.47979853205664824, 146.5532241433796230, 1.607449420861547962 ) ) ;
#7636 = CARTESIAN_POINT ( 'NONE',  ( -24.49496359545907609, 76.94162913054094588, -1.524000000000005572 ) ) ;
#7637 = CARTESIAN_POINT ( 'NONE',  ( 21.01068656986052829, 132.3427885975763161, -0.3612206858233396600 ) ) ;
#7638 = CARTESIAN_POINT ( 'NONE',  ( 4.698556703264293866, 117.9254231662981738, -0.7749991471470429882 ) ) ;
#7639 = CARTESIAN_POINT ( 'NONE',  ( -53.27040232883901183, 10.25240396212598348, 3.758512621827925226 ) ) ;
#7640 = CARTESIAN_POINT ( 'NONE',  ( -47.59483747600737047, 24.73124547893296921, 0.7500189231788738642 ) ) ;
#7641 = CARTESIAN_POINT ( 'NONE',  ( -49.66210360255988832, 16.76989353321783227, 4.946330335750482199 ) ) ;
#7642 = CARTESIAN_POINT ( 'NONE',  ( -57.92211639876096996, 1.229603953560909124, 1.440092494702427617 ) ) ;
#7643 = EDGE_CURVE ( 'NONE', #19349, #11005, #30893, .T. ) ;
#7644 = CARTESIAN_POINT ( 'NONE',  ( -4.482462170607306895, 118.1125532305710664, 0.5757334087516573495 ) ) ;
#7645 = CARTESIAN_POINT ( 'NONE',  ( 1.899379616367111279, 106.4949638843779809, -4.984221880255138792 ) ) ;
#7646 = ORIENTED_EDGE ( 'NONE', *, *, #33633, .T. ) ;
#7647 = CARTESIAN_POINT ( 'NONE',  ( -46.68395179480138779, 26.03198510454123848, 1.523999999999991140 ) ) ;
#7648 = TOROIDAL_SURFACE ( 'NONE', #25996, 0.3809999999999997278, 0.2540000000000000036 ) ;
#7649 = EDGE_CURVE ( 'NONE', #37617, #27765, #28104, .T. ) ;
#7650 = CARTESIAN_POINT ( 'NONE',  ( 3.950356500571747809, 119.0647496460593686, -0.7685950494401324606 ) ) ;
#7651 = CARTESIAN_POINT ( 'NONE',  ( -5.384759902136890375, 117.1811293437636721, -0.8990931802006211226 ) ) ;
#7652 = CARTESIAN_POINT ( 'NONE',  ( 4.500448308262108732, 118.1244505159430247, 0.6707133188938370072 ) ) ;
#7653 = CARTESIAN_POINT ( 'NONE',  ( -1.710293758672658759, 156.3676537730497387, -0.7734167093480263100 ) ) ;
#7654 = FILL_AREA_STYLE_COLOUR ( '', #1589 ) ;
#7655 = EDGE_CURVE ( 'NONE', #4128, #40015, #16773, .T. ) ;
#7656 = CARTESIAN_POINT ( 'NONE',  ( 1.144237119838787287, 117.3993836041131402, -1.432026387098619402 ) ) ;
#7657 = CARTESIAN_POINT ( 'NONE',  ( -4.559029627765868398, 31.49133049583988253, -0.6947656260628575220 ) ) ;
#7658 = CARTESIAN_POINT ( 'NONE',  ( -6.627928625996650780, 155.5185402614932570, -1.342408143365147577 ) ) ;
#7659 = CARTESIAN_POINT ( 'NONE',  ( -4.559649833866270541, 116.0444662015457169, -3.750543233647261498 ) ) ;
#7660 = CARTESIAN_POINT ( 'NONE',  ( -46.39387867998472359, 20.78226312411871035, 4.747706454273270538 ) ) ;
#7661 = CARTESIAN_POINT ( 'NONE',  ( 8.072253591115288174, 121.3304565451444574, -0.9161511751189075348 ) ) ;
#7662 = CARTESIAN_POINT ( 'NONE',  ( -1.638793754983947304, 120.9957929572446886, 0.06788950568023216503 ) ) ;
#7663 = CARTESIAN_POINT ( 'NONE',  ( 7.461249999999948201, 83.56599999999998829, 6.819232607250622208E-46 ) ) ;
#7664 = CARTESIAN_POINT ( 'NONE',  ( 0.9824256172934900944, 116.9078805053781025, 0.3575799159885131306 ) ) ;
#7665 = CARTESIAN_POINT ( 'NONE',  ( 5.871452009091292723, 77.01756249999996840, -5.016499999999999737 ) ) ;
#7666 = CARTESIAN_POINT ( 'NONE',  ( 3.351397644842732948, -15.05179984492975542, 2.935234935891222641 ) ) ;
#7667 = CARTESIAN_POINT ( 'NONE',  ( -3.344131534676259232, 119.2933411826354728, 0.7437009012386071038 ) ) ;
#7668 = CARTESIAN_POINT ( 'NONE',  ( 0.7703063551133444431, -5.692625084440793515, -0.5956917769006077057 ) ) ;
#7669 = CARTESIAN_POINT ( 'NONE',  ( -19.79238143276398176, 128.7876384977266468, -1.131474956103616814 ) ) ;
#7670 = AXIS2_PLACEMENT_3D ( 'NONE', #959, #26077, #39936 ) ;
#7671 = CARTESIAN_POINT ( 'NONE',  ( -0.8573366540693068139, -6.603747334586292261, -0.4721712316449505620 ) ) ;
#7672 = VERTEX_POINT ( 'NONE', #818 ) ;
#7673 = CARTESIAN_POINT ( 'NONE',  ( -50.43530108972998960, 14.71354995532366594, 3.653486772774918734 ) ) ;
#7674 = CARTESIAN_POINT ( 'NONE',  ( 5.590287297675133438, 117.9270669303711117, 0.7481252288361714964 ) ) ;
#7675 = CARTESIAN_POINT ( 'NONE',  ( -10.87798892776825177, 126.1616406593870607, 0.4640774846651396501 ) ) ;
#7676 = CARTESIAN_POINT ( 'NONE',  ( 4.673344545167823938, -12.29283961637177214, 1.688191869143181201 ) ) ;
#7677 = CARTESIAN_POINT ( 'NONE',  ( 10.38102865001212471, 154.1877054190025262, -1.364427777124047170 ) ) ;
#7678 = ORIENTED_EDGE ( 'NONE', *, *, #14926, .T. ) ;
#7679 = CARTESIAN_POINT ( 'NONE',  ( -11.81048985551422703, 122.0047285378078357, -1.760929439237068017 ) ) ;
#7680 = CARTESIAN_POINT ( 'NONE',  ( 3.601325883493490920, 115.7029493296494707, 1.622373432873002175 ) ) ;
#7681 = CARTESIAN_POINT ( 'NONE',  ( 2.569204629087775693, -14.95572128602136530, 4.738577790166504933 ) ) ;
#7682 = CARTESIAN_POINT ( 'NONE',  ( -4.912057176082959664, 117.6260355129238491, -0.9592288914727921112 ) ) ;
#7683 = CARTESIAN_POINT ( 'NONE',  ( 9.164740666423933035, 153.8946005065304803, -0.1038620377607962914 ) ) ;
#7684 = AXIS2_PLACEMENT_3D ( 'NONE', #1406, #40384, #24371 ) ;
#7685 = ORIENTED_EDGE ( 'NONE', *, *, #33617, .F. ) ;
#7686 = CYLINDRICAL_SURFACE ( 'NONE', #11825, 2.540000000000000480 ) ;
#7687 = DIRECTION ( 'NONE',  ( 0.01997839162482749689, 1.040247600000945640E-18, -0.9998004120163610509 ) ) ;
#7688 = FACE_BOUND ( 'NONE', #23877, .T. ) ;
#7689 = DIRECTION ( 'NONE',  ( 5.188838149069472160E-16, -1.699382548006136559E-16, -1.000000000000000000 ) ) ;
#7690 = EDGE_CURVE ( 'NONE', #16059, #702, #5027, .T. ) ;
#7691 = CARTESIAN_POINT ( 'NONE',  ( 10.80084657379828528, 157.9251727141802633, 0.03745751586626431401 ) ) ;
#7692 = ADVANCED_FACE ( 'NONE', ( #30190 ), #15882, .T. ) ;
#7693 = DIRECTION ( 'NONE',  ( 5.188838149069472160E-16, -1.699382548006136559E-16, -1.000000000000000000 ) ) ;
#7694 = TOROIDAL_SURFACE ( 'NONE', #25385, 0.7620000000000000107, 0.2540000000000000036 ) ;
#7695 = CARTESIAN_POINT ( 'NONE',  ( 1.799054236152410224, -15.56691960250831919, 5.455207115090923153 ) ) ;
#7696 = CARTESIAN_POINT ( 'NONE',  ( -28.76494711669534610, 76.52965637509277030, -1.270000000000007567 ) ) ;
#7697 = CARTESIAN_POINT ( 'NONE',  ( -1.067875954944055072, 33.20386983296905470, 0.7215342646006036587 ) ) ;
#7698 = CARTESIAN_POINT ( 'NONE',  ( 13.21388725472894166, 155.5383117973235585, 2.112422614401995080 ) ) ;
#7699 = ORIENTED_EDGE ( 'NONE', *, *, #36327, .T. ) ;
#7700 = CARTESIAN_POINT ( 'NONE',  ( -3.973931221679809056, 20.38425861574787490, -7.466160517099206473 ) ) ;
#7701 = CARTESIAN_POINT ( 'NONE',  ( 2.373934424165132118, 117.2554555581296825, -0.5878954194807157752 ) ) ;
#7702 = CARTESIAN_POINT ( 'NONE',  ( -0.5479319383246573638, 107.0594419416054848, -4.854436055212456580 ) ) ;
#7703 = CARTESIAN_POINT ( 'NONE',  ( -5.477532837487763651, 78.92140300690499544, 5.132221182818779148 ) ) ;
#7704 = CARTESIAN_POINT ( 'NONE',  ( 15.50061618130081165, 62.14374591690594940, 1.904999999999990035 ) ) ;
#7705 = CARTESIAN_POINT ( 'NONE',  ( -0.01111760956215399228, 120.5507043431653784, 0.5563706444133253992 ) ) ;
#7706 = CARTESIAN_POINT ( 'NONE',  ( -1.214995109038484067, 0.9429784454696930052, -4.460028654918597901 ) ) ;
#7707 = EDGE_CURVE ( 'NONE', #26452, #37991, #2291, .T. ) ;
#7708 = DIRECTION ( 'NONE',  ( -0.8745520943968843053, 0.4849315768085461498, -4.268512490100407458E-16 ) ) ;
#7709 = CARTESIAN_POINT ( 'NONE',  ( -4.766160292286565792, 118.5264896598256854, 0.8411326837336940976 ) ) ;
#7710 = CARTESIAN_POINT ( 'NONE',  ( 3.215637690559757456, -14.25221971482225314, 3.321654998001884795 ) ) ;
#7711 = CARTESIAN_POINT ( 'NONE',  ( 2.721163413801359177, 112.7379566594982663, -2.570110030560514236 ) ) ;
#7712 = CARTESIAN_POINT ( 'NONE',  ( -16.58356254348282732, 122.7279807066903032, 0.3948093068319186716 ) ) ;
#7713 = CARTESIAN_POINT ( 'NONE',  ( -0.5795191656544192993, 34.20384076381332505, 3.605158861677521642 ) ) ;
#7714 = DIRECTION ( 'NONE',  ( -1.000000000000000000, -1.092739197465705287E-15, 0.000000000000000000 ) ) ;
#7715 = ORIENTED_EDGE ( 'NONE', *, *, #3453, .F. ) ;
#7716 = CARTESIAN_POINT ( 'NONE',  ( -5.182787013109720675, 104.6144662015412905, -1.273143517811092584 ) ) ;
#7717 = CARTESIAN_POINT ( 'NONE',  ( 5.315755633098069310, -15.26259334675766866, -0.1387823706055290596 ) ) ;
#7718 = CARTESIAN_POINT ( 'NONE',  ( -16.12894526037929666, 128.5601350900737998, 1.548733376446669086 ) ) ;
#7719 = CARTESIAN_POINT ( 'NONE',  ( -4.187759052228169132, -5.978784877027076838, 2.003160513425938483 ) ) ;
#7720 = VERTEX_POINT ( 'NONE', #13586 ) ;
#7721 = DIRECTION ( 'NONE',  ( 5.188838149069471174E-16, -1.699382548006136313E-16, -1.000000000000000000 ) ) ;
#7722 = CARTESIAN_POINT ( 'NONE',  ( 0.8420595575567756397, 109.5507526474568607, 3.867914470699520102 ) ) ;
#7723 = CARTESIAN_POINT ( 'NONE',  ( -16.48541106618858976, 147.8801373804967341, 1.108338632072817465 ) ) ;
#7724 = CARTESIAN_POINT ( 'NONE',  ( -47.23734577298776571, 20.07943201422508395, 5.152903770775020931 ) ) ;
#7725 = CARTESIAN_POINT ( 'NONE',  ( 7.478391884465288797, 120.4750020944285609, -1.007254920367567808 ) ) ;
#7726 = CARTESIAN_POINT ( 'NONE',  ( 0.01111639779257688268, 118.2594330468507593, -0.5563100024230159812 ) ) ;
#7727 = CARTESIAN_POINT ( 'NONE',  ( -5.078986093043186045, 82.13546620154573930, -0.1014902294541231570 ) ) ;
#7728 = CARTESIAN_POINT ( 'NONE',  ( 4.171308675837464008, 118.2392932148226095, -0.2183557931388009354 ) ) ;
#7729 = VECTOR ( 'NONE', #19966, 1000.000000000000114 ) ;
#7730 = CARTESIAN_POINT ( 'NONE',  ( 4.443995521150066352, 155.8637389808261275, -0.5396741685193006122 ) ) ;
#7731 = ORIENTED_EDGE ( 'NONE', *, *, #29812, .F. ) ;
#7732 = CARTESIAN_POINT ( 'NONE',  ( 3.240743527130751200, -15.12236442990058727, 3.435505395146291274 ) ) ;
#7733 = CARTESIAN_POINT ( 'NONE',  ( 11.82906070755469763, 56.41571150956137615, -5.016500000000000625 ) ) ;
#7734 = CIRCLE ( 'NONE', #5010, 13.46199999999999619 ) ;
#7735 = CARTESIAN_POINT ( 'NONE',  ( -57.69387532515970918, 1.166760082113277308, 1.211409762388486300 ) ) ;
#7736 = CARTESIAN_POINT ( 'NONE',  ( 0.4327634382839667393, 5.975216699623357108, -4.620561613140377055 ) ) ;
#7737 = CARTESIAN_POINT ( 'NONE',  ( 10.85577430263303356, 123.7747955097422476, 1.451053175688577390 ) ) ;
#7738 = CARTESIAN_POINT ( 'NONE',  ( 0.9281906404964570534, 34.59732502943162302, 2.863135987906453739 ) ) ;
#7739 = CARTESIAN_POINT ( 'NONE',  ( -6.932344361571818325, 124.3275308867733600, -0.1272746869527292546 ) ) ;
#7740 = CARTESIAN_POINT ( 'NONE',  ( 4.585487687326599726, 17.13547844546973309, 0.5842699607688729424 ) ) ;
#7741 = CARTESIAN_POINT ( 'NONE',  ( 15.78392762965199303, 146.2390805666957192, 0.3668625800963858929 ) ) ;
#7742 = DIRECTION ( 'NONE',  ( 5.188838149069472160E-16, -1.699382548006136559E-16, -1.000000000000000000 ) ) ;
#7743 = ADVANCED_FACE ( 'NONE', ( #13793 ), #13996, .F. ) ;
#7744 = CARTESIAN_POINT ( 'NONE',  ( -52.57757236033170045, 11.11936768914174145, -3.180765541460440105 ) ) ;
#7745 = CARTESIAN_POINT ( 'NONE',  ( 5.563757564550819268, 116.7201818126403197, -0.05438542879854482009 ) ) ;
#7746 = FACE_OUTER_BOUND ( 'NONE', #37834, .T. ) ;
#7747 = CIRCLE ( 'NONE', #30838, 0.2540000000000000591 ) ;
#7748 = CARTESIAN_POINT ( 'NONE',  ( -4.611806494114576438, 117.9324678712513759, -0.9633187536371230486 ) ) ;
#7749 = CARTESIAN_POINT ( 'NONE',  ( -0.6996024724826829244, 105.8261742744577276, 5.294786660180783144 ) ) ;
#7750 = CARTESIAN_POINT ( 'NONE',  ( -29.43804252120325415, 67.00854438735211716, -1.523999999998907784 ) ) ;
#7751 = CARTESIAN_POINT ( 'NONE',  ( 7.936949992814905208, -1.433721018288910853, -2.821688713676304250 ) ) ;
#7752 = EDGE_CURVE ( 'NONE', #11776, #27053, #27493, .T. ) ;
#7753 = CARTESIAN_POINT ( 'NONE',  ( -5.177913976931286300, 56.51500000000000057, 5.372100000000003206 ) ) ;
#7754 = FACE_OUTER_BOUND ( 'NONE', #6733, .T. ) ;
#7755 = CARTESIAN_POINT ( 'NONE',  ( -58.03428750496623678, 2.144022121626051991, 0.09394692876219323807 ) ) ;
#7756 = DIRECTION ( 'NONE',  ( -0.8572391118119481179, -0.5149185422762151410, 0.000000000000000000 ) ) ;
#7757 = CARTESIAN_POINT ( 'NONE',  ( -23.25176476241890455, 142.6711341654318801, -0.007203867522443983124 ) ) ;
#7758 = AXIS2_PLACEMENT_3D ( 'NONE', #530, #6907, #23060 ) ;
#7759 = ORIENTED_EDGE ( 'NONE', *, *, #20338, .T. ) ;
#7760 = CARTESIAN_POINT ( 'NONE',  ( -58.16317756775203662, 1.603007233358586081, -1.028822313162498947 ) ) ;
#7761 = FACE_OUTER_BOUND ( 'NONE', #40766, .T. ) ;
#7762 = EDGE_LOOP ( 'NONE', ( #22981, #21952, #19465, #17069 ) ) ;
#7763 = CARTESIAN_POINT ( 'NONE',  ( -47.35734194463830704, 19.95394279970460971, -5.176037500948948100 ) ) ;
#7764 = CARTESIAN_POINT ( 'NONE',  ( -7.044606587285223931, 122.0729346620515088, -0.1407680048458704314 ) ) ;
#7765 = CARTESIAN_POINT ( 'NONE',  ( 4.690731670358166738, -15.11132977793584686, 4.439372980131230939 ) ) ;
#7766 = CARTESIAN_POINT ( 'NONE',  ( -16.68922378205042634, 153.6190162071354735, 1.533137601955099516 ) ) ;
#7767 = CIRCLE ( 'NONE', #34285, 16.60960244842765121 ) ;
#7768 = CARTESIAN_POINT ( 'NONE',  ( 23.16247218334346414, 146.6831645211815101, 1.199661776592803486 ) ) ;
#7769 = CARTESIAN_POINT ( 'NONE',  ( 22.07843093565568893, 149.7938220333360846, -0.9986438184040019594 ) ) ;
#7770 = CARTESIAN_POINT ( 'NONE',  ( -4.507778648822867495, 31.37953541088120346, -1.025544427737863362 ) ) ;
#7771 = CARTESIAN_POINT ( 'NONE',  ( -23.24214586660315263, 149.3282167461061931, -0.7955682979737040972 ) ) ;
#7772 = CARTESIAN_POINT ( 'NONE',  ( -49.88865472065932494, 16.47292688720559539, -4.948449357369904433 ) ) ;
#7773 = DIRECTION ( 'NONE',  ( -0.9454731675810332803, 0.3256999990547855828, -8.537024980200802097E-16 ) ) ;
#7774 = ORIENTED_EDGE ( 'NONE', *, *, #16668, .T. ) ;
#7775 = CARTESIAN_POINT ( 'NONE',  ( -8.767692638887638168, 117.8781970347225609, 0.2943759000137591841 ) ) ;
#7776 = CARTESIAN_POINT ( 'NONE',  ( -17.86368224974588514, 148.4245508482893854, 1.618106657999740516 ) ) ;
#7777 = CARTESIAN_POINT ( 'NONE',  ( -57.84388493117042174, 0.8425746053944089820, -1.050754030429361885 ) ) ;
#7778 = CARTESIAN_POINT ( 'NONE',  ( 5.031139012175321668, 119.0545008048120366, -0.9043826811606222593 ) ) ;
#7779 = VECTOR ( 'NONE', #20286, 1000.000000000000114 ) ;
#7780 = AXIS2_PLACEMENT_3D ( 'NONE', #9542, #38321, #16127 ) ;
#7781 = CARTESIAN_POINT ( 'NONE',  ( -0.9317526520580600158, -11.96253880033681050, -0.2928614735302202954 ) ) ;
#7782 = CARTESIAN_POINT ( 'NONE',  ( -13.69970117413534361, 155.7522398296385404, -1.951476099255863517 ) ) ;
#7783 = CARTESIAN_POINT ( 'NONE',  ( -48.04822308881582416, 19.89521662531995005, -5.294633059834412236 ) ) ;
#7784 = CARTESIAN_POINT ( 'NONE',  ( -3.009276887026423264, 50.13146620154573441, 1.210121013456480377 ) ) ;
#7785 = CARTESIAN_POINT ( 'NONE',  ( 1.846154440359644600, 156.5029897098349636, -0.9826124536999807368 ) ) ;
#7786 = CARTESIAN_POINT ( 'NONE',  ( -10.18105065676974519, 125.9743313966586129, -0.2034416216762103546 ) ) ;
#7787 = EDGE_LOOP ( 'NONE', ( #37073, #12701, #228, #40316, #26252 ) ) ;
#7788 = CARTESIAN_POINT ( 'NONE',  ( -10.84669103489419761, 122.6724665872831679, -1.607685377936339810 ) ) ;
#7789 = CARTESIAN_POINT ( 'NONE',  ( 5.320894714828252603, -15.22957080661538320, -0.4730099507937148284 ) ) ;
#7790 = TOROIDAL_SURFACE ( 'NONE', #3019, 0.7620000000000000107, 0.2540000000000000036 ) ;
#7791 = CARTESIAN_POINT ( 'NONE',  ( -15.96130909653717111, 80.00612572611477447, 1.269999999999997575 ) ) ;
#7792 = CARTESIAN_POINT ( 'NONE',  ( -4.437756799117888562, 118.1258187118189369, -0.7325781917677525179 ) ) ;
#7793 = CARTESIAN_POINT ( 'NONE',  ( -52.06546789126484498, 13.38259882428268632, -4.575081192416392106 ) ) ;
#7794 = CARTESIAN_POINT ( 'NONE',  ( 4.065926199369043204, 118.2429491485453497, 0.3080910687088499467 ) ) ;
#7795 = CARTESIAN_POINT ( 'NONE',  ( 5.440231158483206819, 156.5946142756450570, 1.801097700867929863 ) ) ;
#7796 = CARTESIAN_POINT ( 'NONE',  ( -13.11133394554952680, 57.78499999999998948, 9.234417301169688841 ) ) ;
#7797 = CARTESIAN_POINT ( 'NONE',  ( 3.703049682113265018, 116.6240124373522065, 0.07399574541707880371 ) ) ;
#7798 = CARTESIAN_POINT ( 'NONE',  ( -3.861838729977780993, 14.11015702457025078, 7.483763204152318771 ) ) ;
#7799 = CARTESIAN_POINT ( 'NONE',  ( 9.821648630411557335, 124.8790005272986861, 0.5336917924355371046 ) ) ;
#7800 = CARTESIAN_POINT ( 'NONE',  ( 14.68046753700549623, 156.0817623197167450, -0.7569547985229806430 ) ) ;
#7801 = CARTESIAN_POINT ( 'NONE',  ( 5.334231700979342961, 105.1224708049047649, -0.08243647111397434113 ) ) ;
#7802 = CARTESIAN_POINT ( 'NONE',  ( -5.078986093043186045, 97.88346620154572975, -0.1014902294541238092 ) ) ;
#7803 = CARTESIAN_POINT ( 'NONE',  ( -57.51979792895002674, 1.380172231454854348, 0.6550001595469883142 ) ) ;
#7804 = EDGE_CURVE ( 'NONE', #35632, #34680, #20796, .T. ) ;
#7805 = CARTESIAN_POINT ( 'NONE',  ( -15.93439728059136939, 121.0320206851898206, -0.2674320648195325223 ) ) ;
#7806 = ORIENTED_EDGE ( 'NONE', *, *, #37587, .F. ) ;
#7807 = CARTESIAN_POINT ( 'NONE',  ( -46.60530155212501313, 26.17382724835480445, -0.08466666666667589658 ) ) ;
#7808 = CARTESIAN_POINT ( 'NONE',  ( 7.890037743085640543, 122.1789050061608179, -0.5073752957019501686 ) ) ;
#7809 = LINE ( 'NONE', #40398, #17604 ) ;
#7810 = ORIENTED_EDGE ( 'NONE', *, *, #1083, .T. ) ;
#7811 = CARTESIAN_POINT ( 'NONE',  ( 2.051715782278035416, 115.6909491485438650, -1.638092376821394192 ) ) ;
#7812 = CARTESIAN_POINT ( 'NONE',  ( -15.49830880841133585, 147.8629129908177049, -0.8994996151558259934 ) ) ;
#7813 = CARTESIAN_POINT ( 'NONE',  ( 4.637598599007382916, -11.68863464395987428, 0.6963472677309354708 ) ) ;
#7814 = CARTESIAN_POINT ( 'NONE',  ( -10.16518949684075324, 157.7687470436769388, 1.006875576665116956 ) ) ;
#7815 = CARTESIAN_POINT ( 'NONE',  ( -5.423544988499506836, 78.92590603608628896, -5.135347845727594063 ) ) ;
#7816 = CARTESIAN_POINT ( 'NONE',  ( 15.69471450241202426, 120.8333755831694702, 0.3643268586347851445 ) ) ;
#7817 = EDGE_LOOP ( 'NONE', ( #17794, #40352, #13993, #5202 ) ) ;
#7818 = CARTESIAN_POINT ( 'NONE',  ( 3.315635589170360831, -10.27688868798473720, -3.234826238065521053 ) ) ;
#7819 = CARTESIAN_POINT ( 'NONE',  ( -6.896076486346299994, 117.1676486657671177, -0.1523180551073340938 ) ) ;
#7820 = CARTESIAN_POINT ( 'NONE',  ( -6.059261036834480585, 64.39150124418100063, 5.016499999999999737 ) ) ;
#7821 = LINE ( 'NONE', #27192, #6111 ) ;
#7822 = ORIENTED_EDGE ( 'NONE', *, *, #35344, .F. ) ;
#7823 = CARTESIAN_POINT ( 'NONE',  ( 6.312484072712937433, 119.3915106940810205, 1.259512802889745764 ) ) ;
#7824 = CARTESIAN_POINT ( 'NONE',  ( -1.959332070151295291, -8.942847522256865744, 4.198131957625402144 ) ) ;
#7825 = CARTESIAN_POINT ( 'NONE',  ( 10.11685142855833774, 157.7687470436769388, 1.412159022929360797 ) ) ;
#7826 = CARTESIAN_POINT ( 'NONE',  ( -58.62613161865938594, -0.2841797903866821740, -0.3870556671703427321 ) ) ;
#7827 = CARTESIAN_POINT ( 'NONE',  ( 20.41374081727966328, 149.7738053052645171, -1.564883410832889288 ) ) ;
#7828 = CARTESIAN_POINT ( 'NONE',  ( 0.2036312542886812293, -3.545347522689146214, -4.628372119175537591 ) ) ;
#7829 = CARTESIAN_POINT ( 'NONE',  ( -12.78669781772278924, 156.8686255264331635, -1.389142476906146673 ) ) ;
#7830 = VERTEX_POINT ( 'NONE', #16560 ) ;
#7831 = CARTESIAN_POINT ( 'NONE',  ( -1.594039003485612227, 156.2604006213118453, 0.1692965565027966801 ) ) ;
#7832 = CARTESIAN_POINT ( 'NONE',  ( 5.611968257679588845, -14.69514533571547688, 3.041973840610588287 ) ) ;
#7833 = DIRECTION ( 'NONE',  ( 0.8745520943968235761, -0.4849315768086558398, 4.268512490100410909E-16 ) ) ;
#7834 = CARTESIAN_POINT ( 'NONE',  ( -4.731576593360331096, 114.9758031406737615, -1.766933436629785525 ) ) ;
#7835 = ORIENTED_EDGE ( 'NONE', *, *, #9252, .F. ) ;
#7836 = CARTESIAN_POINT ( 'NONE',  ( 10.89600635431576592, 121.6366708983051836, 1.687201357748379316 ) ) ;
#7837 = CARTESIAN_POINT ( 'NONE',  ( -10.41103689192127568, 56.51499999999998636, -5.203122797516516407 ) ) ;
#7838 = EDGE_CURVE ( 'NONE', #20535, #6660, #9093, .T. ) ;
#7839 = CARTESIAN_POINT ( 'NONE',  ( -10.15441061790785682, 81.86333342972157823, -1.523999999999999133 ) ) ;
#7840 = CARTESIAN_POINT ( 'NONE',  ( -9.476822779618647274, 118.5748184150550060, 0.6643292918320550244 ) ) ;
#7841 = CARTESIAN_POINT ( 'NONE',  ( -0.4402761300873825334, 6.286315195291644287, -8.460265346311377499 ) ) ;
#7842 = CARTESIAN_POINT ( 'NONE',  ( 16.21957319403749054, 147.1082353761072454, 1.436993664011567029 ) ) ;
#7843 = CARTESIAN_POINT ( 'NONE',  ( -6.559134203278482289, 78.24119908707510263, -1.523999999999996469 ) ) ;
#7844 = EDGE_CURVE ( 'NONE', #6518, #16326, #28820, .T. ) ;
#7845 = VECTOR ( 'NONE', #10626, 1000.000000000000000 ) ;
#7846 = CARTESIAN_POINT ( 'NONE',  ( 22.28323889858834050, 137.0232865695268458, -0.2611169771296153463 ) ) ;
#7847 = FACE_OUTER_BOUND ( 'NONE', #11357, .T. ) ;
#7848 = CARTESIAN_POINT ( 'NONE',  ( -57.35194221082588939, 1.902352115738135119, 1.527398156819058661 ) ) ;
#7849 = LINE ( 'NONE', #34045, #15996 ) ;
#7850 = CARTESIAN_POINT ( 'NONE',  ( -57.64973313486724038, 1.352533784701764885, 1.499908592384902706 ) ) ;
#7851 = CARTESIAN_POINT ( 'NONE',  ( -57.63560179895036129, 1.846074579945612637, 1.702420071201910412 ) ) ;
#7852 = ADVANCED_FACE ( 'NONE', ( #8665 ), #31511, .T. ) ;
#7853 = CARTESIAN_POINT ( 'NONE',  ( -4.415273592266121483, 118.1795755137017352, 0.3920396191190627100 ) ) ;
#7854 = CARTESIAN_POINT ( 'NONE',  ( 1.156078607266118219, 106.1808064897588224, -5.165548525996213058 ) ) ;
#7855 = ORIENTED_EDGE ( 'NONE', *, *, #29567, .F. ) ;
#7856 = CARTESIAN_POINT ( 'NONE',  ( -46.40591231939538375, 23.70796668624020853, 2.618124260499386402 ) ) ;
#7857 = CARTESIAN_POINT ( 'NONE',  ( 8.278265034794616284, 120.3444625154268266, -1.110562897522293868 ) ) ;
#7858 = CARTESIAN_POINT ( 'NONE',  ( -6.134665891606804422, 119.5049778551863682, -0.5179261928985368080 ) ) ;
#7859 = CARTESIAN_POINT ( 'NONE',  ( 4.390279874354320988, 118.1641264082274745, 0.6591387255275874546 ) ) ;
#7860 = CARTESIAN_POINT ( 'NONE',  ( -16.28325953274117310, 146.1553843108282820, -1.442930602569014953 ) ) ;
#7861 = CARTESIAN_POINT ( 'NONE',  ( -0.5919055904364763920, 115.7030221220078658, -1.760227757477109467 ) ) ;
#7862 = CARTESIAN_POINT ( 'NONE',  ( 4.320748297369637392, 118.1651004037386059, -0.5003675618858194341 ) ) ;
#7863 = ORIENTED_EDGE ( 'NONE', *, *, #13113, .T. ) ;
#7864 = CARTESIAN_POINT ( 'NONE',  ( 5.284833012248379980, 116.4655405006298849, -0.8823810258511326499 ) ) ;
#7865 = CARTESIAN_POINT ( 'NONE',  ( -10.87485472805872000, 124.6990478933366404, -1.296628760762302823 ) ) ;
#7866 = ADVANCED_FACE ( 'NONE', ( #27619 ), #4859, .F. ) ;
#7867 = CARTESIAN_POINT ( 'NONE',  ( 0.09004192032669379453, 116.0444662015457169, -6.160295767268807232 ) ) ;
#7868 = CARTESIAN_POINT ( 'NONE',  ( -44.75127360237820540, 21.22985803517970638, 3.557274316435921513 ) ) ;
#7869 = DIRECTION ( 'NONE',  ( 5.188838149069472160E-16, -1.699382548006136559E-16, -1.000000000000000000 ) ) ;
#7870 = CARTESIAN_POINT ( 'NONE',  ( -7.767741303917714113, 154.6911059042232353, 0.01209887248576701525 ) ) ;
#7871 = FACE_OUTER_BOUND ( 'NONE', #20094, .T. ) ;
#7872 = CARTESIAN_POINT ( 'NONE',  ( 22.58684024723470785, 150.0155710288180444, 1.417619447182237646 ) ) ;
#7873 = CARTESIAN_POINT ( 'NONE',  ( 5.664977208693799504, 77.01756249999996840, -5.033228321271210781 ) ) ;
#7874 = CARTESIAN_POINT ( 'NONE',  ( 3.172822981795960562, -14.65879537465078464, 0.2101774045261552148 ) ) ;
#7875 = CARTESIAN_POINT ( 'NONE',  ( -17.49586834669434765, 149.8167423968465073, 1.704004628023328083 ) ) ;
#7876 = CARTESIAN_POINT ( 'NONE',  ( -0.4938630982110026046, -9.903502963049303887, 0.8462501600425517134 ) ) ;
#7877 = CARTESIAN_POINT ( 'NONE',  ( -22.91074218474016178, 142.4877946823990271, -1.320775467724695007 ) ) ;
#7878 = CARTESIAN_POINT ( 'NONE',  ( 0.04477287412000752198, 14.82196177864132380, -0.9729305925282246692 ) ) ;
#7879 = ORIENTED_EDGE ( 'NONE', *, *, #29765, .T. ) ;
#7880 = CARTESIAN_POINT ( 'NONE',  ( -50.67046617086457161, 13.01238886216411039, 1.492009926703871336 ) ) ;
#7881 = APPLICATION_PROTOCOL_DEFINITION ( 'draft international standard', 'automotive_design', 1998, #24331 ) ;
#7882 = CIRCLE ( 'NONE', #30989, 0.2540000000000010583 ) ;
#7883 = CARTESIAN_POINT ( 'NONE',  ( -16.10174665100988989, 146.3760696504137684, 0.5323012926561623281 ) ) ;
#7884 = CARTESIAN_POINT ( 'NONE',  ( 4.982342844640083257, -12.32172870019713962, 1.713706004506841740 ) ) ;
#7885 = CARTESIAN_POINT ( 'NONE',  ( 7.013665818177395650, 155.6889469082406947, -1.337060831506289071 ) ) ;
#7886 = ORIENTED_EDGE ( 'NONE', *, *, #31245, .F. ) ;
#7887 = CARTESIAN_POINT ( 'NONE',  ( 3.999473940548379680, 115.7036087109788838, 1.581720450462331673 ) ) ;
#7888 = CARTESIAN_POINT ( 'NONE',  ( 3.136003201302111076, -14.34114629734795088, 4.029177829137042366 ) ) ;
#7889 = CARTESIAN_POINT ( 'NONE',  ( -4.753076465732039679, 117.6359550804434662, -1.138063527254628671 ) ) ;
#7890 = EDGE_CURVE ( 'NONE', #26236, #20434, #2190, .T. ) ;
#7891 = CARTESIAN_POINT ( 'NONE',  ( 5.978688551911849558, 155.3719879121972838, 0.01966617979267130945 ) ) ;
#7892 = ORIENTED_EDGE ( 'NONE', *, *, #14938, .T. ) ;
#7893 = CARTESIAN_POINT ( 'NONE',  ( 6.715107731706551064, 119.1290971219625021, 1.270026890958220855 ) ) ;
#7894 = CARTESIAN_POINT ( 'NONE',  ( 1.698749669598698109, 106.4949638843832247, 5.056121066458325153 ) ) ;
#7895 = CARTESIAN_POINT ( 'NONE',  ( -8.723850037987370243, 68.58388863026053173, 1.524000000000003352 ) ) ;
#7896 = EDGE_CURVE ( 'NONE', #15736, #15805, #2979, .T. ) ;
#7897 = DIRECTION ( 'NONE',  ( -0.02488342977054593119, -0.9876883405951414341, -0.1544427297585422298 ) ) ;
#7898 = CARTESIAN_POINT ( 'NONE',  ( 14.75425959148282828, 120.3062992333385921, 0.06863422566743783426 ) ) ;
#7899 = CARTESIAN_POINT ( 'NONE',  ( -17.08598887363762131, 83.79821757228496892, -1.524000000000002908 ) ) ;
#7900 = CARTESIAN_POINT ( 'NONE',  ( 1.920978177995904979, -15.71867150285087611, 5.654812409921664340 ) ) ;
#7901 = CARTESIAN_POINT ( 'NONE',  ( -4.943487193438446781, 117.5911938081067092, -0.9706830346222778960 ) ) ;
#7902 = CARTESIAN_POINT ( 'NONE',  ( 16.23079787743079194, 153.4734386769207504, 2.282812701028141600 ) ) ;
#7903 = CIRCLE ( 'NONE', #36491, 0.6350000000000001199 ) ;
#7904 = ORIENTED_EDGE ( 'NONE', *, *, #40026, .F. ) ;
#7905 = CARTESIAN_POINT ( 'NONE',  ( -8.420209349088564110, 12.38497237326411415, -0.2929423126682718648 ) ) ;
#7906 = CARTESIAN_POINT ( 'NONE',  ( 8.624984000141996177, 118.6231719595668892, -0.7976843706328619055 ) ) ;
#7907 = CARTESIAN_POINT ( 'NONE',  ( -3.137457178758016330, 117.8122656274855871, -0.9631651297103497322 ) ) ;
#7908 = DIRECTION ( 'NONE',  ( 6.353134868986659519E-16, -1.000000000000000000, 0.000000000000000000 ) ) ;
#7909 = CARTESIAN_POINT ( 'NONE',  ( -5.586884702347496123, 94.32746620154571815, -0.1116392523995361624 ) ) ;
#7910 = CARTESIAN_POINT ( 'NONE',  ( -4.888957423522264811, 105.1215310813731207, 2.142498686656161055 ) ) ;
#7911 = CARTESIAN_POINT ( 'NONE',  ( 3.102408547967445696, -0.5812848888516047863, -3.453265078539196509 ) ) ;
#7912 = CARTESIAN_POINT ( 'NONE',  ( -20.59944062528794362, 79.83666051618703818, -1.524000000000004018 ) ) ;
#7913 = CARTESIAN_POINT ( 'NONE',  ( -4.766356317893496453, 118.5264896598256854, 0.8410930105509721866 ) ) ;
#7914 = CARTESIAN_POINT ( 'NONE',  ( 2.376025398756717699, -14.92724974027714779, 5.073178661078445728 ) ) ;
#7915 = CARTESIAN_POINT ( 'NONE',  ( 4.585195778441632619, 124.9344662015457459, 0.09162312381275083961 ) ) ;
#7916 = EDGE_CURVE ( 'NONE', #25568, #27127, #18591, .T. ) ;
#7917 = CARTESIAN_POINT ( 'NONE',  ( 2.958531772299236362, 39.20946620154573026, 1.329372033065076453 ) ) ;
#7918 = CARTESIAN_POINT ( 'NONE',  ( 13.85159022459153988, 16.51000000000000156, -5.016499999999999737 ) ) ;
#7919 = VERTEX_POINT ( 'NONE', #14826 ) ;
#7920 = CARTESIAN_POINT ( 'NONE',  ( -5.255166069342940283, 105.1223876010384259, -0.9307257834050973733 ) ) ;
#7921 = CARTESIAN_POINT ( 'NONE',  ( 2.341541575351651083, -15.74615379138004378, 5.495207524874286875 ) ) ;
#7922 = CARTESIAN_POINT ( 'NONE',  ( -13.00445675891842257, 122.7019651155717384, 1.321991537619922719 ) ) ;
#7923 = CARTESIAN_POINT ( 'NONE',  ( 0.2723526006440308844, 25.78125159710042169, 0.9401034630801221592 ) ) ;
#7924 = ORIENTED_EDGE ( 'NONE', *, *, #26964, .F. ) ;
#7925 = ORIENTED_EDGE ( 'NONE', *, *, #14409, .T. ) ;
#7926 = CARTESIAN_POINT ( 'NONE',  ( -6.606029807653651701E-14, 92.04146620154574521, -3.372746026535634231E-18 ) ) ;
#7927 = CARTESIAN_POINT ( 'NONE',  ( -0.1065646865916382441, 105.8844662015457061, 5.332932678536314697 ) ) ;
#7928 = CARTESIAN_POINT ( 'NONE',  ( -9.413719431533529303, 122.9055586947561522, 0.7725895697485187785 ) ) ;
#7929 = EDGE_CURVE ( 'NONE', #15919, #42038, #11856, .T. ) ;
#7930 = CARTESIAN_POINT ( 'NONE',  ( -5.309060684617390516E-14, 83.56599999999998829, 0.000000000000000000 ) ) ;
#7931 = CARTESIAN_POINT ( 'NONE',  ( 12.69375283655731934, 153.7453525671159298, -1.672805011026380573 ) ) ;
#7932 = CARTESIAN_POINT ( 'NONE',  ( -13.64080552068802277, 122.3361261571837986, -1.764911742735522315 ) ) ;
#7933 = AXIS2_PLACEMENT_3D ( 'NONE', #35526, #21873, #28495 ) ;
#7934 = CARTESIAN_POINT ( 'NONE',  ( 4.401000572156880786, 118.1832674401186409, -0.4088722398549547998 ) ) ;
#7935 = CARTESIAN_POINT ( 'NONE',  ( 9.191362964797985313, 123.9301100385560943, -0.1344743934557742215 ) ) ;
#7936 = AXIS2_PLACEMENT_3D ( 'NONE', #38854, #6070, #100 ) ;
#7937 = ORIENTED_EDGE ( 'NONE', *, *, #7916, .F. ) ;
#7938 = CARTESIAN_POINT ( 'NONE',  ( 3.205191379615736746, -14.47393913169138102, 3.051678166811226500 ) ) ;
#7939 = EDGE_CURVE ( 'NONE', #27187, #37417, #17303, .T. ) ;
#7940 = CARTESIAN_POINT ( 'NONE',  ( -4.890164892654324191, 117.4101971730238461, 0.9753743779596022456 ) ) ;
#7941 = EDGE_CURVE ( 'NONE', #15033, #26127, #14615, .T. ) ;
#7942 = CARTESIAN_POINT ( 'NONE',  ( -48.15691857872906922, 19.01861963076551021, 5.213839621080547992 ) ) ;
#7943 = CARTESIAN_POINT ( 'NONE',  ( 1.463615122064738427, -3.970138727222522590, -4.384008014421088895 ) ) ;
#7944 = CARTESIAN_POINT ( 'NONE',  ( 14.05412825714257608, 131.1061190467503934, 1.842221413061617241 ) ) ;
#7945 = CARTESIAN_POINT ( 'NONE',  ( 2.393982948168581704, 36.72379010448016601, 1.601961539505906806 ) ) ;
#7946 = CARTESIAN_POINT ( 'NONE',  ( -6.983605877934339290, 124.9344662015457175, -0.1395490654994202828 ) ) ;
#7947 = CARTESIAN_POINT ( 'NONE',  ( -4.636761822055341042, 12.60011390031314349, 0.2095705037016724059 ) ) ;
#7948 = CARTESIAN_POINT ( 'NONE',  ( 15.38115207166213594, 147.8278496344100859, 0.4352178850651141073 ) ) ;
#7949 = CARTESIAN_POINT ( 'NONE',  ( 4.834527910505758364, 118.7629491485453030, -0.4653476702560417344 ) ) ;
#7950 = CARTESIAN_POINT ( 'NONE',  ( -57.71946847630993460, 1.146847591362354368, -1.351507486235954403 ) ) ;
#7951 = CARTESIAN_POINT ( 'NONE',  ( -5.538962611300139116, 116.7971013310818620, -0.4462307559783619815 ) ) ;
#7952 = VECTOR ( 'NONE', #27624, 1000.000000000000000 ) ;
#7953 = CARTESIAN_POINT ( 'NONE',  ( 0.005099097580972779785, 122.5569158606516993, -0.2551796940110859224 ) ) ;
#7954 = DIRECTION ( 'NONE',  ( 0.1906721105965186736, -0.9816537812491066273, 0.000000000000000000 ) ) ;
#7955 = CARTESIAN_POINT ( 'NONE',  ( 2.074264724554227612, -15.58053249244905381, 5.900626476732243830 ) ) ;
#7956 = CARTESIAN_POINT ( 'NONE',  ( -5.177913976931298734, 78.94499979771843812, 5.372100000000002318 ) ) ;
#7957 = CARTESIAN_POINT ( 'NONE',  ( 6.431785950458272616, 8.712657024569978148, -5.436233950049250474 ) ) ;
#7958 = CARTESIAN_POINT ( 'NONE',  ( -5.449044798931593547, 57.14999999999999858, 5.145813327217799049 ) ) ;
#7959 = CARTESIAN_POINT ( 'NONE',  ( -5.586884702347497011, 104.6144662015457243, -0.1116392523995361624 ) ) ;
#7960 = CARTESIAN_POINT ( 'NONE',  ( -58.20820809768405013, 1.420579653404072218, 1.355822160094593887 ) ) ;
#7961 = CARTESIAN_POINT ( 'NONE',  ( 0.001261869788119350478, 124.3520329708341876, -0.06314912420803914239 ) ) ;
#7962 = CARTESIAN_POINT ( 'NONE',  ( -8.196853576810003261, 117.5993832199734328, 0.1745776481207347852 ) ) ;
#7963 = VECTOR ( 'NONE', #38861, 1000.000000000000000 ) ;
#7964 = ORIENTED_EDGE ( 'NONE', *, *, #10499, .T. ) ;
#7965 = CARTESIAN_POINT ( 'NONE',  ( -55.64884842185075087, 8.819639511685364752, -1.021878145082219635 ) ) ;
#7966 = ORIENTED_EDGE ( 'NONE', *, *, #39208, .F. ) ;
#7967 = CARTESIAN_POINT ( 'NONE',  ( -45.96492958221768532, 21.02066589182467382, -4.445716362542115441 ) ) ;
#7968 = CARTESIAN_POINT ( 'NONE',  ( -11.83539255247756117, 152.0195595274622349, -0.2364993098673504601 ) ) ;
#7969 = CARTESIAN_POINT ( 'NONE',  ( 2.850629920820032748, -15.47419331854960056, 5.714803783126763292 ) ) ;
#7970 = CARTESIAN_POINT ( 'NONE',  ( -9.089826843847044202, 119.3941581119689204, 1.016340006442031374 ) ) ;
#7971 = CARTESIAN_POINT ( 'NONE',  ( 13.85601021432049684, 120.6843904051541898, -0.7167389240433504893 ) ) ;
#7972 = CARTESIAN_POINT ( 'NONE',  ( -29.20503723471917823, 64.36951892211030213, 1.269999999999993356 ) ) ;
#7973 = CARTESIAN_POINT ( 'NONE',  ( -0.3042230016543463478, 116.5226405152084652, -0.1306790058978155589 ) ) ;
#7974 = EDGE_CURVE ( 'NONE', #2461, #537, #5700, .T. ) ;
#7975 = CARTESIAN_POINT ( 'NONE',  ( -49.99298857535946894, 16.30720399940068788, -4.926441425282844122 ) ) ;
#7976 = EDGE_LOOP ( 'NONE', ( #6703, #30391, #22393 ) ) ;
#7977 = CARTESIAN_POINT ( 'NONE',  ( -5.563241772947201902, 116.6983512803620471, -0.09199628343113541717 ) ) ;
#7978 = CARTESIAN_POINT ( 'NONE',  ( -5.873652769538547425, 120.2771794157441008, 0.8114825934776858096 ) ) ;
#7979 = CARTESIAN_POINT ( 'NONE',  ( -49.99139319293801975, 16.20859854215753515, -4.826775924100495274 ) ) ;
#7980 = CARTESIAN_POINT ( 'NONE',  ( 19.24794053165960150, 147.9830121424878939, -1.736014841626597471 ) ) ;
#7981 = CARTESIAN_POINT ( 'NONE',  ( -21.52700195390597671, 148.3057046726078170, -2.246165485461372846 ) ) ;
#7982 = CARTESIAN_POINT ( 'NONE',  ( -48.65005484009959957, 18.46594748123760965, -5.297328305960443018 ) ) ;
#7983 = CIRCLE ( 'NONE', #35195, 0.2540000000000000036 ) ;
#7984 = CARTESIAN_POINT ( 'NONE',  ( 1.496072496114335904, 120.3785564700922492, -0.3614901595391030176 ) ) ;
#7985 = CARTESIAN_POINT ( 'NONE',  ( -14.39766717389552397, 60.02151067229126369, -1.904999999999999805 ) ) ;
#7986 = ORIENTED_EDGE ( 'NONE', *, *, #41421, .F. ) ;
#7987 = CARTESIAN_POINT ( 'NONE',  ( -11.45041423386219215, 122.9335272575421669, -1.692945391654126386 ) ) ;
#7988 = CARTESIAN_POINT ( 'NONE',  ( 4.174810697594108611, -15.62279056926031728, 2.935701831792822514 ) ) ;
#7989 = CIRCLE ( 'NONE', #12053, 3.683000000000001162 ) ;
#7990 = FACE_OUTER_BOUND ( 'NONE', #19499, .T. ) ;
#7991 = CARTESIAN_POINT ( 'NONE',  ( -4.269880260387894033, 118.2136455867637466, -0.5281148321755492203 ) ) ;
#7992 = EDGE_CURVE ( 'NONE', #4862, #33118, #29487, .T. ) ;
#7993 = CARTESIAN_POINT ( 'NONE',  ( -55.60486134785667645, 7.243031971518515633, -3.140198620020504094 ) ) ;
#7994 = CIRCLE ( 'NONE', #31797, 0.6350000000000014522 ) ;
#7995 = CARTESIAN_POINT ( 'NONE',  ( -4.970228710897478308, 117.5383302079596746, 0.8106020663343151966 ) ) ;
#7996 = CARTESIAN_POINT ( 'NONE',  ( 18.00824595900788694, 147.8422069945528108, 2.338981374327670171 ) ) ;
#7997 = CARTESIAN_POINT ( 'NONE',  ( -17.14499999999999957, 71.11999999999999034, -1.904999999999999583 ) ) ;
#7998 = CARTESIAN_POINT ( 'NONE',  ( 13.67717291712360961, 119.6429072192227494, 0.2244666789651033056 ) ) ;
#7999 = CARTESIAN_POINT ( 'NONE',  ( 4.095665791538102063, 15.60827804425945331, 7.401523448874606892 ) ) ;
#8000 = CARTESIAN_POINT ( 'NONE',  ( 15.84614414026241924, 146.9522167609303267, 0.9100203137935939379 ) ) ;
#8001 = CARTESIAN_POINT ( 'NONE',  ( 4.973152232786927307, 117.3993868326352015, 0.9753084504214339923 ) ) ;
#8002 = CARTESIAN_POINT ( 'NONE',  ( 5.314256983240370324, 105.1224655745845382, -0.4585143440169748841 ) ) ;
#8003 = AXIS2_PLACEMENT_3D ( 'NONE', #17963, #4014, #35955 ) ;
#8004 = CARTESIAN_POINT ( 'NONE',  ( -58.35029634831491308, -0.2563984898762833309, 0.1830726351724760170 ) ) ;
#8005 = CARTESIAN_POINT ( 'NONE',  ( -6.904872195170285387, 117.1762911274595496, -0.05199240921585723124 ) ) ;
#8006 = ORIENTED_EDGE ( 'NONE', *, *, #2504, .T. ) ;
#8007 = CARTESIAN_POINT ( 'NONE',  ( -47.62967605938791849, 25.45029596856965171, -9.729597958152646858E-15 ) ) ;
#8008 = CARTESIAN_POINT ( 'NONE',  ( 5.796788256709977105, 121.1606928603264492, -0.2966676035594191796 ) ) ;
#8009 = CARTESIAN_POINT ( 'NONE',  ( -8.709803600792287881, 118.1821829479768553, 0.5645179937759793320 ) ) ;
#8010 = ORIENTED_EDGE ( 'NONE', *, *, #35498, .T. ) ;
#8011 = DIRECTION ( 'NONE',  ( -0.8745520943968249084, 0.4849315768086533418, -5.271987356194193006E-16 ) ) ;
#8012 = CARTESIAN_POINT ( 'NONE',  ( -15.82044549406361611, 146.2622375132148989, -0.6472507553222681675 ) ) ;
#8013 = CARTESIAN_POINT ( 'NONE',  ( 4.828046317437772572, -12.99562652935115636, 2.825559498992329832 ) ) ;
#8014 = CARTESIAN_POINT ( 'NONE',  ( -15.58647730463680325, 154.9569273371780298, 1.293949759430877533 ) ) ;
#8015 = CARTESIAN_POINT ( 'NONE',  ( 5.571852488405371062, 78.91397923090406152, -5.086862008547680780 ) ) ;
#8016 = CARTESIAN_POINT ( 'NONE',  ( 16.23049043870583930, 121.3954344197762083, 0.4305223454732414190 ) ) ;
#8017 = CARTESIAN_POINT ( 'NONE',  ( 10.39928917620358817, 153.1223395828141918, 0.2078025466733119664 ) ) ;
#8018 = ORIENTED_EDGE ( 'NONE', *, *, #15372, .T. ) ;
#8019 = CARTESIAN_POINT ( 'NONE',  ( 0.9593126492114073534, 18.43563504644844642, -0.1793159252426369810 ) ) ;
#8020 = CARTESIAN_POINT ( 'NONE',  ( -22.98446660148367826, 150.1594536303649932, -0.4849100737359563484 ) ) ;
#8021 = CARTESIAN_POINT ( 'NONE',  ( 5.008579095262371439, 117.3966161975143052, -0.7759206765000108419 ) ) ;
#8022 = VERTEX_POINT ( 'NONE', #21838 ) ;
#8023 = CARTESIAN_POINT ( 'NONE',  ( 5.078986093043053707, 94.83546620154572793, 0.1014902294541237954 ) ) ;
#8024 = ORIENTED_EDGE ( 'NONE', *, *, #2466, .F. ) ;
#8025 = CARTESIAN_POINT ( 'NONE',  ( -3.063299625903500800, 117.4009674993953780, 0.6350039608490424259 ) ) ;
#8026 = CARTESIAN_POINT ( 'NONE',  ( 3.679437910380295218, 2.726752568732802917, 2.794697870780981752 ) ) ;
#8027 = CARTESIAN_POINT ( 'NONE',  ( 22.07432572979840657, 148.5290936231802448, 2.031061984987305280 ) ) ;
#8028 = CARTESIAN_POINT ( 'NONE',  ( -56.42349525705788693, 3.945591430473524230, -2.427201670071943429 ) ) ;
#8029 = CARTESIAN_POINT ( 'NONE',  ( 20.28847770310427734, 149.9354415288716780, -1.565775960057087524 ) ) ;
#8030 = CARTESIAN_POINT ( 'NONE',  ( 0.8067276567327370529, -3.745225398377231674, -4.556403025205434609 ) ) ;
#8031 = CARTESIAN_POINT ( 'NONE',  ( -11.19826879832072031, 119.1264784044212632, -1.044736191152864091 ) ) ;
#8032 = CARTESIAN_POINT ( 'NONE',  ( 4.980187925143842342, 117.5315200247294456, -0.7740374538369801938 ) ) ;
#8033 = ORIENTED_EDGE ( 'NONE', *, *, #22149, .T. ) ;
#8034 = CARTESIAN_POINT ( 'NONE',  ( -8.102825354745354147, 122.8525693413601800, -0.01624079103423752349 ) ) ;
#8035 = CARTESIAN_POINT ( 'NONE',  ( 4.535621022044703743, -15.16026073378742822, 4.605481170969206062 ) ) ;
#8036 = CARTESIAN_POINT ( 'NONE',  ( 13.34576682144454196, 17.14499999999997115, -5.016499999999998849 ) ) ;
#8037 = CARTESIAN_POINT ( 'NONE',  ( 0.02808993038205571599, 117.9496054766756288, -1.405735097488628682 ) ) ;
#8038 = EDGE_LOOP ( 'NONE', ( #21208, #34655, #29672, #34261 ) ) ;
#8039 = CARTESIAN_POINT ( 'NONE',  ( 5.971676678096363489, 157.1185343457808301, 1.951309749225692558 ) ) ;
#8040 = DIRECTION ( 'NONE',  ( 5.188838149069472160E-16, -1.699382548006136559E-16, -1.000000000000000000 ) ) ;
#8041 = CARTESIAN_POINT ( 'NONE',  ( -20.37123700195715870, 79.57406833244878896, -1.524000000000003796 ) ) ;
#8042 = CARTESIAN_POINT ( 'NONE',  ( -12.95464425825008803, 119.9671592456446803, 0.6090756887631915140 ) ) ;
#8043 = CARTESIAN_POINT ( 'NONE',  ( 8.270632439779459943, 13.09856730479051912, 1.690137114335896751 ) ) ;
#8044 = CARTESIAN_POINT ( 'NONE',  ( 16.27374876192079256, 146.7930872653447523, 1.439762483169732876 ) ) ;
#8045 = DIRECTION ( 'NONE',  ( 0.9849462604886047856, 0.000000000000000000, 0.1728608224830407714 ) ) ;
#8046 = CARTESIAN_POINT ( 'NONE',  ( 23.15061725546894067, 148.7607265879045144, -0.2678260907677694758 ) ) ;
#8047 = DIRECTION ( 'NONE',  ( 0.000000000000000000, 1.000000000000000000, 0.000000000000000000 ) ) ;
#8048 = CARTESIAN_POINT ( 'NONE',  ( -55.27300860040548258, 6.262530169634048072, 2.859796270508659255 ) ) ;
#8049 = SURFACE_SIDE_STYLE ('',( #1260 ) ) ;
#8050 = CARTESIAN_POINT ( 'NONE',  ( -58.83227707057486811, -0.08366279997995551554, 0.2458995907044889129 ) ) ;
#8051 = CARTESIAN_POINT ( 'NONE',  ( -58.63368340525728684, -0.2968340078074506727, 0.3659978923735402456 ) ) ;
#8052 = LINE ( 'NONE', #28053, #30693 ) ;
#8053 = CARTESIAN_POINT ( 'NONE',  ( -4.254034338640801494, 118.2250400857918038, 0.3060042376985389612 ) ) ;
#8054 = CARTESIAN_POINT ( 'NONE',  ( 3.041860522939319189, 107.5209036112489969, -4.373094760128172886 ) ) ;
#8055 = EDGE_LOOP ( 'NONE', ( #13032, #42124 ) ) ;
#8056 = CARTESIAN_POINT ( 'NONE',  ( -53.83456308493991571, 9.379524109395250164, 3.755176697756422044 ) ) ;
#8057 = CARTESIAN_POINT ( 'NONE',  ( -8.270437544260451190, 120.1331483986364503, -1.449690397053889690 ) ) ;
#8058 = CARTESIAN_POINT ( 'NONE',  ( -5.183518906920142832, 115.4398124677065596, -1.515634836823671838 ) ) ;
#8059 = CARTESIAN_POINT ( 'NONE',  ( 4.303048441523191769, 118.2117257955810317, 0.4941738720055364742 ) ) ;
#8060 = CARTESIAN_POINT ( 'NONE',  ( -13.47315239181501845, 134.2048320552371763, -1.097568958570526165 ) ) ;
#8061 = CARTESIAN_POINT ( 'NONE',  ( 0.3943891902157575791, 117.3993832487344520, -1.481047929051600986 ) ) ;
#8062 = ORIENTED_EDGE ( 'NONE', *, *, #41616, .F. ) ;
#8063 = CARTESIAN_POINT ( 'NONE',  ( 4.256838582791900194, 16.71066835407712858, 1.825063967593055558 ) ) ;
#8064 = CARTESIAN_POINT ( 'NONE',  ( -4.884089373684617819, 156.1188696671683260, -1.381267178739763235 ) ) ;
#8065 = CARTESIAN_POINT ( 'NONE',  ( -6.474089935681887051E-14, 69.94346620154573202, 3.752704589293910110E-29 ) ) ;
#8066 = CARTESIAN_POINT ( 'NONE',  ( -43.98070909377825899, 21.30087824702203037, 2.736222515986834747 ) ) ;
#8067 = DIRECTION ( 'NONE',  ( -0.8745520943968235761, 0.4849315768086558953, -5.361993529360570985E-16 ) ) ;
#8068 = CARTESIAN_POINT ( 'NONE',  ( -5.338855604227259910, 121.3506614897932252, 0.002391977014555100173 ) ) ;
#8069 = AXIS2_PLACEMENT_3D ( 'NONE', #10510, #17317, #20921 ) ;
#8070 = CARTESIAN_POINT ( 'NONE',  ( 3.682264917456192332, 94.83546620154572793, 0.07358041635423968885 ) ) ;
#8071 = CARTESIAN_POINT ( 'NONE',  ( 7.798299699696582543, 158.6358315003295161, 0.8787250540639038876 ) ) ;
#8072 = DIRECTION ( 'NONE',  ( -0.9816537812491077375, -0.1906721105965138996, -4.769617732184456426E-16 ) ) ;
#8074 = CARTESIAN_POINT ( 'NONE',  ( 12.29982474031027806, 156.6574886424908470, -1.289654987246353857 ) ) ;
#8073 = CARTESIAN_POINT ( 'NONE',  ( 3.216700609619024931, -14.42020774479446921, 2.887214088933996337 ) ) ;
#8075 = CARTESIAN_POINT ( 'NONE',  ( -12.93728320859319147, 153.8477531742089468, 1.710492906883538167 ) ) ;
#8076 = AXIS2_PLACEMENT_3D ( 'NONE', #38255, #22657, #25468 ) ;
#8077 = CARTESIAN_POINT ( 'NONE',  ( 0.4551624184790937777, -5.041848893434334400, -0.8611515851349844652 ) ) ;
#8078 = CARTESIAN_POINT ( 'NONE',  ( -0.9591953284562637627, 116.7682604261274264, -0.2970936445032629769 ) ) ;
#8079 = CARTESIAN_POINT ( 'NONE',  ( -0.07513956969218944792, 19.57165678886816096, 0.9711860325417217554 ) ) ;
#8080 = EDGE_LOOP ( 'NONE', ( #15022, #41657, #10257, #2611 ) ) ;
#8081 = CARTESIAN_POINT ( 'NONE',  ( -52.67395729902614221, 10.59333423579336753, 2.513629069394781368 ) ) ;
#8082 = CARTESIAN_POINT ( 'NONE',  ( -9.185752227574177198, 123.6526633469202920, 0.3199782652467454969 ) ) ;
#8083 = CARTESIAN_POINT ( 'NONE',  ( 4.994336218630399671, -12.17445384341683834, 1.469335147697719890 ) ) ;
#8084 = CARTESIAN_POINT ( 'NONE',  ( 3.633016119382470599, 156.6183338678525558, -1.377765736259032536 ) ) ;
#8085 = EDGE_LOOP ( 'NONE', ( #16010, #22347, #18581, #33928, #38964, #10390, #22184, #27259, #33297, #16982, #12121, #3599 ) ) ;
#8086 = CARTESIAN_POINT ( 'NONE',  ( 0.7503318161881147308, 115.7029095348785148, 1.755759173997271105 ) ) ;
#8087 = CARTESIAN_POINT ( 'NONE',  ( 3.066387819753066069, -14.51305101688413224, 3.912045622741378903 ) ) ;
#8088 = DIRECTION ( 'NONE',  ( -5.188838149069471174E-16, 1.699382548006136313E-16, 1.000000000000000000 ) ) ;
#8089 = EDGE_CURVE ( 'NONE', #29909, #11064, #9752, .T. ) ;
#8090 = CARTESIAN_POINT ( 'NONE',  ( 10.41298992473515561, 153.0987333575537548, 0.09138415589099070646 ) ) ;
#8091 = ORIENTED_EDGE ( 'NONE', *, *, #38040, .F. ) ;
#8092 = CARTESIAN_POINT ( 'NONE',  ( 20.22212501804812490, 145.4934252350392114, 2.489959791085248231 ) ) ;
#8093 = CARTESIAN_POINT ( 'NONE',  ( 2.743188893672867223, 107.9147049449198903, 4.446318134730120164 ) ) ;
#8094 = DIRECTION ( 'NONE',  ( -0.9998004120163608288, -5.205824365704082573E-17, -0.01997839162482749342 ) ) ;
#8095 = DIRECTION ( 'NONE',  ( -5.188838149069471174E-16, 1.699382548006136313E-16, 1.000000000000000000 ) ) ;
#8096 = CARTESIAN_POINT ( 'NONE',  ( 23.19846888548980601, 149.6199392087789306, 0.2334144245939554496 ) ) ;
#8097 = CIRCLE ( 'NONE', #28497, 5.588000000000006295 ) ;
#8098 = DIRECTION ( 'NONE',  ( 9.627370216492862708E-17, 1.000000000000000000, -0.000000000000000000 ) ) ;
#8099 = CARTESIAN_POINT ( 'NONE',  ( 1.702263513459753907, -15.37342380949326071, 5.866026421007169311 ) ) ;
#8100 = CARTESIAN_POINT ( 'NONE',  ( -18.35410564743290607, 77.35382415001784295, 5.016499999999999737 ) ) ;
#8101 = FACE_OUTER_BOUND ( 'NONE', #12928, .T. ) ;
#8102 = CARTESIAN_POINT ( 'NONE',  ( -4.783018391820325732, 117.8919472439429796, 0.7199156508651073372 ) ) ;
#8103 = EDGE_LOOP ( 'NONE', ( #30874, #33955, #14459, #18374 ) ) ;
#8104 = CARTESIAN_POINT ( 'NONE',  ( 5.064488095677227797, 115.7029491485453150, -1.196137279639045259 ) ) ;
#8105 = CARTESIAN_POINT ( 'NONE',  ( -8.512111711805967929, 118.9720400677293810, -1.270775419876498669 ) ) ;
#8106 = CARTESIAN_POINT ( 'NONE',  ( -0.3635706870684802805, 106.2969274751293938, -5.168771910137537340 ) ) ;
#8107 = CARTESIAN_POINT ( 'NONE',  ( 4.734360898042774046, 117.6653353942706843, 1.129076436732644906 ) ) ;
#8108 = CARTESIAN_POINT ( 'NONE',  ( 17.14499999999999957, 71.11999999999999034, 5.016499999999999737 ) ) ;
#8109 = CARTESIAN_POINT ( 'NONE',  ( -5.075364051007695387, 105.1217683680384027, 1.652234970701472738 ) ) ;
#8110 = CARTESIAN_POINT ( 'NONE',  ( -0.5496829067194369811, 0.7180641350488168317, -4.598301960397928489 ) ) ;
#8111 = DIRECTION ( 'NONE',  ( -1.000000000000000000, 1.365923996832131856E-16, 0.000000000000000000 ) ) ;
#8112 = CARTESIAN_POINT ( 'NONE',  ( -5.237832120027548832, 115.7029491485453860, -1.023639123012231034 ) ) ;
#8113 = CARTESIAN_POINT ( 'NONE',  ( 3.302240090359226610, -14.10740904597654399, 3.820541190522989350 ) ) ;
#8114 = EDGE_CURVE ( 'NONE', #2780, #27477, #5479, .T. ) ;
#8115 = CARTESIAN_POINT ( 'NONE',  ( 4.036547470782338998, 117.2022048034790487, -0.8857695023546173774 ) ) ;
#8116 = CARTESIAN_POINT ( 'NONE',  ( -4.923982053054707819, 28.56637592605547837, 2.110792280427853385 ) ) ;
#8117 = CARTESIAN_POINT ( 'NONE',  ( -0.8472532152023458663, 115.7028161379835893, 1.722469557941253226 ) ) ;
#8118 = ORIENTED_EDGE ( 'NONE', *, *, #12274, .T. ) ;
#8119 = CARTESIAN_POINT ( 'NONE',  ( -5.137756011363697084, 104.6144662015446585, -1.444153010337383192 ) ) ;
#8120 = CARTESIAN_POINT ( 'NONE',  ( 4.493636945811098293, -15.48460478268967577, 1.406059860741644574 ) ) ;
#8121 = CARTESIAN_POINT ( 'NONE',  ( -12.60853345060003328, 122.2722385251898771, 1.300450782769299929 ) ) ;
#8122 = CARTESIAN_POINT ( 'NONE',  ( -0.2871545817224689379, 15.30011720780053430, 0.9385489134671207712 ) ) ;
#8123 = ORIENTED_EDGE ( 'NONE', *, *, #38619, .F. ) ;
#8124 = ORIENTED_EDGE ( 'NONE', *, *, #37081, .F. ) ;
#8125 = FACE_OUTER_BOUND ( 'NONE', #3961, .T. ) ;
#8126 = CARTESIAN_POINT ( 'NONE',  ( 4.551180572033469929, 124.4408722044843927, 0.1097773164883772967 ) ) ;
#8127 = CARTESIAN_POINT ( 'NONE',  ( -4.403754988258326897, 120.5100497556178567, 0.5130326506441985623 ) ) ;
#8128 = DIRECTION ( 'NONE',  ( 9.627370216492862708E-17, 1.000000000000000000, -0.000000000000000000 ) ) ;
#8129 = AXIS2_PLACEMENT_3D ( 'NONE', #12932, #41923, #390 ) ;
#8130 = CARTESIAN_POINT ( 'NONE',  ( 4.625065594204414765, 118.0227253997019261, -0.6695745435591143879 ) ) ;
#8131 = CARTESIAN_POINT ( 'NONE',  ( 4.293775319275984437, 119.8084884740358547, -0.7325880323699281993 ) ) ;
#8132 = CIRCLE ( 'NONE', #31934, 6.349999999999999645 ) ;
#8133 = CARTESIAN_POINT ( 'NONE',  ( -3.146714701749098619, 118.3302933575512412, -0.8734028913305706965 ) ) ;
#8134 = CARTESIAN_POINT ( 'NONE',  ( 11.58677707360137532, 55.98894877578617724, 4.474811398758258285 ) ) ;
#8135 = EDGE_CURVE ( 'NONE', #9063, #19512, #11119, .T. ) ;
#8136 = CARTESIAN_POINT ( 'NONE',  ( 4.298646650716237971, 118.2143447890847767, -0.3450677996601986819 ) ) ;
#8137 = CARTESIAN_POINT ( 'NONE',  ( 10.62256650593128349, 126.1357510980948575, -0.2607537273017399571 ) ) ;
#8138 = ORIENTED_EDGE ( 'NONE', *, *, #18745, .T. ) ;
#8139 = CARTESIAN_POINT ( 'NONE',  ( 3.221735024265227398, -14.36526069886394730, 2.718910799868354378 ) ) ;
#8140 =( BOUNDED_SURFACE ( )  B_SPLINE_SURFACE ( 3, 2, ( 
 ( #16191, #41800, #18763 ),
 ( #9607, #18979, #15780 ),
 ( #9400, #6422, #22364 ),
 ( #35389, #6219, #29196 ) ),
 .UNSPECIFIED., .F., .F., .F. ) 
 B_SPLINE_SURFACE_WITH_KNOTS ( ( 4, 4 ),
 ( 3, 3 ),
 ( 0.001248665271192764357, 0.001438387644263458293 ),
 ( 0.000000000000000000, 0.2793900051564218168 ),
 .UNSPECIFIED. ) 
 GEOMETRIC_REPRESENTATION_ITEM ( )  RATIONAL_B_SPLINE_SURFACE ( (
 ( 1.000000000000000000, 0.9330598963482298336, 0.9035245845053385683),
 ( 1.000000000000000000, 0.9330598627208536167, 0.9035245360408918902),
 ( 1.000000000000000000, 0.9330598214100492838, 0.9035244765029348812),
 ( 1.000000000000000000, 0.9330598214935086343, 0.9035244766232181091) ) ) 
 REPRESENTATION_ITEM ( '' )  SURFACE ( )  );
#8141 = CARTESIAN_POINT ( 'NONE',  ( -4.801647862234980302, 117.4032733357427105, 1.015449305853463491 ) ) ;
#8142 = CARTESIAN_POINT ( 'NONE',  ( -56.62423581747135160, 3.520748359633372182, 2.300294558594641714 ) ) ;
#8143 = ADVANCED_FACE ( 'NONE', ( #17607 ), #34940, .T. ) ;
#8144 = CARTESIAN_POINT ( 'NONE',  ( 3.440871586586784936, -6.993729544307834445, 3.087053954803492761 ) ) ;
#8145 = CARTESIAN_POINT ( 'NONE',  ( 0.7897433827103791382, 156.7682548876429109, 1.239156740209750529 ) ) ;
#8146 = CARTESIAN_POINT ( 'NONE',  ( -0.9149567752697743694, 32.47697140010484418, 3.785418454572508473 ) ) ;
#8147 = CARTESIAN_POINT ( 'NONE',  ( -7.426015305410983203, 123.6670498955208473, -0.1137005639190685757 ) ) ;
#8148 = CARTESIAN_POINT ( 'NONE',  ( 4.440015753948663324, -2.305524871907271400, 1.325333094644747245 ) ) ;
#8149 = CARTESIAN_POINT ( 'NONE',  ( 9.144532176012500457, 124.1724329610943300, 0.2170005234668581362 ) ) ;
#8150 = CARTESIAN_POINT ( 'NONE',  ( -46.95911617132934879, 24.98948415085533270, 1.986615011824473864 ) ) ;
#8151 = CIRCLE ( 'NONE', #4081, 8.794749999999993406 ) ;
#8152 = CIRCLE ( 'NONE', #41493, 12.69999999999999751 ) ;
#8153 = CARTESIAN_POINT ( 'NONE',  ( -58.02159823468433331, 0.4660483771539991604, -0.8824573672536869529 ) ) ;
#8154 = CARTESIAN_POINT ( 'NONE',  ( -2.153153780027678099, 116.6795619169676712, -0.4673014195697471340 ) ) ;
#8155 = CARTESIAN_POINT ( 'NONE',  ( -13.85159022459153988, 16.50999999999999801, -5.016499999999999737 ) ) ;
#8156 = CARTESIAN_POINT ( 'NONE',  ( -31.59722765895411101, 71.22255575826451945, -1.270000000000008233 ) ) ;
#8157 = CARTESIAN_POINT ( 'NONE',  ( -1.454323051397943489, 106.2083702520809396, 5.134232663482987569 ) ) ;
#8158 = DIRECTION ( 'NONE',  ( 5.188838149069472160E-16, -1.699382548006136559E-16, -1.000000000000000000 ) ) ;
#8159 = CARTESIAN_POINT ( 'NONE',  ( 7.178138493693461797, 8.485180552427815215, -4.444891729080387321 ) ) ;
#8160 = CARTESIAN_POINT ( 'NONE',  ( -46.59067040677711447, 25.67275826535883709, 1.583530073016286899 ) ) ;
#8161 = DIRECTION ( 'NONE',  ( -0.8745520943968240202, 0.4849315768086551737, -5.361993529360572958E-16 ) ) ;
#8162 = CARTESIAN_POINT ( 'NONE',  ( 1.979187190576821465, -15.21425526833739639, 5.301287498526151332 ) ) ;
#8163 = ADVANCED_FACE ( 'NONE', ( #34442 ), #24481, .F. ) ;
#8164 = CARTESIAN_POINT ( 'NONE',  ( 0.07157677169882613322, 110.3683645023726569, -3.581994345755985076 ) ) ;
#8165 = CARTESIAN_POINT ( 'NONE',  ( -22.47739742037834176, 150.5824416163731314, 0.2728482117335696566 ) ) ;
#8166 = ORIENTED_EDGE ( 'NONE', *, *, #34061, .T. ) ;
#8167 = CYLINDRICAL_SURFACE ( 'NONE', #1882, 0.2539999999999986158 ) ;
#8168 = ADVANCED_FACE ( 'NONE', ( #9090, #42109 ), #32507, .F. ) ;
#8169 = EDGE_LOOP ( 'NONE', ( #23862, #23704, #7339, #19890 ) ) ;
#8170 = CARTESIAN_POINT ( 'NONE',  ( -46.78477525497644507, 20.40172935491330719, -4.969468548368532801 ) ) ;
#8171 = CARTESIAN_POINT ( 'NONE',  ( -3.758730197597831779, 121.0943292417197199, -0.07510837462871987336 ) ) ;
#8172 = CARTESIAN_POINT ( 'NONE',  ( 5.915669078949217230, -14.48123931593440972, 2.327441804047190033 ) ) ;
#8173 = CARTESIAN_POINT ( 'NONE',  ( -18.49784594330485987, 151.8926627062091086, 1.576652458532301182 ) ) ;
#8174 = EDGE_CURVE ( 'NONE', #22720, #16450, #12904, .T. ) ;
#8175 = CARTESIAN_POINT ( 'NONE',  ( 8.071933480009564121, 118.1206512225135015, -0.6391883341457641476 ) ) ;
#8176 = CARTESIAN_POINT ( 'NONE',  ( -3.366035089439492811, 13.68705809737886447, 3.178168622443589886 ) ) ;
#8177 = CARTESIAN_POINT ( 'NONE',  ( -23.25077945365681487, 149.0206351951634076, -0.9193108337986202194 ) ) ;
#8178 = CARTESIAN_POINT ( 'NONE',  ( -49.52577634351906966, 17.04162928648567288, -5.022404464390935352 ) ) ;
#8179 = ORIENTED_EDGE ( 'NONE', *, *, #15810, .T. ) ;
#8180 = CYLINDRICAL_SURFACE ( 'NONE', #27485, 0.6350000000000014522 ) ;
#8181 = CARTESIAN_POINT ( 'NONE',  ( -17.49548072478915728, 148.2779598588913643, 1.530134328283176526 ) ) ;
#8182 = CARTESIAN_POINT ( 'NONE',  ( -56.47502814425232742, 3.765754792631150760, -2.169991423106563566 ) ) ;
#8183 = CARTESIAN_POINT ( 'NONE',  ( 15.27645447632537490, 153.0676604005411434, -1.747501773188613772 ) ) ;
#8184 = CARTESIAN_POINT ( 'NONE',  ( -9.146501239663658467, 119.1751624949753534, -1.313831160619747251 ) ) ;
#8185 = CARTESIAN_POINT ( 'NONE',  ( -41.88683177698051452, 22.33947639032530219, -1.656270940288501636 ) ) ;
#8186 = CARTESIAN_POINT ( 'NONE',  ( 15.20409169301239949, 148.9716719698033387, -0.7946991634813624916 ) ) ;
#8187 = ORIENTED_EDGE ( 'NONE', *, *, #7169, .T. ) ;
#8188 = CARTESIAN_POINT ( 'NONE',  ( -13.34752792037781788, 125.8771108566470502, -1.915935069336977659 ) ) ;
#8189 = CARTESIAN_POINT ( 'NONE',  ( 3.893829680932177517, -15.58178733528788129, 3.041689768969074503 ) ) ;
#8190 = CARTESIAN_POINT ( 'NONE',  ( -4.381356941451189257, 118.1833196942565394, -0.5842306280113004346 ) ) ;
#8191 = CARTESIAN_POINT ( 'NONE',  ( -58.37934292759150168, 0.9822739792931106662, -1.208960021102219340 ) ) ;
#8192 = CARTESIAN_POINT ( 'NONE',  ( -5.003023251195230614, 117.4023580318003184, 0.8028984813139020682 ) ) ;
#8193 = CARTESIAN_POINT ( 'NONE',  ( 0.5133504486496096586, 119.5442839488369628, 0.5494766105906194742 ) ) ;
#8194 = CARTESIAN_POINT ( 'NONE',  ( -6.651972016613293606E-14, 104.1064662015457287, 7.011588703784780528E-31 ) ) ;
#8195 = CARTESIAN_POINT ( 'NONE',  ( 15.19466275752361462, 156.0906695176550443, 0.2814020119901242678 ) ) ;
#8196 = CARTESIAN_POINT ( 'NONE',  ( 2.951631207686332470, -3.807527625098089175, 7.891363245966695139 ) ) ;
#8197 = CARTESIAN_POINT ( 'NONE',  ( 8.672603809708727240, 123.3259068333282755, 0.4768435845110675642 ) ) ;
#8198 = CARTESIAN_POINT ( 'NONE',  ( 4.801257864230994876, 117.4019737406461843, -1.015743596227263179 ) ) ;
#8199 = EDGE_CURVE ( 'NONE', #11267, #1003, #40388, .T. ) ;
#8200 = CARTESIAN_POINT ( 'NONE',  ( -41.40170217118274110, 22.71997040916441080, -0.2118088196526931866 ) ) ;
#8201 = CARTESIAN_POINT ( 'NONE',  ( -4.812480952929572453, 117.4093055390909797, -1.196567565725688231 ) ) ;
#8202 = CIRCLE ( 'NONE', #34074, 0.2540000000000010583 ) ;
#8203 = CARTESIAN_POINT ( 'NONE',  ( -8.539387426415398608, 74.43734692935288422, -1.269999999999996909 ) ) ;
#8204 = CARTESIAN_POINT ( 'NONE',  ( -58.37241122568488549, -0.2962816677227891882, -1.032426590602281809E-14 ) ) ;
#8205 = CARTESIAN_POINT ( 'NONE',  ( -53.84631020977099780, 15.55534180641097386, 0.3033304672099269017 ) ) ;
#8206 = CARTESIAN_POINT ( 'NONE',  ( -3.292377373361788262, 159.4686222989141697, 0.02724393823342696752 ) ) ;
#8207 = ORIENTED_EDGE ( 'NONE', *, *, #3230, .F. ) ;
#8208 = CARTESIAN_POINT ( 'NONE',  ( -47.91671457320775573, 24.98613645765719582, -0.3547230740385284853 ) ) ;
#8209 = CARTESIAN_POINT ( 'NONE',  ( 6.905879605078832917, 121.7555842300460682, -0.3103901444470414939 ) ) ;
#8210 = CARTESIAN_POINT ( 'NONE',  ( -20.83467972660109169, 65.95194780259438971, 5.016499999999999737 ) ) ;
#8211 = CARTESIAN_POINT ( 'NONE',  ( 0.1363104457296995253, 115.6909491485452719, -1.761380027197414266 ) ) ;
#8212 = CARTESIAN_POINT ( 'NONE',  ( -0.6270554149911886643, 120.8998192842950488, -0.1385313962210437677 ) ) ;
#8213 = CARTESIAN_POINT ( 'NONE',  ( 4.431203275146504694, -13.68733396499126265, 3.949578922469492603 ) ) ;
#8214 = CARTESIAN_POINT ( 'NONE',  ( -7.282534483022796934, 158.3006260280594404, 1.262407574188499249 ) ) ;
#8215 = CARTESIAN_POINT ( 'NONE',  ( -6.758592445694407663E-14, 130.0144662015457300, 5.650815781856659706E-18 ) ) ;
#8216 = CARTESIAN_POINT ( 'NONE',  ( 11.70340384973333059, 118.7242475115495495, 0.3301557443347883924 ) ) ;
#8217 = ADVANCED_FACE ( 'NONE', ( #39113 ), #38340, .T. ) ;
#8218 = CARTESIAN_POINT ( 'NONE',  ( 5.950997316710809670, 155.3987497974532062, 0.1711121705728039510 ) ) ;
#8219 = DIRECTION ( 'NONE',  ( -0.8745520943968240202, 0.4849315768086553402, -5.361993529360572958E-16 ) ) ;
#8220 = CARTESIAN_POINT ( 'NONE',  ( -0.8313783143457759151, 22.10655722792919065, -0.5139362334944024280 ) ) ;
#8221 = CARTESIAN_POINT ( 'NONE',  ( -17.29877781292331562, 122.7677429521249053, -0.3633837628929260100 ) ) ;
#8222 = CYLINDRICAL_SURFACE ( 'NONE', #19441, 5.588000000000006295 ) ;
#8223 = ORIENTED_EDGE ( 'NONE', *, *, #15865, .T. ) ;
#8224 = CARTESIAN_POINT ( 'NONE',  ( 5.177913976931212581, 57.15000000000004832, -5.372100000000001430 ) ) ;
#8225 = ADVANCED_FACE ( 'NONE', ( #6521 ), #25420, .F. ) ;
#8226 = ORIENTED_EDGE ( 'NONE', *, *, #21855, .T. ) ;
#8227 = CARTESIAN_POINT ( 'NONE',  ( -6.041875895422170295, 118.7642705874486637, 0.9760351844723705872 ) ) ;
#8228 = LINE ( 'NONE', #5262, #35447 ) ;
#8229 = CARTESIAN_POINT ( 'NONE',  ( 19.40029886644210322, 131.9512773411433670, 1.949052778313794088 ) ) ;
#8230 = CARTESIAN_POINT ( 'NONE',  ( -58.47668496617176004, -0.4796687618251362917, -0.2989310191338567235 ) ) ;
#8231 = CARTESIAN_POINT ( 'NONE',  ( 20.30545318303836311, 145.4934252350392114, -1.680122328351855598 ) ) ;
#8232 = CARTESIAN_POINT ( 'NONE',  ( -6.895871986696200828, 19.14539577913392066, 4.887076909655228896 ) ) ;
#8233 = CARTESIAN_POINT ( 'NONE',  ( -2.920589480036270835, 117.1197906563906344, -0.5561477985301582772 ) ) ;
#8234 = CARTESIAN_POINT ( 'NONE',  ( 4.785785881226994221, 117.6676823434926149, -0.9347408560558295720 ) ) ;
#8235 = AXIS2_PLACEMENT_3D ( 'NONE', #32235, #35430, #38426 ) ;
#8236 = ORIENTED_EDGE ( 'NONE', *, *, #11582, .T. ) ;
#8237 = CARTESIAN_POINT ( 'NONE',  ( -7.051595240896901373, 122.0586610246435129, -0.007850877590933749012 ) ) ;
#8238 = CARTESIAN_POINT ( 'NONE',  ( 5.861737433447875567, -14.68024823731529871, 2.247769314782747774 ) ) ;
#8239 = AXIS2_PLACEMENT_3D ( 'NONE', #31929, #28096, #28726 ) ;
#8240 = CARTESIAN_POINT ( 'NONE',  ( 13.17422243436029916, 17.14500000000093394, -5.016499999999999737 ) ) ;
#8241 = CARTESIAN_POINT ( 'NONE',  ( -4.785365374205540867, 117.3993836135881708, -1.202560736569652677 ) ) ;
#8242 = EDGE_LOOP ( 'NONE', ( #4669, #25772, #18551, #39628, #10050, #25815, #27622, #31026, #10615, #14845 ) ) ;
#8243 = CARTESIAN_POINT ( 'NONE',  ( 0.4763900686812377883, 119.0154928070276412, 0.6070730232697147954 ) ) ;
#8244 = DIRECTION ( 'NONE',  ( -5.188838149069472160E-16, 1.699382548006136559E-16, 1.000000000000000000 ) ) ;
#8245 = CARTESIAN_POINT ( 'NONE',  ( 4.610436209567292387, 117.9340757871244847, 0.9619774773656434297 ) ) ;
#8246 = CARTESIAN_POINT ( 'NONE',  ( -0.7593927098684029042, 117.6736730875354766, 1.153084249965024455 ) ) ;
#8247 = CARTESIAN_POINT ( 'NONE',  ( -8.389224625646681588, -1.175411479303250628, -1.011143247504549869 ) ) ;
#8248 = CARTESIAN_POINT ( 'NONE',  ( 8.969937932052559404, 123.1852847016406685, 0.8267063328025513469 ) ) ;
#8249 = CARTESIAN_POINT ( 'NONE',  ( 14.73199999999999754, 61.59499999999999886, -1.904999999999999583 ) ) ;
#8250 = CARTESIAN_POINT ( 'NONE',  ( 23.13757068712586573, 148.9583646262859133, -0.2674444443938934768 ) ) ;
#8251 = CARTESIAN_POINT ( 'NONE',  ( -17.64290547347870941, 83.78857423953914463, 1.523999999999996247 ) ) ;
#8252 = CARTESIAN_POINT ( 'NONE',  ( -58.36745437842773754, -0.2866796535172885796, 0.05885235802170251523 ) ) ;
#8253 = CARTESIAN_POINT ( 'NONE',  ( -30.60466991270287807, 55.37784481733978481, -1.524000000000004462 ) ) ;
#8254 = AXIS2_PLACEMENT_3D ( 'NONE', #33501, #7514, #20264 ) ;
#8255 = CARTESIAN_POINT ( 'NONE',  ( -55.83113473690871587, 5.632394305663344092, 2.901290885506219386 ) ) ;
#8256 = DIRECTION ( 'NONE',  ( 0.9998004120163608288, 0.000000000000000000, 0.01997839162482749342 ) ) ;
#8257 = CARTESIAN_POINT ( 'NONE',  ( -4.317796372703391228, 118.2120857186201732, 0.3236837648097654063 ) ) ;
#8258 = CARTESIAN_POINT ( 'NONE',  ( 0.1066086480733247077, 105.8844037013956410, -5.332931792593717191 ) ) ;
#8259 = ORIENTED_EDGE ( 'NONE', *, *, #35338, .F. ) ;
#8260 = CARTESIAN_POINT ( 'NONE',  ( -53.68435271313694557, 11.12367579685427721, 3.945100831076007619 ) ) ;
#8261 = ADVANCED_FACE ( 'NONE', ( #38901 ), #41473, .F. ) ;
#8262 = CARTESIAN_POINT ( 'NONE',  ( -4.138294784885184541, 119.2769814663382419, -0.9260517387791210586 ) ) ;
#8263 = CYLINDRICAL_SURFACE ( 'NONE', #11489, 0.5080000000000000071 ) ;
#8265 = CARTESIAN_POINT ( 'NONE',  ( 4.229037014694107199, 118.2245626801250182, 0.4851524337614830373 ) ) ;
#8264 = AXIS2_PLACEMENT_3D ( 'NONE', #40228, #11022, #23366 ) ;
#8266 = CARTESIAN_POINT ( 'NONE',  ( -10.85076598842381124, 126.1616406593870607, -0.8982697194533707519 ) ) ;
#8267 = CARTESIAN_POINT ( 'NONE',  ( 6.057513928997568797, 57.78500000000000369, -1.904999999999999805 ) ) ;
#8268 = CARTESIAN_POINT ( 'NONE',  ( 11.74288454345096788, 118.7273140689154616, 0.2346507796901761422 ) ) ;
#8269 = EDGE_CURVE ( 'NONE', #29132, #1824, #8415, .T. ) ;
#8270 = ORIENTED_EDGE ( 'NONE', *, *, #19599, .F. ) ;
#8271 = CARTESIAN_POINT ( 'NONE',  ( 4.300553167417687561, 27.50566818391071422, -1.719522505244270860 ) ) ;
#8272 = CARTESIAN_POINT ( 'NONE',  ( -10.10772093100563751, 154.1059161911440469, -1.650231108813019043 ) ) ;
#8273 = CARTESIAN_POINT ( 'NONE',  ( -6.422645615570758970, 77.88548590848095898, -1.523999999999996469 ) ) ;
#8274 = CARTESIAN_POINT ( 'NONE',  ( -0.1064799869812408512, 105.7853621660184444, 5.332934571178566507 ) ) ;
#8275 = DIRECTION ( 'NONE',  ( -0.8745520943968249084, 0.4849315768086536194, -5.575199987069925217E-16 ) ) ;
#8276 = CARTESIAN_POINT ( 'NONE',  ( 6.070556577249959673, 121.4252507025452559, 0.3080570883581159047 ) ) ;
#8277 = CARTESIAN_POINT ( 'NONE',  ( -5.861642722916909243, 64.54502714855203749, -1.523999999999993804 ) ) ;
#8278 = CARTESIAN_POINT ( 'NONE',  ( 0.3408176794664849463, 116.9919054422455531, 0.3412737040790792542 ) ) ;
#8279 = DIRECTION ( 'NONE',  ( 0.9998004120163608288, 0.000000000000000000, 0.01997839162482736852 ) ) ;
#8281 = CARTESIAN_POINT ( 'NONE',  ( 18.85079593648338658, 152.0234722879370111, -1.474728064877437017 ) ) ;
#8280 = CARTESIAN_POINT ( 'NONE',  ( 1.822811606207361823, -15.29362660170947841, 5.402418844745947801 ) ) ;
#8282 = CARTESIAN_POINT ( 'NONE',  ( -1.325863631979564472, 119.1766673560425858, 0.6173222594915838135 ) ) ;
#8283 = TOROIDAL_SURFACE ( 'NONE', #11680, 0.3810000000000014486, 0.2540000000000000036 ) ;
#8284 = CARTESIAN_POINT ( 'NONE',  ( 0.7467592606654794851, -15.18718160513664195, -0.6397234560659120772 ) ) ;
#8285 = CARTESIAN_POINT ( 'NONE',  ( -16.63860074592949445, 155.2617138006751532, -0.9902706816744289986 ) ) ;
#8286 = CARTESIAN_POINT ( 'NONE',  ( 0.9436776830090995993, 12.87300645547595046, -0.2395577073833762005 ) ) ;
#8287 = ORIENTED_EDGE ( 'NONE', *, *, #11633, .T. ) ;
#8288 = CARTESIAN_POINT ( 'NONE',  ( -48.25086062633821626, 17.91646674446130305, 3.976701633436060757 ) ) ;
#8289 = CARTESIAN_POINT ( 'NONE',  ( -12.39727431377436062, 130.6617397222824479, 0.4182072254281061219 ) ) ;
#8290 = CARTESIAN_POINT ( 'NONE',  ( 4.778253948640466042, -14.19231145175180231, 4.234097743872750286 ) ) ;
#8291 = CARTESIAN_POINT ( 'NONE',  ( 6.570524231283992656, 120.8223817900871495, -0.7604033795411312413 ) ) ;
#8292 = ORIENTED_EDGE ( 'NONE', *, *, #42104, .T. ) ;
#8293 = CIRCLE ( 'NONE', #31395, 2.540000000000000480 ) ;
#8294 = CARTESIAN_POINT ( 'NONE',  ( 1.665672165190749565, 115.7029491485453434, 1.727344103749859583 ) ) ;
#8295 = AXIS2_PLACEMENT_3D ( 'NONE', #8680, #32262, #21644 ) ;
#8296 = ORIENTED_EDGE ( 'NONE', *, *, #37593, .F. ) ;
#8297 = CARTESIAN_POINT ( 'NONE',  ( 2.376025398756717699, -14.92724974027714779, 5.073178661078445728 ) ) ;
#8298 = CARTESIAN_POINT ( 'NONE',  ( -4.854266779389924125, 117.7484759862343964, -0.9334171246494462615 ) ) ;
#8299 = CARTESIAN_POINT ( 'NONE',  ( 14.68196552533998123, 148.8424012017631242, 0.1663232928928552179 ) ) ;
#8300 = ORIENTED_EDGE ( 'NONE', *, *, #13123, .T. ) ;
#8301 = CARTESIAN_POINT ( 'NONE',  ( 1.175363150376307564, 118.2527139659984101, 0.6673024542226162481 ) ) ;
#8302 = CARTESIAN_POINT ( 'NONE',  ( -6.654617103318593247E-14, 104.6144662015457243, 1.534725424433578570E-31 ) ) ;
#8303 = DIRECTION ( 'NONE',  ( 0.8745520943968235761, -0.4849315768086558398, 0.000000000000000000 ) ) ;
#8304 = CARTESIAN_POINT ( 'NONE',  ( 0.0008202526017135117458, 159.6052337359418800, -0.04104879434819952433 ) ) ;
#8305 = CARTESIAN_POINT ( 'NONE',  ( 0.9174821693851576976, 116.5216256635990391, -0.1124321123350597307 ) ) ;
#8306 = DIRECTION ( 'NONE',  ( -0.8745520943968235761, 0.4849315768086558953, -5.361993529360570985E-16 ) ) ;
#8307 = CARTESIAN_POINT ( 'NONE',  ( 1.731823037650620289, -15.42244943691900616, 5.436280266706707387 ) ) ;
#8308 = CARTESIAN_POINT ( 'NONE',  ( 10.63219908769094069, 56.50600268266111215, 5.016499999999999737 ) ) ;
#8309 = DIRECTION ( 'NONE',  ( -0.9998004120163608288, 0.000000000000000000, -0.01997839162482749342 ) ) ;
#8310 = CARTESIAN_POINT ( 'NONE',  ( -4.672965529255816541, 117.9840894666471058, 0.6969538851604538676 ) ) ;
#8311 = ORIENTED_EDGE ( 'NONE', *, *, #14937, .T. ) ;
#8312 = CARTESIAN_POINT ( 'NONE',  ( -23.97640303682767993, 76.49434496853974963, -1.270000000000005347 ) ) ;
#8313 = CARTESIAN_POINT ( 'NONE',  ( -2.936339730833952277, 118.0886593047229667, -0.8676653305777561886 ) ) ;
#8314 = CARTESIAN_POINT ( 'NONE',  ( -4.551180572033598715, 124.4408722044843927, -0.1097773164883771579 ) ) ;
#8316 = CARTESIAN_POINT ( 'NONE',  ( 4.806277061065945766, 117.4760889790769909, 1.179883221431397455 ) ) ;
#8315 = B_SPLINE_CURVE_WITH_KNOTS ( 'NONE', 3,
 ( #19356, #9165, #2785, #12560 ),
 .UNSPECIFIED., .F., .F.,
 ( 4, 4 ),
 ( 0.000000000000000000, 0.9566564897266378598 ),
 .UNSPECIFIED. ) ;
#8317 = CARTESIAN_POINT ( 'NONE',  ( -11.25890006629606610, 56.90956307411701687, -5.016499999999999737 ) ) ;
#8318 = CARTESIAN_POINT ( 'NONE',  ( -0.1065646865916158176, 105.8844662015456919, 5.332932678536313809 ) ) ;
#8319 = AXIS2_PLACEMENT_3D ( 'NONE', #18104, #38141, #15746 ) ;
#8320 = CARTESIAN_POINT ( 'NONE',  ( -3.416230376366909294, -5.529048218071860532, 3.121479803864907865 ) ) ;
#8321 = CARTESIAN_POINT ( 'NONE',  ( -48.56815661899839398, 19.24492339269599839, 5.224590812749970503 ) ) ;
#8322 = DIRECTION ( 'NONE',  ( 1.000000000000000000, 0.000000000000000000, 0.000000000000000000 ) ) ;
#8323 = CARTESIAN_POINT ( 'NONE',  ( 3.416089938271958726, -12.71546774565127080, 1.400931973480754822 ) ) ;
#8324 = CARTESIAN_POINT ( 'NONE',  ( 0.6941271473898690259, 106.1608668108878817, -5.200699783222979988 ) ) ;
#8325 = EDGE_CURVE ( 'NONE', #31622, #24097, #15185, .T. ) ;
#8326 = CARTESIAN_POINT ( 'NONE',  ( -3.216045294022573220, 29.79186273158684983, 3.430717191674401700 ) ) ;
#8327 = CARTESIAN_POINT ( 'NONE',  ( -0.3155423528362975016, 115.7029491485453718, 1.753374870527287355 ) ) ;
#8328 = CARTESIAN_POINT ( 'NONE',  ( -3.685501180670149424, 30.72893705507438611, -2.802369389919810772 ) ) ;
#8329 = ORIENTED_EDGE ( 'NONE', *, *, #34821, .F. ) ;
#8330 = CARTESIAN_POINT ( 'NONE',  ( -5.339818517979998624, 105.1224975962397110, -0.2412077680896454468 ) ) ;
#8331 = CARTESIAN_POINT ( 'NONE',  ( 4.008975597637738808, -15.55340266690961926, 2.658432704422428738 ) ) ;
#8332 = CARTESIAN_POINT ( 'NONE',  ( -1.119065284002324745, 158.2739225783580537, 1.587016747512054238 ) ) ;
#8333 = CARTESIAN_POINT ( 'NONE',  ( 0.7290388503741822568, 0.07276798020498101427, -0.6497956273326017662 ) ) ;
#8334 = CARTESIAN_POINT ( 'NONE',  ( -0.009113691291695666039, 25.33460033795575583, 0.9756159547818916700 ) ) ;
#8335 = ORIENTED_EDGE ( 'NONE', *, *, #18832, .T. ) ;
#8336 = AXIS2_PLACEMENT_3D ( 'NONE', #28372, #18982, #38179 ) ;
#8337 = ORIENTED_EDGE ( 'NONE', *, *, #2384, .T. ) ;
#8338 = LINE ( 'NONE', #38781, #35787 ) ;
#8339 = CARTESIAN_POINT ( 'NONE',  ( 1.881281939329280117, 113.2583846565721757, 2.513576850050686318 ) ) ;
#8340 = CARTESIAN_POINT ( 'NONE',  ( -5.880513813086854391, 121.0368588677253143, 0.5043468530174899378 ) ) ;
#8341 = CARTESIAN_POINT ( 'NONE',  ( -42.82337740149211669, 22.05454911558773645, 2.000910913296384930 ) ) ;
#8342 = CARTESIAN_POINT ( 'NONE',  ( 4.610465475190451912, 118.0209586553088172, -0.6829666416481755542 ) ) ;
#8343 = CARTESIAN_POINT ( 'NONE',  ( 7.441788261791815628, 120.6159063994810055, -0.9748553081951374377 ) ) ;
#8344 = CARTESIAN_POINT ( 'NONE',  ( -16.37183938475186906, 128.5611466799914240, -2.176631273311136372 ) ) ;
#8345 = DIRECTION ( 'NONE',  ( -5.188838149069471174E-16, 1.699382548006136313E-16, 1.000000000000000000 ) ) ;
#8346 = CARTESIAN_POINT ( 'NONE',  ( -0.02244247360070322078, 39.09286639261657115, 1.286999615499953231 ) ) ;
#8347 = CARTESIAN_POINT ( 'NONE',  ( 7.078188358610526087, 121.9740017686541194, -0.1969649471280497111 ) ) ;
#8348 = ORIENTED_EDGE ( 'NONE', *, *, #10985, .F. ) ;
#8349 = CARTESIAN_POINT ( 'NONE',  ( 3.117629155811438402, -14.23119940253145188, 1.544136867890079090 ) ) ;
#8350 = CARTESIAN_POINT ( 'NONE',  ( 11.58677707360137532, 55.24500000000000455, -4.474811398758259173 ) ) ;
#8351 = TOROIDAL_SURFACE ( 'NONE', #19229, 3.683000000000000718, 0.5080000000000000071 ) ;
#8352 = B_SPLINE_CURVE_WITH_KNOTS ( 'NONE', 3,
 ( #10506, #29891, #14114, #26266, #36924, #20709, #40125, #36088, #10082, #4353, #23476, #729, #19871, #13706, #7322, #20281, #17314, #20492 ),
 .UNSPECIFIED., .F., .F.,
 ( 4, 2, 2, 2, 2, 2, 2, 2, 4 ),
 ( 0.000000000000000000, 0.0008271500248385261133, 0.001654300049677052227, 0.003308600099354083203, 0.004135750124192599450, 0.004962900149031114830, 0.006617200198708181151, 0.009925800298062312926, 0.01323440039741644383 ),
 .UNSPECIFIED. ) ;
#8353 = CARTESIAN_POINT ( 'NONE',  ( -57.94306413390888366, 1.184802614102420382, 1.419326152558788134 ) ) ;
#8354 = CARTESIAN_POINT ( 'NONE',  ( -3.522755225739859775, -9.592572062075928940, 3.019445982675781348 ) ) ;
#8355 = CARTESIAN_POINT ( 'NONE',  ( 16.72040787068447187, 146.6545634508490821, 1.779279871595184082 ) ) ;
#8356 = CARTESIAN_POINT ( 'NONE',  ( 0.9447929531305513384, 34.22797915461067930, 2.226895425005813056 ) ) ;
#8357 = CARTESIAN_POINT ( 'NONE',  ( -4.842864477130262912, 117.0601473006971105, 0.7870117353683143691 ) ) ;
#8358 = CIRCLE ( 'NONE', #11094, 0.6350000000000014522 ) ;
#8359 = CARTESIAN_POINT ( 'NONE',  ( -3.974385726840726107, -7.478117039488521023, -2.359557994316856533 ) ) ;
#8360 = CARTESIAN_POINT ( 'NONE',  ( 1.569753016146328228, 156.2570369995211479, 0.1094014671735940580 ) ) ;
#8361 = EDGE_CURVE ( 'NONE', #2275, #13951, #19496, .T. ) ;
#8362 = CARTESIAN_POINT ( 'NONE',  ( 8.423846519715326053, 3.801276092563157682, 0.04266398729441032295 ) ) ;
#8363 = CARTESIAN_POINT ( 'NONE',  ( -57.78284603921808582, 0.8603191986865516006, -0.5272538806337706552 ) ) ;
#8364 = CARTESIAN_POINT ( 'NONE',  ( 8.771996676116902592, 117.8544088467123458, -0.2656499505225238256 ) ) ;
#8365 = CARTESIAN_POINT ( 'NONE',  ( -10.34239276132902319, 65.15305678602257444, -1.269999999999996243 ) ) ;
#8366 = CARTESIAN_POINT ( 'NONE',  ( -6.059261036834476144, 57.14999999999999858, -5.016499999999999737 ) ) ;
#8367 = CARTESIAN_POINT ( 'NONE',  ( 1.834459164715509960, -15.41678468052755946, 5.387059099755639124 ) ) ;
#8368 = CARTESIAN_POINT ( 'NONE',  ( -17.08598887363762131, 83.79821757228496892, -1.270000000000002904 ) ) ;
#8369 = CARTESIAN_POINT ( 'NONE',  ( 2.068261358883969780, 0.06400946394871305511, -8.190863557276260920 ) ) ;
#8370 = CARTESIAN_POINT ( 'NONE',  ( 1.960761714621917395, 117.3993839177211242, 1.450045767418920883 ) ) ;
#8371 = DIRECTION ( 'NONE',  ( 0.9998004120163608288, 5.205824365704082573E-17, 0.01997839162482749342 ) ) ;
#8372 = CARTESIAN_POINT ( 'NONE',  ( 2.671714809844681238, -14.97371442308345380, 4.574436322856921144 ) ) ;
#8373 = EDGE_CURVE ( 'NONE', #1213, #5065, #42155, .T. ) ;
#8374 = CARTESIAN_POINT ( 'NONE',  ( 0.3585272760097797384, 113.0327356262573915, -2.615547676125327570 ) ) ;
#8375 = CARTESIAN_POINT ( 'NONE',  ( -22.54544115201725063, 150.6069110094195764, 0.1392563518891846153 ) ) ;
#8376 = ORIENTED_EDGE ( 'NONE', *, *, #17204, .F. ) ;
#8377 = CARTESIAN_POINT ( 'NONE',  ( -6.540718711769984318E-14, 75.78546620154573077, -7.235675496349066572E-18 ) ) ;
#8378 = ORIENTED_EDGE ( 'NONE', *, *, #37282, .F. ) ;
#8379 = CARTESIAN_POINT ( 'NONE',  ( -47.84756666395252722, 19.38928433903621240, -5.209054514891962917 ) ) ;
#8380 = CIRCLE ( 'NONE', #18583, 0.2539999999999986158 ) ;
#8381 = CARTESIAN_POINT ( 'NONE',  ( -5.953848250812766807, 121.5461441479843216, -0.08186234018733787310 ) ) ;
#8382 = CARTESIAN_POINT ( 'NONE',  ( 5.416639188517969217, -15.16156180871851333, 2.817365454923381307 ) ) ;
#8383 = CARTESIAN_POINT ( 'NONE',  ( -4.917623111643208311, 158.3981005702974016, 1.478962986009813685 ) ) ;
#8384 = AXIS2_PLACEMENT_3D ( 'NONE', #36428, #10209, #38984 ) ;
#8385 = CARTESIAN_POINT ( 'NONE',  ( 22.19718911286642893, 149.5167998366165989, -0.9981983707184384214 ) ) ;
#8386 = CARTESIAN_POINT ( 'NONE',  ( -0.5093740622119584671, 14.76157059199007016, 4.595130897425484306 ) ) ;
#8387 = CARTESIAN_POINT ( 'NONE',  ( -5.807154922825684018, 117.0096406922080376, -0.3504623104576316539 ) ) ;
#8388 = CARTESIAN_POINT ( 'NONE',  ( -48.68735867619428603, 18.29031291928623659, -5.164865279787345997 ) ) ;
#8389 = EDGE_CURVE ( 'NONE', #33842, #13325, #33143, .T. ) ;
#8390 = ORIENTED_EDGE ( 'NONE', *, *, #31314, .T. ) ;
#8391 = CARTESIAN_POINT ( 'NONE',  ( 2.183572936211770177, 116.1951486486012470, 0.06351249239639800148 ) ) ;
#8392 = FACE_OUTER_BOUND ( 'NONE', #27755, .T. ) ;
#8393 = CARTESIAN_POINT ( 'NONE',  ( -0.8914275061361285335, 157.0053619834820324, 1.381823885352171599 ) ) ;
#8394 = CARTESIAN_POINT ( 'NONE',  ( -52.83837246138028831, 11.08843963240696517, -3.928308309794706688 ) ) ;
#8395 = CARTESIAN_POINT ( 'NONE',  ( 4.356286657365759929, 157.6046910967438066, -1.678189947947346994 ) ) ;
#8396 = CARTESIAN_POINT ( 'NONE',  ( -21.26307135201312093, 148.5140355411650717, -2.311892396764663626 ) ) ;
#8397 = CARTESIAN_POINT ( 'NONE',  ( -56.22331024217277928, 5.808995339285999648, -2.850545730341259798 ) ) ;
#8398 = VECTOR ( 'NONE', #6212, 1000.000000000000227 ) ;
#8399 = CARTESIAN_POINT ( 'NONE',  ( 14.98735845036247127, 139.3652335140928074, -0.8263902896301492662 ) ) ;
#8400 = EDGE_CURVE ( 'NONE', #19740, #9063, #8151, .T. ) ;
#8401 = ORIENTED_EDGE ( 'NONE', *, *, #34821, .T. ) ;
#8402 = CARTESIAN_POINT ( 'NONE',  ( -3.875499641586351629, 157.0187206368471209, -1.749001665105742731 ) ) ;
#8403 = CARTESIAN_POINT ( 'NONE',  ( 4.521904862512733381, -15.32733325190937990, -0.1948396341466702986 ) ) ;
#8404 = CARTESIAN_POINT ( 'NONE',  ( -4.397284644090289518, 118.1792272226432061, -0.5668491568854608920 ) ) ;
#8405 = EDGE_CURVE ( 'NONE', #1192, #30178, #11546, .T. ) ;
#8406 = CARTESIAN_POINT ( 'NONE',  ( -58.07447437077728125, 1.735896131820596766, -1.499107834811110429 ) ) ;
#8407 = CARTESIAN_POINT ( 'NONE',  ( -4.804336728621736441, 117.5395540501120877, 0.9846445990501094814 ) ) ;
#8408 = CARTESIAN_POINT ( 'NONE',  ( 12.92173176740947760, 125.9520529675768898, 1.821380522590920314 ) ) ;
#8409 = CARTESIAN_POINT ( 'NONE',  ( -17.14500000000466784, 71.11999999999886768, -1.524000000000000909 ) ) ;
#8410 = CIRCLE ( 'NONE', #945, 3.175000000000001155 ) ;
#8411 = EDGE_CURVE ( 'NONE', #18509, #33497, #35371, .T. ) ;
#8412 = CARTESIAN_POINT ( 'NONE',  ( -5.875566536072981627, -5.528788512802195854, 6.048791003748659634 ) ) ;
#8413 = CARTESIAN_POINT ( 'NONE',  ( 12.12200908156748547, 130.5412724693565849, 0.6534646642625604462 ) ) ;
#8414 = DIRECTION ( 'NONE',  ( -0.1906721105965055174, 0.9816537812491091808, 0.000000000000000000 ) ) ;
#8415 = CIRCLE ( 'NONE', #33577, 1.905000000000007354 ) ;
#8416 = CARTESIAN_POINT ( 'NONE',  ( -44.35420297070785978, 19.68308750433651966, -0.4327882352162440438 ) ) ;
#8417 = CARTESIAN_POINT ( 'NONE',  ( -1.627066591301449483, 117.3993836555909098, 1.397831962642635872 ) ) ;
#8418 = CARTESIAN_POINT ( 'NONE',  ( 6.057513928997551034, 86.35999999999998522, 1.904999999999996030 ) ) ;
#8419 = TOROIDAL_SURFACE ( 'NONE', #37018, 0.7620000000000000107, 0.2540000000000000036 ) ;
#8420 = CARTESIAN_POINT ( 'NONE',  ( -57.78284603921808582, 0.8603191986865516006, 0.5272538806337502271 ) ) ;
#8421 = CARTESIAN_POINT ( 'NONE',  ( -49.23607562092252721, 19.66429951101446960, 3.974467759520285082 ) ) ;
#8422 = CARTESIAN_POINT ( 'NONE',  ( -20.68286957925308656, 152.5754960671270055, -0.1900957434528338652 ) ) ;
#8423 = EDGE_LOOP ( 'NONE', ( #2573, #33924, #21553, #29564 ) ) ;
#8424 = CARTESIAN_POINT ( 'NONE',  ( -48.74997074597248314, 21.16799237019927205, -3.036721307642072265 ) ) ;
#8425 = CARTESIAN_POINT ( 'NONE',  ( -5.872192093296925819, 121.3219910589839685, -0.3926023243202280688 ) ) ;
#8426 = CARTESIAN_POINT ( 'NONE',  ( -8.107080057029742548, 121.1657703571620885, 0.9663533087783954256 ) ) ;
#8427 = CIRCLE ( 'NONE', #2339, 0.2540000000000018909 ) ;
#8428 = EDGE_LOOP ( 'NONE', ( #13331, #23123, #8963, #10492 ) ) ;
#8429 = CARTESIAN_POINT ( 'NONE',  ( 0.03519895179119666290, 115.7029491485446613, -1.761499482103947800 ) ) ;
#8430 = CARTESIAN_POINT ( 'NONE',  ( -5.276193270648819933, 121.3253820001177417, -0.2225082926070588163 ) ) ;
#8431 = CARTESIAN_POINT ( 'NONE',  ( 3.203739484688298500, -15.10556029324786032, 5.619401687775556375 ) ) ;
#8432 = CARTESIAN_POINT ( 'NONE',  ( -16.82967018813389970, 125.2521365416322254, 1.031881933595589995 ) ) ;
#8433 = CARTESIAN_POINT ( 'NONE',  ( 0.4298212797809583541, 117.3993833036163181, -1.480797141651997162 ) ) ;
#8434 = CARTESIAN_POINT ( 'NONE',  ( 15.48069746188175166, 120.7065362441885981, 0.4134764081404143088 ) ) ;
#8435 = CARTESIAN_POINT ( 'NONE',  ( 1.561582345843624431, 156.2588034088681184, 0.03120413162939523685 ) ) ;
#8436 = DIRECTION ( 'NONE',  ( 0.7071067811865479058, -0.7071067811865472397, 0.000000000000000000 ) ) ;
#8437 = CARTESIAN_POINT ( 'NONE',  ( -0.8918910426314872186, 22.31184809748591391, -0.3959014520797728975 ) ) ;
#8438 = CARTESIAN_POINT ( 'NONE',  ( -23.33940156856683856, 149.0646716566344026, -0.5435133253920597651 ) ) ;
#8439 = CARTESIAN_POINT ( 'NONE',  ( -41.05189575270519242, 23.09451173561982529, -1.269999999999997797 ) ) ;
#8440 = DIRECTION ( 'NONE',  ( -5.188838149069472160E-16, 1.699382548006136559E-16, 1.000000000000000000 ) ) ;
#8441 = VERTEX_POINT ( 'NONE', #26952 ) ;
#8442 = CARTESIAN_POINT ( 'NONE',  ( -4.116559577307818962, 118.3381180974515274, 0.8321499372237044501 ) ) ;
#8443 = CARTESIAN_POINT ( 'NONE',  ( -5.322367322403097845, 105.1224774134945790, 0.3643359423292727994 ) ) ;
#8444 = CARTESIAN_POINT ( 'NONE',  ( 14.08892660837130606, 121.3807765770047666, 1.491720297716245369 ) ) ;
#8445 = CARTESIAN_POINT ( 'NONE',  ( -47.84356795211455449, 19.38525671449502852, -5.197506975155119058 ) ) ;
#8446 = CARTESIAN_POINT ( 'NONE',  ( 16.05265579080195337, 153.3736753708079732, -1.680156470693514814 ) ) ;
#8447 = AXIS2_PLACEMENT_3D ( 'NONE', #34224, #11839, #38259 ) ;
#8448 = CARTESIAN_POINT ( 'NONE',  ( -1.404924415901314561, -12.60368214249519703, -4.422195601339041993 ) ) ;
#8449 = CARTESIAN_POINT ( 'NONE',  ( -14.92730792698330866, 121.5307057168427605, -1.330945954902034822 ) ) ;
#8450 = CARTESIAN_POINT ( 'NONE',  ( 4.877181834135257965, 117.6443843650974088, -0.8852099847017325107 ) ) ;
#8451 = CARTESIAN_POINT ( 'NONE',  ( 6.711594774621037374, 121.2247800624193133, 0.3423702293131484775 ) ) ;
#8452 = VERTEX_POINT ( 'NONE', #7166 ) ;
#8453 = EDGE_CURVE ( 'NONE', #9800, #29150, #13954, .T. ) ;
#8454 = CARTESIAN_POINT ( 'NONE',  ( -13.59948517815245772, 150.2262467139961473, -0.1464537565166197652 ) ) ;
#8455 = CARTESIAN_POINT ( 'NONE',  ( -13.13949684203677570, 123.8872625266795211, -1.904607404193280340 ) ) ;
#8456 = CARTESIAN_POINT ( 'NONE',  ( 2.291706021380962355, -15.53059561260056221, 5.887745402940570472 ) ) ;
#8457 = EDGE_CURVE ( 'NONE', #18705, #21597, #23768, .T. ) ;
#8458 = DIRECTION ( 'NONE',  ( -5.188838149069472160E-16, 1.699382548006136559E-16, 1.000000000000000000 ) ) ;
#8459 = CIRCLE ( 'NONE', #15918, 0.6349999999999977884 ) ;
#8460 = CARTESIAN_POINT ( 'NONE',  ( -3.903555647324534306, 118.1651005205136897, -0.7209690768601634270 ) ) ;
#8461 = VERTEX_POINT ( 'NONE', #775 ) ;
#8462 = CARTESIAN_POINT ( 'NONE',  ( 8.504430935371811273, 120.5511696877957775, 1.462663580662433294 ) ) ;
#8463 = CARTESIAN_POINT ( 'NONE',  ( -6.318938770521977055, 64.36956080246774548, -1.269999999999994023 ) ) ;
#8464 = EDGE_CURVE ( 'NONE', #3752, #32528, #576, .T. ) ;
#8465 = CARTESIAN_POINT ( 'NONE',  ( -3.844008814211067993, 118.0218828919481098, -0.9706315391978014295 ) ) ;
#8466 = B_SPLINE_CURVE_WITH_KNOTS ( 'NONE', 3,
 ( #14956, #35006, #6033, #21758 ),
 .UNSPECIFIED., .F., .F.,
 ( 4, 4 ),
 ( 9.335326988569945976E-17, 6.355780391037319497E-05 ),
 .UNSPECIFIED. ) ;
#8467 = CARTESIAN_POINT ( 'NONE',  ( -1.590100404673132184, 118.0223913815010377, 0.9765506547304494411 ) ) ;
#8468 = ADVANCED_FACE ( 'NONE', ( #36135 ), #18325, .T. ) ;
#8469 = CARTESIAN_POINT ( 'NONE',  ( -8.417729735924666556, -0.9468307554896212563, 0.2322036382352700989 ) ) ;
#8470 = CARTESIAN_POINT ( 'NONE',  ( 10.42685857375358260, 124.8149993102252182, 1.042337215157124186 ) ) ;
#8471 = CARTESIAN_POINT ( 'NONE',  ( -5.240921474315769046, 115.6909491485453003, -1.017345001637511404 ) ) ;
#8472 = CARTESIAN_POINT ( 'NONE',  ( 21.63859276624132377, 151.3813297165527274, -0.4067934712883240489 ) ) ;
#8473 = LINE ( 'NONE', #24637, #26739 ) ;
#8474 = CARTESIAN_POINT ( 'NONE',  ( -58.34697146883529228, -0.2437238978784766197, 0.1881573647123204462 ) ) ;
#8475 = CARTESIAN_POINT ( 'NONE',  ( 5.177913976931204587, 71.67999986514567468, 5.372100000000000541 ) ) ;
#8476 = CARTESIAN_POINT ( 'NONE',  ( -28.65049350906917880, 77.81814547195517662, -1.524000000000008015 ) ) ;
#8477 = CARTESIAN_POINT ( 'NONE',  ( -4.158717781106146205, 118.2391784042057026, 0.2328764324043287315 ) ) ;
#8478 = CARTESIAN_POINT ( 'NONE',  ( 14.73199999999999932, 12.96416000000000146, 0.000000000000000000 ) ) ;
#8479 = ORIENTED_EDGE ( 'NONE', *, *, #38421, .T. ) ;
#8480 = CARTESIAN_POINT ( 'NONE',  ( -49.19743978460682143, 17.65503563884207594, 5.190924102448284394 ) ) ;
#8481 = CARTESIAN_POINT ( 'NONE',  ( 8.322108986833429256, 120.1313932179692330, -1.118147983713804194 ) ) ;
#8482 = CARTESIAN_POINT ( 'NONE',  ( -0.1524052867847605630, 105.8811906981200934, -5.339394923009169958 ) ) ;
#8483 = CARTESIAN_POINT ( 'NONE',  ( 4.345256946659891817, 118.1827420971760887, 0.6195611995493047752 ) ) ;
#8484 = CARTESIAN_POINT ( 'NONE',  ( -9.732298487430798062, 124.2227999206177032, -0.8093454005834662679 ) ) ;
#8485 = CARTESIAN_POINT ( 'NONE',  ( 4.854908608518735846, 117.4053607954329976, -1.004341486598190558 ) ) ;
#8486 = CARTESIAN_POINT ( 'NONE',  ( -17.14499999999998892, 57.14999999999997726, -5.016499999999999737 ) ) ;
#8487 = EDGE_LOOP ( 'NONE', ( #39478, #10384, #17593, #18008, #36861 ) ) ;
#8488 = CARTESIAN_POINT ( 'NONE',  ( 0.2838385327444274964, 29.22985346960623332, -4.617364983570896086 ) ) ;
#8489 = DIRECTION ( 'NONE',  ( 5.188838149069472160E-16, -1.699382548006136559E-16, -1.000000000000000000 ) ) ;
#8490 = CARTESIAN_POINT ( 'NONE',  ( -41.63373767251881929, 22.51256436878201939, 1.325597493787631587 ) ) ;
#8491 = CARTESIAN_POINT ( 'NONE',  ( -11.41714695485569742, 57.14999999999998437, -5.016499999999999737 ) ) ;
#8492 = CARTESIAN_POINT ( 'NONE',  ( 6.075699028729387052, 121.3938335755924243, 0.3948700328016164218 ) ) ;
#8493 = CARTESIAN_POINT ( 'NONE',  ( 3.707542801486926276, 23.89195667223011910, -2.776928957275885068 ) ) ;
#8494 = CARTESIAN_POINT ( 'NONE',  ( 22.70140800483388688, 148.7873826295267747, 1.635989027091525161 ) ) ;
#8495 = CYLINDRICAL_SURFACE ( 'NONE', #25200, 0.2539999999999986158 ) ;
#8497 = CARTESIAN_POINT ( 'NONE',  ( 11.93281433870457775, 156.4809912657682673, -1.479000486392926916 ) ) ;
#8496 = CARTESIAN_POINT ( 'NONE',  ( 3.047145566129288330, -14.72663143740328806, 3.823360744794035870 ) ) ;
#8498 = CARTESIAN_POINT ( 'NONE',  ( -18.43358770356691068, 147.0160646422468744, 1.663356549802410989 ) ) ;
#8499 = CARTESIAN_POINT ( 'NONE',  ( -2.133573495637306916, 19.78131850274109382, 4.120466288703205748 ) ) ;
#8500 = CARTESIAN_POINT ( 'NONE',  ( -18.33253411489134876, 154.1536317137893661, -1.165609363665846221 ) ) ;
#8501 = CARTESIAN_POINT ( 'NONE',  ( 0.5691593726700751033, 20.64373787749807576, 0.7897743370290384313 ) ) ;
#8502 = VERTEX_POINT ( 'NONE', #32723 ) ;
#8503 = CARTESIAN_POINT ( 'NONE',  ( -56.39145920764457287, 3.696195836928164891, 1.449839391286695589 ) ) ;
#8504 = CARTESIAN_POINT ( 'NONE',  ( -12.53742732955040395, 130.7145975665201831, 0.5304871790577964097 ) ) ;
#8505 = CARTESIAN_POINT ( 'NONE',  ( 4.077043646397369159, -14.32506836492906999, 4.807529146363894057 ) ) ;
#8506 = CARTESIAN_POINT ( 'NONE',  ( 13.27577938203601526, 128.5100244389050204, -1.209575533060949892 ) ) ;
#8507 = ORIENTED_EDGE ( 'NONE', *, *, #40447, .F. ) ;
#8508 = CARTESIAN_POINT ( 'NONE',  ( 2.225394578381316268, 115.7029491485453150, 1.707871263558881969 ) ) ;
#8509 = ORIENTED_EDGE ( 'NONE', *, *, #24317, .F. ) ;
#8510 = CARTESIAN_POINT ( 'NONE',  ( 3.188489192988832155, -14.31930622237681483, 3.473944028487384372 ) ) ;
#8511 = CARTESIAN_POINT ( 'NONE',  ( -4.691900465594415870, 117.8976975978048642, -0.9735392405797208548 ) ) ;
#8512 = CARTESIAN_POINT ( 'NONE',  ( 3.751144962740032618, 121.0949217282140182, 0.04819499160668145460 ) ) ;
#8513 = ORIENTED_EDGE ( 'NONE', *, *, #33182, .T. ) ;
#8514 = CARTESIAN_POINT ( 'NONE',  ( 19.69933843609242530, 149.7343351798865285, 2.455316921491699667 ) ) ;
#8515 = LINE ( 'NONE', #27887, #10887 ) ;
#8516 = DIRECTION ( 'NONE',  ( -0.9998004120163608288, 0.000000000000000000, -0.01997839162482749342 ) ) ;
#8517 = EDGE_CURVE ( 'NONE', #16752, #28439, #35646, .T. ) ;
#8518 = CARTESIAN_POINT ( 'NONE',  ( 0.03153862713803012863, 157.4657262375360176, -1.578321868909182246 ) ) ;
#8519 = CARTESIAN_POINT ( 'NONE',  ( 1.411700740068499993, 159.5982469381528972, -0.1593474270858732111 ) ) ;
#8520 = CARTESIAN_POINT ( 'NONE',  ( -5.256666791691372076, 57.15000000000019043, -5.296388421271849722 ) ) ;
#8521 = CARTESIAN_POINT ( 'NONE',  ( 1.760709524605698961, -15.18916190965080659, 5.866327383715185917 ) ) ;
#8522 = CARTESIAN_POINT ( 'NONE',  ( 10.94257363143051087, 56.35470871607771670, 4.428493390990901446 ) ) ;
#8523 = CARTESIAN_POINT ( 'NONE',  ( -6.059261036834472591, 56.98375738874752727, -5.016500000000000625 ) ) ;
#8524 = CARTESIAN_POINT ( 'NONE',  ( -4.894527635837473412, 117.7423471277129607, 0.7194462064511487620 ) ) ;
#8525 = B_SPLINE_SURFACE_WITH_KNOTS ( 'NONE', 3, 1, ( 
 ( #29478, #29262 ),
 ( #4143, #6908 ),
 ( #32466, #13287 ),
 ( #19878, #13916 ),
 ( #23061, #32892 ) ),
 .UNSPECIFIED., .F., .F., .F.,
 ( 4, 1, 4 ),
 ( 2, 2 ),
 ( 0.000000000000000000, 0.4760613254002281081, 0.9521226508004562161 ),
 ( 0.000000000000000000, 1.000000000000000000 ),
 .UNSPECIFIED. ) ;
#8526 = EDGE_LOOP ( 'NONE', ( #40626, #25995, #152, #26633 ) ) ;
#8527 = ORIENTED_EDGE ( 'NONE', *, *, #13418, .T. ) ;
#8528 = CARTESIAN_POINT ( 'NONE',  ( -5.369399562154598904, 64.90898011766716991, -1.269999999999993578 ) ) ;
#8529 = CARTESIAN_POINT ( 'NONE',  ( -2.865660977700466017, 118.0055230577426073, -0.8541496112950387465 ) ) ;
#8530 = CARTESIAN_POINT ( 'NONE',  ( -4.807558371750645598, 117.0601473006971105, -0.9798501506189060128 ) ) ;
#8531 = CARTESIAN_POINT ( 'NONE',  ( 4.909831060657428026, 117.4773178990584483, 1.095440290055193389 ) ) ;
#8532 = CARTESIAN_POINT ( 'NONE',  ( -11.58677707360117282, 55.41127257906206438, -4.474811398756911807 ) ) ;
#8533 = CARTESIAN_POINT ( 'NONE',  ( -0.8223074630897415638, 121.2007779179981384, 0.3881979734473210431 ) ) ;
#8534 = CARTESIAN_POINT ( 'NONE',  ( 4.529186081025091681, -11.15152372915077095, -0.9203776863585164669 ) ) ;
#8535 = CARTESIAN_POINT ( 'NONE',  ( -57.80205714066466527, 2.371715784325115095, 1.753227392946289154 ) ) ;
#8536 = DIRECTION ( 'NONE',  ( -4.017660918040594346E-17, 1.000000000000000000, 2.376309959284834438E-19 ) ) ;
#8537 = CARTESIAN_POINT ( 'NONE',  ( 3.214659515886821861, -12.19625089790456229, 0.4983212145216010525 ) ) ;
#8538 = CARTESIAN_POINT ( 'NONE',  ( 6.675377558974045833, 121.2389289720308199, -0.07470202506228480754 ) ) ;
#8539 = CARTESIAN_POINT ( 'NONE',  ( 6.076994399821980863, 121.4412224314809521, 0.1214066477987181120 ) ) ;
#8540 = CARTESIAN_POINT ( 'NONE',  ( -5.361994333976945803, 30.20544108279508677, 3.344879823269458985 ) ) ;
#8541 = CIRCLE ( 'NONE', #33701, 12.69999999999999751 ) ;
#8542 = CARTESIAN_POINT ( 'NONE',  ( -0.7578723423243420854, 115.7030198846401134, 1.728701198025235364 ) ) ;
#8543 = CARTESIAN_POINT ( 'NONE',  ( -2.136650056307613621, 10.86338872207680950, -4.114640003288728920 ) ) ;
#8545 = EDGE_LOOP ( 'NONE', ( #15802, #37512, #23781, #12479 ) ) ;
#8544 = CARTESIAN_POINT ( 'NONE',  ( 23.18613385382694503, 148.9919839608952827, 1.059503902452021640 ) ) ;
#8546 = CARTESIAN_POINT ( 'NONE',  ( 5.024936854470411163, 105.1216725936605201, -1.825215542048775674 ) ) ;
#8547 = CARTESIAN_POINT ( 'NONE',  ( 2.631420558634286255, -15.64638348417481062, 4.926794133592228064 ) ) ;
#8548 = CARTESIAN_POINT ( 'NONE',  ( -2.301458206243153892, 118.5910164976458532, 0.7067537174111425680 ) ) ;
#8549 = CARTESIAN_POINT ( 'NONE',  ( -0.9107729336552147226, 17.84451472381387305, 0.3451692354151053577 ) ) ;
#8550 = CARTESIAN_POINT ( 'NONE',  ( -0.8615061033338488050, 12.60145565637890286, -0.4637196408544374537 ) ) ;
#8551 = EDGE_LOOP ( 'NONE', ( #32545, #28515, #21808 ) ) ;
#8552 = ORIENTED_EDGE ( 'NONE', *, *, #35525, .F. ) ;
#8553 = DIRECTION ( 'NONE',  ( 0.9336303900108928744, 0.3582377630123714241, 0.000000000000000000 ) ) ;
#8554 = CARTESIAN_POINT ( 'NONE',  ( 3.315491766441247101, 124.7872298565087021, 0.07248898146901455730 ) ) ;
#8555 = SURFACE_STYLE_FILL_AREA ( #14714 ) ;
#8556 = CARTESIAN_POINT ( 'NONE',  ( -13.46182233857078536, 130.9706359334022920, 1.049250031952806861 ) ) ;
#8557 = DIRECTION ( 'NONE',  ( -4.017660918040594346E-17, 1.000000000000000000, 2.376309959284834438E-19 ) ) ;
#8558 = CARTESIAN_POINT ( 'NONE',  ( 2.265044067826554652, -14.95788512594138631, 5.210342366881125287 ) ) ;
#8559 = CARTESIAN_POINT ( 'NONE',  ( 18.15383854178424272, 147.5382818419693649, -1.618175512470155120 ) ) ;
#8560 = CARTESIAN_POINT ( 'NONE',  ( -12.21120734956430809, 121.7247091083657153, -1.742548127100890243 ) ) ;
#8561 = DIRECTION ( 'NONE',  ( 6.104810211199659290E-14, 1.534542364845396606E-13, 1.000000000000000000 ) ) ;
#8562 = CARTESIAN_POINT ( 'NONE',  ( -6.442297258278467886, 29.65178619621697464, 0.8020365093557801917 ) ) ;
#8563 = CARTESIAN_POINT ( 'NONE',  ( 9.242439611670231869, 123.9961275534082148, -0.1349267066575718654 ) ) ;
#8564 = ORIENTED_EDGE ( 'NONE', *, *, #37299, .F. ) ;
#8565 = CARTESIAN_POINT ( 'NONE',  ( 2.568134854143032442, -15.02010252187911554, 4.714990346623905815 ) ) ;
#8566 = DIRECTION ( 'NONE',  ( 0.4849315768086534528, 0.8745520943968249084, 1.030032898892974818E-16 ) ) ;
#8567 = CARTESIAN_POINT ( 'NONE',  ( -57.60629982073535871, 1.412843483088787044, 1.546595473637959239 ) ) ;
#8568 = CIRCLE ( 'NONE', #32370, 0.5080000000000000071 ) ;
#8569 = CARTESIAN_POINT ( 'NONE',  ( 3.417104117279694098, -14.34023910220586906, -3.129441506049576383 ) ) ;
#8570 = CARTESIAN_POINT ( 'NONE',  ( 16.94675455810613229, 147.0740084267719396, 1.925552282123431436 ) ) ;
#8571 = CARTESIAN_POINT ( 'NONE',  ( 2.887677632297840802, 37.80609079512323234, 0.7577488597010552107 ) ) ;
#8572 = CARTESIAN_POINT ( 'NONE',  ( -7.588858076165209354, 124.2943531750336490, -0.1426133663090954629 ) ) ;
#8573 = CARTESIAN_POINT ( 'NONE',  ( 0.05711764529616595448, 0.5181683540770932739, -4.631227783250111862 ) ) ;
#8574 = CARTESIAN_POINT ( 'NONE',  ( -0.0005468344959659662699, 156.3034662015456604, 0.02736583427618497280 ) ) ;
#8575 = CARTESIAN_POINT ( 'NONE',  ( 4.050812540078617019, -7.421221357003889629, 7.384888961799156881 ) ) ;
#8576 = CARTESIAN_POINT ( 'NONE',  ( -56.88731995051697510, 2.378615435641926013, -1.029510524999914353E-14 ) ) ;
#8577 = CARTESIAN_POINT ( 'NONE',  ( 2.159899147946715114, 116.3864810981202851, -0.2326697378273381023 ) ) ;
#8578 = CARTESIAN_POINT ( 'NONE',  ( -0.3665064675492638036, 121.9236798544226730, -0.3444762419765420303 ) ) ;
#8579 = PLANE ( 'NONE',  #24623 ) ;
#8580 = CARTESIAN_POINT ( 'NONE',  ( -10.55305098051677248, 77.31887769575739355, -1.523999999999998467 ) ) ;
#8581 = CARTESIAN_POINT ( 'NONE',  ( 4.622858883031034871, 26.85595184169372374, 0.2084198311932836112 ) ) ;
#8582 = DIRECTION ( 'NONE',  ( 1.000000000000000000, 0.000000000000000000, 0.000000000000000000 ) ) ;
#8583 = CARTESIAN_POINT ( 'NONE',  ( -5.486567272856878414E-14, 86.35999999999998522, 0.000000000000000000 ) ) ;
#8584 = CARTESIAN_POINT ( 'NONE',  ( 7.213960532363571154, 78.77618639008812806, -1.904999999999999583 ) ) ;
#8585 = CARTESIAN_POINT ( 'NONE',  ( 0.1065646865914871289, 105.8844662015457203, -5.332932678536313809 ) ) ;
#8586 = CARTESIAN_POINT ( 'NONE',  ( -19.95587765737807828, 128.8226523212408949, 0.2284701554834995540 ) ) ;
#8587 = ORIENTED_EDGE ( 'NONE', *, *, #32686, .T. ) ;
#8588 = CARTESIAN_POINT ( 'NONE',  ( -58.33482727260580702, 1.278009831241974759, -1.053392386569325874E-14 ) ) ;
#8589 = VERTEX_POINT ( 'NONE', #10130 ) ;
#8590 = DIRECTION ( 'NONE',  ( 0.9998004120163609398, 4.016384292689130894E-17, 0.01997839162482749689 ) ) ;
#8591 = CARTESIAN_POINT ( 'NONE',  ( -9.104209967888042598, 153.9432936505793066, -0.1819237819739442652 ) ) ;
#8592 = CARTESIAN_POINT ( 'NONE',  ( 3.829091000068871598, -15.41100336169511031, 5.152250049158875633 ) ) ;
#8593 = CARTESIAN_POINT ( 'NONE',  ( -13.79335258734193914, 122.1113760975138263, 1.168436778447113689 ) ) ;
#8594 = CARTESIAN_POINT ( 'NONE',  ( 0.01645572339161061742, 159.4324016994384010, -0.8235116888278192215 ) ) ;
#8595 = CARTESIAN_POINT ( 'NONE',  ( -4.603678009535974169, 12.38766144714272066, -0.4343361176327051321 ) ) ;
#8596 = CIRCLE ( 'NONE', #7933, 0.2539999999999990599 ) ;
#8597 = CARTESIAN_POINT ( 'NONE',  ( -3.781797959329980863, 116.7736770086926867, -0.3417761088697101601 ) ) ;
#8598 = CARTESIAN_POINT ( 'NONE',  ( -51.53167472531687565, 13.74790139509799936, -4.551524594881854568 ) ) ;
#8599 = AXIS2_PLACEMENT_3D ( 'NONE', #41224, #2676, #35459 ) ;
#8600 = CARTESIAN_POINT ( 'NONE',  ( -2.183475033498248230, 116.1883682894288796, -0.03369517848931347787 ) ) ;
#8601 = CARTESIAN_POINT ( 'NONE',  ( -38.65395868481546415, 29.38327706004843876, -1.524000000000004906 ) ) ;
#8602 = CARTESIAN_POINT ( 'NONE',  ( -11.26369337785518709, 123.4744472594011739, 1.139971239082961052 ) ) ;
#8603 = CIRCLE ( 'NONE', #32404, 0.6350000000000014522 ) ;
#8604 = CARTESIAN_POINT ( 'NONE',  ( -56.22633580991770685, 4.287755688858543301, -2.325607019181227475 ) ) ;
#8605 = CARTESIAN_POINT ( 'NONE',  ( 19.29133405012190750, 147.6776069388173767, -1.737063910747457030 ) ) ;
#8606 = CARTESIAN_POINT ( 'NONE',  ( -21.19397400757792482, 145.8710773725474610, -2.320968965272669937 ) ) ;
#8607 = CARTESIAN_POINT ( 'NONE',  ( -50.15972161391664486, 17.13814111569220699, -4.955022299345085202 ) ) ;
#8608 = CARTESIAN_POINT ( 'NONE',  ( 9.599121003648848571, 153.9312916436033447, -0.7969471826422132033 ) ) ;
#8609 = ORIENTED_EDGE ( 'NONE', *, *, #7707, .F. ) ;
#8610 = CARTESIAN_POINT ( 'NONE',  ( -17.59644933020973667, 144.4767212251450417, -2.299577266864829994 ) ) ;
#8611 = CARTESIAN_POINT ( 'NONE',  ( 3.857521300888583582, -15.67877420849868386, 3.673684628067402702 ) ) ;
#8612 = CARTESIAN_POINT ( 'NONE',  ( -4.065972646788793554, 118.2429491485453070, -0.3080848862740693250 ) ) ;
#8613 = EDGE_CURVE ( 'NONE', #38737, #41570, #14919, .T. ) ;
#8614 = EDGE_CURVE ( 'NONE', #41032, #28056, #9727, .T. ) ;
#8615 = CARTESIAN_POINT ( 'NONE',  ( -58.40597088826705630, 0.2738206778524349128, -0.9753506901443967925 ) ) ;
#8616 = CARTESIAN_POINT ( 'NONE',  ( -4.987820457167934762, 117.4712984309037438, 0.8194575654087326022 ) ) ;
#8617 = CARTESIAN_POINT ( 'NONE',  ( 2.063908814988649532, 157.0334531201187644, 1.539797002863053210 ) ) ;
#8618 = DIRECTION ( 'NONE',  ( -5.206863593109713045E-17, 1.000000000000000000, -1.077750396879097359E-30 ) ) ;
#8619 = CARTESIAN_POINT ( 'NONE',  ( -3.210878647048973189, -8.553304832117262890, -7.794174491370510438 ) ) ;
#8620 = CARTESIAN_POINT ( 'NONE',  ( 6.044022022451693843, 155.3491655920357459, 0.4731370799734938015 ) ) ;
#8621 = DIRECTION ( 'NONE',  ( -0.9816537812491094028, -0.1906721105965052399, 6.949828216605158287E-15 ) ) ;
#8623 = ORIENTED_EDGE ( 'NONE', *, *, #38592, .F. ) ;
#8622 = CARTESIAN_POINT ( 'NONE',  ( 17.68910244842765778, 8.844871939465424049, 0.000000000000000000 ) ) ;
#8624 = CARTESIAN_POINT ( 'NONE',  ( -4.862565162136183616, 117.4116260025058693, -1.165543200563879056 ) ) ;
#8625 = CARTESIAN_POINT ( 'NONE',  ( -7.836093358135542530, 122.3276016517421994, -0.6978168763808364483 ) ) ;
#8626 = CARTESIAN_POINT ( 'NONE',  ( -5.871452009091383317, 65.30181249999998272, -5.016499999999999737 ) ) ;
#8627 = CARTESIAN_POINT ( 'NONE',  ( -50.94572941386617515, 18.90544291192138004, 2.223209376321575004 ) ) ;
#8628 = CARTESIAN_POINT ( 'NONE',  ( -23.28495812418893607, 149.3453998935430604, -0.3112269551726869476 ) ) ;
#8629 = B_SPLINE_CURVE_WITH_KNOTS ( 'NONE', 5,
 ( #30360, #20972, #23750, #14369, #39978, #36770, #583, #20549 ),
 .UNSPECIFIED., .F., .F.,
 ( 6, 2, 6 ),
 ( -5.999999999695239656E-08, 0.0004919218780628863792, 0.0009839037561257695831 ),
 .UNSPECIFIED. ) ;
#8630 = ORIENTED_EDGE ( 'NONE', *, *, #28953, .F. ) ;
#8631 = CARTESIAN_POINT ( 'NONE',  ( -50.95401363114979176, 21.69085172357045010, -1.082912443856812391E-14 ) ) ;
#8632 = CARTESIAN_POINT ( 'NONE',  ( -7.841358516840601034, 122.2961712410880324, -0.7253305154435645274 ) ) ;
#8633 = CARTESIAN_POINT ( 'NONE',  ( -8.262035544818829180, 120.4240392771559414, 1.115000201712872618 ) ) ;
#8634 = ORIENTED_EDGE ( 'NONE', *, *, #18492, .T. ) ;
#8635 = CARTESIAN_POINT ( 'NONE',  ( -47.84356795211458291, 19.38525671449504983, 5.197506975155153697 ) ) ;
#8636 = CARTESIAN_POINT ( 'NONE',  ( -13.02783148976621774, 133.9378623523624299, -0.5757418746946230126 ) ) ;
#8637 = CARTESIAN_POINT ( 'NONE',  ( 4.896986379477733742, -14.09362661677580952, 4.057159877996594055 ) ) ;
#8638 = CARTESIAN_POINT ( 'NONE',  ( -7.994725381675435116, 118.4344479264803169, 0.7928399906090751736 ) ) ;
#8639 = CIRCLE ( 'NONE', #36541, 0.2539999999999931202 ) ;
#8640 = DIRECTION ( 'NONE',  ( -4.017660918040594346E-17, 1.000000000000000000, 2.376309959284834438E-19 ) ) ;
#8641 = CARTESIAN_POINT ( 'NONE',  ( 22.97436839085978733, 150.1579452496398801, 0.6125673049107098755 ) ) ;
#8642 = TOROIDAL_SURFACE ( 'NONE', #19510, 4.826000000000000512, 0.5080000000000000071 ) ;
#8643 = CARTESIAN_POINT ( 'NONE',  ( 9.126830667405478437, 124.2274448616014411, 0.2272647324663854829 ) ) ;
#8644 = CARTESIAN_POINT ( 'NONE',  ( -4.903827551164339660, 117.7626876103193325, 0.5344712183346053136 ) ) ;
#8645 = CARTESIAN_POINT ( 'NONE',  ( 0.7580923926444932404, 28.79380631387826028, -0.6184068814828035388 ) ) ;
#8646 = ADVANCED_FACE ( 'NONE', ( #3977 ), #3385, .T. ) ;
#8647 = CARTESIAN_POINT ( 'NONE',  ( -23.21042342040066231, 149.6290410902582551, -0.5408589295980601452 ) ) ;
#8648 = CARTESIAN_POINT ( 'NONE',  ( -41.08173151913536003, 23.06272320883578075, -1.524000000017811773 ) ) ;
#8649 = CARTESIAN_POINT ( 'NONE',  ( -5.579075174912628832, 56.51499999999997925, -4.418274828058819992 ) ) ;
#8650 = ORIENTED_EDGE ( 'NONE', *, *, #10267, .F. ) ;
#8651 = CARTESIAN_POINT ( 'NONE',  ( 8.283808458469433589, 120.0678368811737755, 1.450790680561929280 ) ) ;
#8652 = LINE ( 'NONE', #41246, #27933 ) ;
#8653 = CARTESIAN_POINT ( 'NONE',  ( 19.72970310060704335, 132.0165317526581816, 1.843001364771305939 ) ) ;
#8654 = AXIS2_PLACEMENT_3D ( 'NONE', #32729, #39118, #154 ) ;
#8655 = CARTESIAN_POINT ( 'NONE',  ( 4.992797058274879518, 118.5534682650580862, -0.8674252695128576995 ) ) ;
#8656 = CARTESIAN_POINT ( 'NONE',  ( -4.326994387844902867, 19.77997674669536465, 7.266063235268683584 ) ) ;
#8657 = CARTESIAN_POINT ( 'NONE',  ( -22.23208127788764443, 149.2301036976659816, -1.887777678714757768 ) ) ;
#8658 = CARTESIAN_POINT ( 'NONE',  ( 4.907634972350170877, 117.7148210790128360, -0.7337193700908156702 ) ) ;
#8659 = CARTESIAN_POINT ( 'NONE',  ( 5.011858831344538245, 114.3657942991566472, 1.958205155698268696 ) ) ;
#8660 = ORIENTED_EDGE ( 'NONE', *, *, #18578, .T. ) ;
#8661 = AXIS2_PLACEMENT_3D ( 'NONE', #36672, #17275, #33691 ) ;
#8662 = CARTESIAN_POINT ( 'NONE',  ( -9.001127587916252892, 123.9218113011205986, -0.09563458650452036358 ) ) ;
#8663 = CARTESIAN_POINT ( 'NONE',  ( -13.10180873912566035, 153.9517556018257096, -2.260155593826742582 ) ) ;
#8664 = CARTESIAN_POINT ( 'NONE',  ( 5.095505811086057157, -15.28584205578724386, 3.479711806413861908 ) ) ;
#8665 = FACE_OUTER_BOUND ( 'NONE', #7137, .T. ) ;
#8666 = CARTESIAN_POINT ( 'NONE',  ( -0.6964149855636846409, 117.3993842960376099, -1.488886793157482957 ) ) ;
#8667 = ORIENTED_EDGE ( 'NONE', *, *, #1928, .F. ) ;
#8668 = CARTESIAN_POINT ( 'NONE',  ( 18.59210649535962290, 147.7499600834086948, 2.443498639627972313 ) ) ;
#8669 = DIRECTION ( 'NONE',  ( -1.011795553208986377E-16, -1.000000000000000000, 0.000000000000000000 ) ) ;
#8670 = CARTESIAN_POINT ( 'NONE',  ( 4.756814333351318425, 117.4032681585794791, 1.206529664789174339 ) ) ;
#8671 = CIRCLE ( 'NONE', #18874, 0.3810000000000015041 ) ;
#8672 = CARTESIAN_POINT ( 'NONE',  ( -0.3374525697216100295, 106.5118632461160217, 5.070939582669566903 ) ) ;
#8673 = CARTESIAN_POINT ( 'NONE',  ( -5.378050908718009282, 0.3500678860072145016, 6.480130142454380682 ) ) ;
#8674 = CARTESIAN_POINT ( 'NONE',  ( 9.619667158014634012, 123.8920215319950842, 0.8772578247576550137 ) ) ;
#8675 = PLANE ( 'NONE',  #4977 ) ;
#8676 = EDGE_CURVE ( 'NONE', #41701, #2340, #5433, .T. ) ;
#8677 = CARTESIAN_POINT ( 'NONE',  ( 5.566083668711077515, 159.0643023895801491, -0.5661052595122396669 ) ) ;
#8678 = DIRECTION ( 'NONE',  ( 0.8745520943968235761, -0.4849315768086558398, 0.000000000000000000 ) ) ;
#8679 = CARTESIAN_POINT ( 'NONE',  ( -58.28980089130899245, -0.1221305639422176070, 0.3636100989710047693 ) ) ;
#8680 = CARTESIAN_POINT ( 'NONE',  ( 1.204770341778093456E-15, 12.51401280605345967, 0.000000000000000000 ) ) ;
#8681 = CARTESIAN_POINT ( 'NONE',  ( -4.118105137886063360, 118.2429491485453354, 0.1865571212249754751 ) ) ;
#8682 = CARTESIAN_POINT ( 'NONE',  ( -23.29144772315980916, 149.3526176766912101, -0.4654185560736369132 ) ) ;
#8683 = CIRCLE ( 'NONE', #23532, 0.5079999999999968985 ) ;
#8684 = ORIENTED_EDGE ( 'NONE', *, *, #28211, .F. ) ;
#8685 = EDGE_CURVE ( 'NONE', #12906, #16433, #11712, .T. ) ;
#8686 = CARTESIAN_POINT ( 'NONE',  ( -51.09990735641632398, 14.52648110433587370, 4.713018929684107405 ) ) ;
#8687 = CARTESIAN_POINT ( 'NONE',  ( -6.268960521413761811, 119.8969868274346027, -1.221708021102049901 ) ) ;
#8688 = CARTESIAN_POINT ( 'NONE',  ( -5.336420303164543633, 104.6144662015457101, 0.06783417913549341649 ) ) ;
#8689 = CARTESIAN_POINT ( 'NONE',  ( -9.371428955827290963, 153.8930958044198576, -0.9350090023289892027 ) ) ;
#8690 = DIRECTION ( 'NONE',  ( -0.6559537821943236535, 0.7548010569845287066, 2.445308717870848367E-15 ) ) ;
#8691 = CARTESIAN_POINT ( 'NONE',  ( 16.18905205736044906, 121.2598130428683447, 0.3234957879086921562 ) ) ;
#8692 = VERTEX_POINT ( 'NONE', #4402 ) ;
#8693 = CARTESIAN_POINT ( 'NONE',  ( -0.1328416520900886078, 24.48205809745167372, 4.627450821846854190 ) ) ;
#8694 = CARTESIAN_POINT ( 'NONE',  ( -33.42971872652991294, 49.93539301574497813, 1.523999999999990917 ) ) ;
#8695 = CARTESIAN_POINT ( 'NONE',  ( -5.078986093043185157, 66.13346620154574396, -0.1014902294541238092 ) ) ;
#8696 = CARTESIAN_POINT ( 'NONE',  ( -42.61647787783788743, 21.91010357080768856, 1.992259954793912158 ) ) ;
#8697 = DIRECTION ( 'NONE',  ( 0.01997839162482749689, 1.040247600000945640E-18, -0.9998004120163610509 ) ) ;
#8698 = CARTESIAN_POINT ( 'NONE',  ( 6.990876450665549413, 121.9332825538419200, 0.2917046836452048542 ) ) ;
#8699 = EDGE_CURVE ( 'NONE', #28106, #5804, #17662, .T. ) ;
#8700 = LINE ( 'NONE', #28289, #32035 ) ;
#8701 = CARTESIAN_POINT ( 'NONE',  ( 1.336693583852395673, 159.4956652290339605, 0.6991310044172547311 ) ) ;
#8702 = CARTESIAN_POINT ( 'NONE',  ( -4.694219104381005536, 104.6144662015457953, -1.165030450612820623 ) ) ;
#8704 = CARTESIAN_POINT ( 'NONE',  ( 13.10001109591386559, 121.1598417376693533, -1.052633080380691144 ) ) ;
#8703 = CARTESIAN_POINT ( 'NONE',  ( 3.186936940905604754, -14.67134942876716153, 3.163583609075255598 ) ) ;
#8705 = CARTESIAN_POINT ( 'NONE',  ( -7.718355369771888519, 156.1362479297160348, 1.656311413603696936 ) ) ;
#8706 = CARTESIAN_POINT ( 'NONE',  ( -0.1338072975148606736, -13.68656151007796495, -0.9662261747338762863 ) ) ;
#8707 = CARTESIAN_POINT ( 'NONE',  ( -8.135778112230864778, 117.7673425867732249, -0.7050676646501271572 ) ) ;
#8708 = PRODUCT_DEFINITION_FORMATION_WITH_SPECIFIED_SOURCE ( 'ANY', '', #30001, .NOT_KNOWN. ) ;
#8709 = EDGE_CURVE ( 'NONE', #30779, #6194, #35926, .T. ) ;
#8710 = CARTESIAN_POINT ( 'NONE',  ( -0.3421040304481134942, 19.14286131909006272, 0.9136164113388466346 ) ) ;
#8711 = ORIENTED_EDGE ( 'NONE', *, *, #5335, .T. ) ;
#8712 = CARTESIAN_POINT ( 'NONE',  ( -55.14069116334859189, 5.401725095812784261, -9.468868952413029037E-15 ) ) ;
#8713 = CARTESIAN_POINT ( 'NONE',  ( -8.002172173406888689, 154.6030710842251494, 0.4507127070663228263 ) ) ;
#8714 = CARTESIAN_POINT ( 'NONE',  ( 5.820712434538892310, -12.64545009755467575, 1.387492028720230364 ) ) ;
#8715 = CARTESIAN_POINT ( 'NONE',  ( 6.842818979164380089, 155.5980657034081105, -1.215443052661050460 ) ) ;
#8716 = ORIENTED_EDGE ( 'NONE', *, *, #25566, .T. ) ;
#8717 = CARTESIAN_POINT ( 'NONE',  ( 0.6864031510614769793, 115.7029491485453576, 1.757686897103055923 ) ) ;
#8718 = CARTESIAN_POINT ( 'NONE',  ( -4.742366482708093578, 117.6343161886170208, -1.141804636843513965 ) ) ;
#8719 = CARTESIAN_POINT ( 'NONE',  ( 12.91960671971514252, 133.8340822528099636, 0.1412842392263899960 ) ) ;
#8720 = EDGE_CURVE ( 'NONE', #20977, #16752, #40821, .T. ) ;
#8721 = ORIENTED_EDGE ( 'NONE', *, *, #16216, .F. ) ;
#8722 = CARTESIAN_POINT ( 'NONE',  ( -0.01147819631913261050, 118.5605975114896609, 0.5744158801423953076 ) ) ;
#8723 = DIRECTION ( 'NONE',  ( -5.206863593109713661E-17, 1.000000000000000000, -1.077750396879097183E-30 ) ) ;
#8724 = CARTESIAN_POINT ( 'NONE',  ( 17.68910244842765778, -7.669212195657745698E-17, 0.000000000000000000 ) ) ;
#8725 = CARTESIAN_POINT ( 'NONE',  ( 0.02156508032615568615, 159.2730288250082538, -1.079204802879467406 ) ) ;
#8726 = CARTESIAN_POINT ( 'NONE',  ( 23.31467963135034438, 142.7201128741078833, 0.1336249016415858304 ) ) ;
#8727 = CARTESIAN_POINT ( 'NONE',  ( -14.73199999999999399, 17.14499999999999957, 0.000000000000000000 ) ) ;
#8728 = AXIS2_PLACEMENT_3D ( 'NONE', #13683, #1124, #28353 ) ;
#8729 = CARTESIAN_POINT ( 'NONE',  ( 1.801801447854238569, -15.42219197509341022, 5.395122923460818676 ) ) ;
#8730 = CARTESIAN_POINT ( 'NONE',  ( -4.095482865093060809, 71.62450171983788039, 1.524000000000005350 ) ) ;
#8731 = CARTESIAN_POINT ( 'NONE',  ( -6.564189886853176475E-14, 81.62746620154572952, -5.847435218134868453E-18 ) ) ;
#8732 = EDGE_CURVE ( 'NONE', #11424, #4990, #93, .T. ) ;
#8733 = CARTESIAN_POINT ( 'NONE',  ( -4.662673704711017386, 117.9838541597224406, 0.7073371538211529197 ) ) ;
#8734 = EDGE_CURVE ( 'NONE', #25703, #39961, #29523, .T. ) ;
#8735 = ORIENTED_EDGE ( 'NONE', *, *, #21417, .T. ) ;
#8736 = VERTEX_POINT ( 'NONE', #25173 ) ;
#8737 = CARTESIAN_POINT ( 'NONE',  ( -5.968544434436104299E-14, 66.13346620154574396, 9.705588791358230112E-17 ) ) ;
#8738 = CARTESIAN_POINT ( 'NONE',  ( -8.527069590570199864, 118.9013125089547600, -1.248037646211100249 ) ) ;
#8739 = CARTESIAN_POINT ( 'NONE',  ( -4.183818394377370353, 118.4033805524614849, -0.7412457532797813720 ) ) ;
#8740 = CARTESIAN_POINT ( 'NONE',  ( 4.859669866895486301, 117.7242276672350272, 0.9631597096148959425 ) ) ;
#8741 = LINE ( 'NONE', #27698, #7323 ) ;
#8742 = CARTESIAN_POINT ( 'NONE',  ( -0.07157677169895493297, 110.3683645023726569, 3.581994345755985076 ) ) ;
#8743 = DIRECTION ( 'NONE',  ( 0.8745520943968249084, -0.4849315768086533418, 5.271987356194193006E-16 ) ) ;
#8744 = CARTESIAN_POINT ( 'NONE',  ( 5.005702202344075147, 117.4009237673399610, -0.7895530272732956822 ) ) ;
#8745 = DIRECTION ( 'NONE',  ( -0.8745520943968243532, 0.4849315768086547296, -5.361993529360573944E-16 ) ) ;
#8746 = CARTESIAN_POINT ( 'NONE',  ( 3.427377709871179512, -13.85078959623727002, 3.379007147668904754 ) ) ;
#8747 = CARTESIAN_POINT ( 'NONE',  ( 6.300951452924033802, 121.9812576474260055, -0.03014847038595253048 ) ) ;
#8748 = CARTESIAN_POINT ( 'NONE',  ( -10.53370020345052893, 154.2769816202975051, -1.888232850154634823 ) ) ;
#8749 = CARTESIAN_POINT ( 'NONE',  ( -7.785932599179138158, 122.6147803075941454, -0.2294614199791660536 ) ) ;
#8750 = CARTESIAN_POINT ( 'NONE',  ( -2.169500164636429140, 35.42160933236649356, 3.123960633263313635 ) ) ;
#8751 = CARTESIAN_POINT ( 'NONE',  ( -0.2889451677547653641, 115.7029882247660879, 1.754375496046200578 ) ) ;
#8752 = CARTESIAN_POINT ( 'NONE',  ( 4.617411384770501392, 7.639850289152962048, 0.2838591255797697777 ) ) ;
#8754 = ORIENTED_EDGE ( 'NONE', *, *, #13430, .F. ) ;
#8753 = CARTESIAN_POINT ( 'NONE',  ( -0.006534887713674795984, 159.5822087645323393, 0.3270325034788581497 ) ) ;
#8755 = CARTESIAN_POINT ( 'NONE',  ( 4.270891071783644577, 105.1220196924935237, -3.200937537902331709 ) ) ;
#8756 = CARTESIAN_POINT ( 'NONE',  ( 2.294714809908028119, -15.51018114022951977, 5.078884642465592236 ) ) ;
#8757 = CARTESIAN_POINT ( 'NONE',  ( -9.796729639280952640, 120.9522862504114897, 1.196371290339073079 ) ) ;
#8758 = VECTOR ( 'NONE', #35203, 1000.000000000000000 ) ;
#8759 = CARTESIAN_POINT ( 'NONE',  ( 0.9476013557874021220, 22.48150014755712078, -0.2491751695904415032 ) ) ;
#8760 = ADVANCED_FACE ( 'NONE', ( #2613, #15147 ), #37168, .F. ) ;
#8761 = CARTESIAN_POINT ( 'NONE',  ( -0.5883093083485460006, 14.76436220226899465, 0.7776626239079347247 ) ) ;
#8762 = ORIENTED_EDGE ( 'NONE', *, *, #21447, .F. ) ;
#8763 = EDGE_CURVE ( 'NONE', #35910, #14467, #2024, .T. ) ;
#8764 = ORIENTED_EDGE ( 'NONE', *, *, #41268, .F. ) ;
#8765 = CARTESIAN_POINT ( 'NONE',  ( 3.009276887026298031, 39.20946620154573736, -1.210121013456480599 ) ) ;
#8766 = CARTESIAN_POINT ( 'NONE',  ( 2.972890788444304988, 110.6400929099055332, 3.409217096083849263 ) ) ;
#8767 =( LENGTH_UNIT ( ) NAMED_UNIT ( * ) SI_UNIT ( .MILLI., .METRE. ) );
#8768 = CARTESIAN_POINT ( 'NONE',  ( -16.24447748055638385, 147.7868695473139553, 0.9462090312511077794 ) ) ;
#8769 = DIRECTION ( 'NONE',  ( -1.000000000000000000, 0.000000000000000000, 0.000000000000000000 ) ) ;
#8770 =( BOUNDED_CURVE ( )  B_SPLINE_CURVE ( 3, ( #36657, #37076, #40692, #1303 ),
 .UNSPECIFIED., .F., .T. ) 
 B_SPLINE_CURVE_WITH_KNOTS ( ( 4, 4 ),
 ( 0.5508374472049354376, 0.6038647612415126709 ),
 .UNSPECIFIED. ) 
 CURVE ( )  GEOMETRIC_REPRESENTATION_ITEM ( )  RATIONAL_B_SPLINE_CURVE ( ( 0.8173257794870510962, 0.7610001515862588883, 0.7121729131092952025, 0.6708440640561601498 ) ) 
 REPRESENTATION_ITEM ( '' )  );
#8771 = CARTESIAN_POINT ( 'NONE',  ( 3.513860297840244673, -13.27766151250851756, 2.382095677556017588 ) ) ;
#8772 = CARTESIAN_POINT ( 'NONE',  ( 16.98902716506006882, 149.6223975874448229, -1.623990461445592892 ) ) ;
#8773 = CARTESIAN_POINT ( 'NONE',  ( -8.895965109948988925, 157.0267672960688969, -2.032209471265452816 ) ) ;
#8774 = CARTESIAN_POINT ( 'NONE',  ( -18.01920641645601151, 83.84822824455466161, 1.269999999999995799 ) ) ;
#8775 = CARTESIAN_POINT ( 'NONE',  ( -11.03183784343237583, 128.0124916018596650, -0.2204423744267033636 ) ) ;
#8776 = CARTESIAN_POINT ( 'NONE',  ( -6.203946039754976383, 30.82792567283054552, 2.070158528702760403 ) ) ;
#8777 = CARTESIAN_POINT ( 'NONE',  ( 11.48476400923499341, 128.2561452373498980, -0.2810130423614016770 ) ) ;
#8778 = ORIENTED_EDGE ( 'NONE', *, *, #9517, .F. ) ;
#8779 = CARTESIAN_POINT ( 'NONE',  ( 3.130567944924658175, -14.75736435017342707, 3.480214150758962788 ) ) ;
#8780 = FACE_OUTER_BOUND ( 'NONE', #37266, .T. ) ;
#8781 = AXIS2_PLACEMENT_3D ( 'NONE', #15840, #25230, #38654 ) ;
#8782 = VECTOR ( 'NONE', #8436, 999.9999999999998863 ) ;
#8783 = CARTESIAN_POINT ( 'NONE',  ( 6.113380087472956159E-17, 0.6350000000000001199, 0.000000000000000000 ) ) ;
#8784 = CARTESIAN_POINT ( 'NONE',  ( -56.60409974985236659, 4.028981045520047211, 2.444348447023971804 ) ) ;
#8785 = CARTESIAN_POINT ( 'NONE',  ( -2.900346660479264482, -2.445871450894649968, -3.618988008572288972 ) ) ;
#8786 = CARTESIAN_POINT ( 'NONE',  ( 16.40533521683933316, 148.4304801786341272, 1.905158959863711310 ) ) ;
#8787 = CARTESIAN_POINT ( 'NONE',  ( -6.552838421881942555E-14, 85.18346620154574111, 1.207165459533130484E-19 ) ) ;
#8788 = CARTESIAN_POINT ( 'NONE',  ( -0.1065646865916158176, 105.8844662015456919, 5.332932678536313809 ) ) ;
#8789 = CARTESIAN_POINT ( 'NONE',  ( -3.832284926465886254, -5.753926550059754064, 2.584458424559757272 ) ) ;
#8790 = CARTESIAN_POINT ( 'NONE',  ( 0.6407465451153555591, 156.3034662015456888, 0.04018040219424109244 ) ) ;
#8791 = CARTESIAN_POINT ( 'NONE',  ( -7.766292583485225443, -1.596223907437250844, -3.263082884517814364 ) ) ;
#8792 = CARTESIAN_POINT ( 'NONE',  ( -57.22211421646275653, 1.778355698664441098, -1.009576694067165286E-14 ) ) ;
#8793 = CARTESIAN_POINT ( 'NONE',  ( -5.502499940525628297, 117.0098869289899142, -0.6785148692947098326 ) ) ;
#8794 = CARTESIAN_POINT ( 'NONE',  ( 0.07931638298543132459, 106.1822392402443143, -5.212590348647615279 ) ) ;
#8795 = CARTESIAN_POINT ( 'NONE',  ( -6.505112547751767921E-14, 75.78546620154573077, -1.207165459009924652E-19 ) ) ;
#8796 = CARTESIAN_POINT ( 'NONE',  ( -1.386537629721184883, 36.36735770096321829, 2.585368322340788172 ) ) ;
#8797 = CARTESIAN_POINT ( 'NONE',  ( -1.648064503646425649, 29.87956589480163316, -4.325937074807028715 ) ) ;
#8798 = CARTESIAN_POINT ( 'NONE',  ( 1.083433792273709839, 117.9394488523357580, 1.391098255892824653 ) ) ;
#8799 = DIRECTION ( 'NONE',  ( -0.8745520943968243532, 0.4849315768086547296, -5.361993529360573944E-16 ) ) ;
#8800 = CYLINDRICAL_SURFACE ( 'NONE', #16099, 2.540000000000000480 ) ;
#8801 = CARTESIAN_POINT ( 'NONE',  ( 0.3981704103449270060, 123.4679809879532542, -0.1459118279324086442 ) ) ;
#8802 = CARTESIAN_POINT ( 'NONE',  ( -16.66487874612770881, 155.2617138006751532, 0.3247879035468689835 ) ) ;
#8803 = ORIENTED_EDGE ( 'NONE', *, *, #27463, .T. ) ;
#8804 = CIRCLE ( 'NONE', #37349, 0.6350000000000014522 ) ;
#8805 = AXIS2_PLACEMENT_3D ( 'NONE', #41342, #25348, #28544 ) ;
#8806 = VERTEX_POINT ( 'NONE', #41585 ) ;
#8807 = CARTESIAN_POINT ( 'NONE',  ( -41.52577271625990818, 22.97115911878781702, -1.524000000000015564 ) ) ;
#8808 = CARTESIAN_POINT ( 'NONE',  ( -4.211726112319180260, 155.8650792863299159, -0.03635988582397711028 ) ) ;
#8809 = CARTESIAN_POINT ( 'NONE',  ( 3.194259428633707376, -15.59200274161393018, 5.439406988142795107 ) ) ;
#8810 = CARTESIAN_POINT ( 'NONE',  ( -18.27466214341559336, 151.8090458617612057, 1.628071726616033610 ) ) ;
#8811 = CARTESIAN_POINT ( 'NONE',  ( 18.64118049546047118, 128.6297099747515347, -0.9949054493987050662 ) ) ;
#8812 = CARTESIAN_POINT ( 'NONE',  ( 4.573446973487649281, 17.56025517495590904, -0.6989348988664985107 ) ) ;
#8813 = CARTESIAN_POINT ( 'NONE',  ( -22.58226468115107011, 150.6256779753201158, -0.9011697351191819694 ) ) ;
#8814 = CARTESIAN_POINT ( 'NONE',  ( -56.33726422335487172, 4.582392934301856791, -2.601884677528782497 ) ) ;
#8815 = EDGE_LOOP ( 'NONE', ( #17494, #40207, #15298, #31342 ) ) ;
#8816 = CARTESIAN_POINT ( 'NONE',  ( 8.790925543711857415, 117.7045849823074946, 0.3245846052679721705 ) ) ;
#8817 = LINE ( 'NONE', #28612, #15472 ) ;
#8818 = CARTESIAN_POINT ( 'NONE',  ( -5.120154531940317000, 120.2090573957402455, 0.7231840875875846786 ) ) ;
#8819 = CARTESIAN_POINT ( 'NONE',  ( -48.37723337351298625, 18.71554189175216010, -5.186504670261411043 ) ) ;
#8820 = CARTESIAN_POINT ( 'NONE',  ( 2.359155998022406830, 118.9063233352275972, -0.7056007782052503563 ) ) ;
#8821 = CARTESIAN_POINT ( 'NONE',  ( -14.79112219052239752, 123.2524255416106342, -1.763561952744265859 ) ) ;
#8822 = CARTESIAN_POINT ( 'NONE',  ( -56.21344593158320180, 5.939860726778031896, -2.828251681716873911 ) ) ;
#8823 = CARTESIAN_POINT ( 'NONE',  ( 6.503815726751999371, 121.4942169270607053, -0.3795357812798487163 ) ) ;
#8824 = ORIENTED_EDGE ( 'NONE', *, *, #5103, .F. ) ;
#8825 = CARTESIAN_POINT ( 'NONE',  ( -13.94976549039478186, 152.5802402909829425, -2.190326936676450398 ) ) ;
#8826 = CARTESIAN_POINT ( 'NONE',  ( 4.296659151754357531, -15.58794764271442901, 2.529927869898711545 ) ) ;
#8827 = CARTESIAN_POINT ( 'NONE',  ( -4.254363289858590136, 118.2238500054434382, -0.4591314105454073480 ) ) ;
#8828 = CARTESIAN_POINT ( 'NONE',  ( -58.83227707057486811, -0.08366279997995551554, -0.2458995907045101459 ) ) ;
#8829 = CIRCLE ( 'NONE', #16297, 0.2539999999999992819 ) ;
#8830 = CARTESIAN_POINT ( 'NONE',  ( -4.812647089374579856, 117.4736139279835072, 1.001469096630185796 ) ) ;
#8831 = CARTESIAN_POINT ( 'NONE',  ( 0.8526219981721140373, 157.1001331247151143, 1.466586365881669574 ) ) ;
#8832 = CARTESIAN_POINT ( 'NONE',  ( -5.010144981628188887, 117.3993855238222608, -0.7522679339500687457 ) ) ;
#8833 = CARTESIAN_POINT ( 'NONE',  ( -8.332721659230562850, 3.087680552427906733, 1.359589815967415127 ) ) ;
#8834 = CARTESIAN_POINT ( 'NONE',  ( 0.6512579105864789719, 156.3106852680424765, 0.2006220687487344223 ) ) ;
#8835 = CARTESIAN_POINT ( 'NONE',  ( -57.24023649071029496, 3.661034843983918208, -2.195083147259570211 ) ) ;
#8837 = ORIENTED_EDGE ( 'NONE', *, *, #5633, .T. ) ;
#8836 = LINE ( 'NONE', #30982, #35612 ) ;
#8838 = CARTESIAN_POINT ( 'NONE',  ( -0.4424955508668900750, 117.9394511451274781, 1.393115402039464268 ) ) ;
#8839 = CARTESIAN_POINT ( 'NONE',  ( -57.83637253161431602, 2.237724655402451024, 1.757929103219288747 ) ) ;
#8840 = CARTESIAN_POINT ( 'NONE',  ( -7.948460536704424761, 121.7397034463535874, -1.077183805330166999 ) ) ;
#8841 = CARTESIAN_POINT ( 'NONE',  ( -5.241362157049125337, 65.30181249999998272, -5.310945289804168468 ) ) ;
#8842 = CARTESIAN_POINT ( 'NONE',  ( -49.72500615219620101, 20.62299186128851858, 2.281585690523495025 ) ) ;
#8843 = CARTESIAN_POINT ( 'NONE',  ( -22.83127913370414674, 150.4067493646842593, -0.3029848903584387854 ) ) ;
#8844 = EDGE_LOOP ( 'NONE', ( #26773, #19969, #18010, #36197, #36479 ) ) ;
#8845 = CARTESIAN_POINT ( 'NONE',  ( -48.56815661899839398, 19.24492339269599839, -5.224590812749988267 ) ) ;
#8846 = CARTESIAN_POINT ( 'NONE',  ( 6.029423134339813473, 121.4446780596064315, 0.06661046868258485576 ) ) ;
#8847 = DIRECTION ( 'NONE',  ( 9.627370216492862708E-17, 1.000000000000000000, -0.000000000000000000 ) ) ;
#8848 = ORIENTED_EDGE ( 'NONE', *, *, #17811, .F. ) ;
#8849 = CARTESIAN_POINT ( 'NONE',  ( 2.147067015561635817, 115.7025572403689750, -1.628760164966848389 ) ) ;
#8850 = CARTESIAN_POINT ( 'NONE',  ( -7.046279781204644266, 122.0586610246435129, -0.2738582164285299214 ) ) ;
#8851 = CARTESIAN_POINT ( 'NONE',  ( 5.386302285778954868, -11.84411807400357475, 0.7125209553660817319 ) ) ;
#8852 = CARTESIAN_POINT ( 'NONE',  ( -21.83021172428713896, 149.6930991844618291, 1.147003836765864593 ) ) ;
#8853 = CARTESIAN_POINT ( 'NONE',  ( 5.421568387540328438, 78.92574702321223867, -5.165409981420356011 ) ) ;
#8854 = CARTESIAN_POINT ( 'NONE',  ( 11.65197432296780278, 118.7334002725740874, 0.4428703322330642123 ) ) ;
#8855 = CARTESIAN_POINT ( 'NONE',  ( 13.58953805363860745, 150.2515523695257116, 0.3364537918566254393 ) ) ;
#8856 = CARTESIAN_POINT ( 'NONE',  ( -6.639407854763120941E-14, 101.6934662015457320, 3.307182826377456566E-30 ) ) ;
#8857 = CARTESIAN_POINT ( 'NONE',  ( -0.8176680875534481086, 23.83313504737664346, 0.5327793711180701663 ) ) ;
#8858 = CARTESIAN_POINT ( 'NONE',  ( -3.295257134497992180, 159.4684106755469202, -0.1128235000732132204 ) ) ;
#8859 = CARTESIAN_POINT ( 'NONE',  ( -23.91048590848665967, 81.84235438443283783, 1.269999999999992912 ) ) ;
#8860 = CIRCLE ( 'NONE', #25183, 0.5080000000000002292 ) ;
#8861 = FACE_OUTER_BOUND ( 'NONE', #30503, .T. ) ;
#8862 = ORIENTED_EDGE ( 'NONE', *, *, #39176, .T. ) ;
#8863 = CARTESIAN_POINT ( 'NONE',  ( -8.425645715861348251, 119.6231226099808254, 1.083608480663881490 ) ) ;
#8864 = CARTESIAN_POINT ( 'NONE',  ( 10.92199999999999704, 17.14499999999999957, 5.850485014536587995E-17 ) ) ;
#8865 = CARTESIAN_POINT ( 'NONE',  ( 2.066728864738883953, 117.5043770775735510, 0.6257643424168405355 ) ) ;
#8866 = CARTESIAN_POINT ( 'NONE',  ( 12.87447296688122300, 155.3440856034525837, -1.681555337288024754 ) ) ;
#8867 = CARTESIAN_POINT ( 'NONE',  ( 4.581731014592691054, -15.30239759458089388, -0.5121113081912510578 ) ) ;
#8868 = CARTESIAN_POINT ( 'NONE',  ( -20.05503673871689685, 132.0867704272472452, -1.718978086785434733 ) ) ;
#8869 = CARTESIAN_POINT ( 'NONE',  ( 4.805319368223364584, 117.6713915772949974, -0.9245024293283279349 ) ) ;
#8870 = CARTESIAN_POINT ( 'NONE',  ( 2.913298842129254496, 107.8271213589905386, 4.473571949258134950 ) ) ;
#8871 = CARTESIAN_POINT ( 'NONE',  ( -15.79043079689205697, 145.9231181611787918, -0.08479106802855317093 ) ) ;
#8872 = CARTESIAN_POINT ( 'NONE',  ( -18.85642017384699898, 148.8558894138562039, -2.490767737705128049 ) ) ;
#8873 = CARTESIAN_POINT ( 'NONE',  ( 6.347728850385006005, -14.18411723689298753, 0.2678442101147658905 ) ) ;
#8874 = CARTESIAN_POINT ( 'NONE',  ( -10.57002714855771508, 82.40335727708655611, -1.269999999999999130 ) ) ;
#8875 = AXIS2_PLACEMENT_3D ( 'NONE', #4745, #1753, #8553 ) ;
#8876 = CARTESIAN_POINT ( 'NONE',  ( -45.67973391888839529, 25.66060799623228661, -1.524000000000008237 ) ) ;
#8877 = ORIENTED_EDGE ( 'NONE', *, *, #19024, .T. ) ;
#8878 = CARTESIAN_POINT ( 'NONE',  ( 14.78649082109369672, 128.5561590274816126, 2.111834004041170498 ) ) ;
#8879 = DIRECTION ( 'NONE',  ( -5.188838149069472160E-16, 1.699382548006136559E-16, 1.000000000000000000 ) ) ;
#8880 = DIRECTION ( 'NONE',  ( -1.000000000000000000, 1.365923996832131856E-16, 0.000000000000000000 ) ) ;
#8881 = CARTESIAN_POINT ( 'NONE',  ( -3.159661387648548647, 123.6198120039584154, 0.01957516827081343461 ) ) ;
#8882 = CARTESIAN_POINT ( 'NONE',  ( -2.078203845413400863, -12.60517393744602721, -8.197436486331740824 ) ) ;
#8883 = CARTESIAN_POINT ( 'NONE',  ( 8.116318325016090185, 154.6259123219959690, 0.9857874811295551654 ) ) ;
#8884 = CARTESIAN_POINT ( 'NONE',  ( -5.012889280905649336, 115.6909491485453003, -1.400213983655213212 ) ) ;
#8885 = CARTESIAN_POINT ( 'NONE',  ( 22.56840570087976872, 150.3096427868838987, -0.3971349512683050031 ) ) ;
#8886 = CARTESIAN_POINT ( 'NONE',  ( 5.256643466843669010, 57.15000000000020464, -5.296410794270209443 ) ) ;
#8887 = CARTESIAN_POINT ( 'NONE',  ( -58.05778227315403228, 0.3792031317013907499, 0.7797940327017545137 ) ) ;
#8888 = CARTESIAN_POINT ( 'NONE',  ( -8.793333135444262538, 117.6964036462294274, -0.2880565789670351817 ) ) ;
#8889 = VECTOR ( 'NONE', #34605, 1000.000000000000000 ) ;
#8890 = FACE_OUTER_BOUND ( 'NONE', #13042, .T. ) ;
#8891 = DIRECTION ( 'NONE',  ( 5.188838149069472160E-16, -1.699382548006136559E-16, -1.000000000000000000 ) ) ;
#8892 = DIRECTION ( 'NONE',  ( 5.188838149069472160E-16, -1.699382548006136559E-16, -1.000000000000000000 ) ) ;
#8893 = ORIENTED_EDGE ( 'NONE', *, *, #33827, .T. ) ;
#8894 = CARTESIAN_POINT ( 'NONE',  ( -48.16508968810062896, 19.01313136326716347, 5.219744232931976313 ) ) ;
#8895 = CARTESIAN_POINT ( 'NONE',  ( 8.213282778328196088, 120.6581456215331372, -1.077642949125763083 ) ) ;
#8896 = CARTESIAN_POINT ( 'NONE',  ( -4.171990346301578612, 104.6144662015457385, -4.124402238216698713 ) ) ;
#8897 = CARTESIAN_POINT ( 'NONE',  ( -14.94204527009774175, 148.8997249754567349, -1.137790122619589228 ) ) ;
#8898 = DIRECTION ( 'NONE',  ( 0.7548010569845180484, 0.6559537821943359770, 0.000000000000000000 ) ) ;
#8899 = CIRCLE ( 'NONE', #1443, 8.794749999999996959 ) ;
#8900 = CARTESIAN_POINT ( 'NONE',  ( -6.439570805302779653E-14, 116.4254662015457313, -3.894619736530179447E-17 ) ) ;
#8901 = ADVANCED_FACE ( 'NONE', ( #2189 ), #9198, .F. ) ;
#8902 = ORIENTED_EDGE ( 'NONE', *, *, #2707, .T. ) ;
#8903 = CARTESIAN_POINT ( 'NONE',  ( -2.201963191602333225, 30.07953629247752758, -4.075912811544394998 ) ) ;
#8904 = CARTESIAN_POINT ( 'NONE',  ( -7.213960532363670630, 78.77618639008812806, 1.904999999999999583 ) ) ;
#8905 = DIRECTION ( 'NONE',  ( 0.8745520943968240202, -0.4849315768086553402, 6.829619984160650158E-16 ) ) ;
#8906 = CARTESIAN_POINT ( 'NONE',  ( -3.174366308152013705, 104.6144662015457243, -0.06343139340882732180 ) ) ;
#8907 = DIRECTION ( 'NONE',  ( -0.8745520943968245753, 0.4849315768086539524, -5.691349986800526185E-16 ) ) ;
#8908 = CARTESIAN_POINT ( 'NONE',  ( -6.994445320580605419, 121.9510454495767817, -0.1010066434573844985 ) ) ;
#8909 = CARTESIAN_POINT ( 'NONE',  ( 0.4006815055314143503, 20.64345356492705719, 4.603752038498275745 ) ) ;
#8910 = CARTESIAN_POINT ( 'NONE',  ( 22.81419135200704673, 148.8343141121478652, 1.537101565576850959 ) ) ;
#8911 = DIRECTION ( 'NONE',  ( -0.8745520943968361216, 0.4849315768086333023, -6.829619984160648185E-16 ) ) ;
#8913 = CARTESIAN_POINT ( 'NONE',  ( 20.90199038452897184, 141.6159226613069109, -1.473829418026497029 ) ) ;
#8912 = CARTESIAN_POINT ( 'NONE',  ( 3.216763585201820153, -14.58149021785123978, 2.832987347109013676 ) ) ;
#8914 = CARTESIAN_POINT ( 'NONE',  ( -5.874384117068585098, 120.0568572605186546, 0.8667843538975030793 ) ) ;
#8915 = CARTESIAN_POINT ( 'NONE',  ( -4.628372119175923949, 18.04465247731148381, -0.2036312542868722320 ) ) ;
#8916 = CARTESIAN_POINT ( 'NONE',  ( -22.92073667220936883, 148.8788797244430384, -1.430292205038964815 ) ) ;
#8917 = CARTESIAN_POINT ( 'NONE',  ( -0.6014681082635296994, -0.5174402789662015945, 0.7683055774679631300 ) ) ;
#8918 = ORIENTED_EDGE ( 'NONE', *, *, #1409, .T. ) ;
#8919 = EDGE_CURVE ( 'NONE', #1690, #24097, #8829, .T. ) ;
#8920 = CARTESIAN_POINT ( 'NONE',  ( -55.00324375927522169, 6.200002331679180578, 1.420877854375688587 ) ) ;
#8921 = CARTESIAN_POINT ( 'NONE',  ( -9.260187833317626627, 153.8817031120973411, 0.3320757922997039646 ) ) ;
#8922 = CARTESIAN_POINT ( 'NONE',  ( 2.095434763668091005, -15.29852786734210746, 5.959135360315205077 ) ) ;
#8923 = CARTESIAN_POINT ( 'NONE',  ( 16.74402619291549144, 146.1290494286844819, -1.112937342747913672 ) ) ;
#8924 = EDGE_LOOP ( 'NONE', ( #40682, #36696, #8300, #35309, #19220, #16470, #28126, #39116, #40558 ) ) ;
#8925 = CARTESIAN_POINT ( 'NONE',  ( 2.413036817438981352, 115.7029552731866886, 1.699863360245213117 ) ) ;
#8926 = CARTESIAN_POINT ( 'NONE',  ( -4.807653879508299255, 117.8307963401735776, -0.8997078521567819509 ) ) ;
#8927 = CARTESIAN_POINT ( 'NONE',  ( 15.78437780952694069, 146.2378312303354448, 0.3154094333657936899 ) ) ;
#8928 = ORIENTED_EDGE ( 'NONE', *, *, #27889, .F. ) ;
#8929 = CARTESIAN_POINT ( 'NONE',  ( 12.54651694896164749, 122.2722385251898771, 1.803108555445325445 ) ) ;
#8930 = CARTESIAN_POINT ( 'NONE',  ( 5.959810334499592521, 155.3892724211786742, 0.1190911940436167188 ) ) ;
#8931 = DIRECTION ( 'NONE',  ( -0.8745520943968240202, 0.4849315768086553402, -5.361993529360572958E-16 ) ) ;
#8932 = EDGE_CURVE ( 'NONE', #17444, #1544, #41157, .T. ) ;
#8933 = CARTESIAN_POINT ( 'NONE',  ( 4.992456132208793029, 117.4692012670405319, -0.8003051716943823113 ) ) ;
#8934 = CARTESIAN_POINT ( 'NONE',  ( 16.05353943441293296, 121.3766923467913585, -0.004207837007976880303 ) ) ;
#8935 = ADVANCED_FACE ( 'NONE', ( #8780 ), #28367, .T. ) ;
#8936 = CARTESIAN_POINT ( 'NONE',  ( -5.224239234539626686, 57.14999999999513136, -5.327449267724884585 ) ) ;
#8937 = CIRCLE ( 'NONE', #13710, 5.588000000000006295 ) ;
#8938 = CARTESIAN_POINT ( 'NONE',  ( -46.94614764229907422, 25.08748753966319001, 1.921268435158901999 ) ) ;
#8939 = CARTESIAN_POINT ( 'NONE',  ( -46.81215924274956564, 25.79096025118141711, 0.6894041771338947910 ) ) ;
#8940 = EDGE_CURVE ( 'NONE', #4233, #30281, #12393, .T. ) ;
#8941 = CARTESIAN_POINT ( 'NONE',  ( 1.826821012229639996, -15.37444383369212986, 5.378835944469607888 ) ) ;
#8942 = CARTESIAN_POINT ( 'NONE',  ( -46.91604881613255174, 25.30076613767161220, 1.786867259277511666 ) ) ;
#8943 = DIRECTION ( 'NONE',  ( -5.206863593109713661E-17, 1.000000000000000000, -1.077750396879097183E-30 ) ) ;
#8944 = CARTESIAN_POINT ( 'NONE',  ( -4.680719045354315710, 117.9631509934803972, 0.7257729203454069689 ) ) ;
#8945 = VERTEX_POINT ( 'NONE', #25381 ) ;
#8946 = CARTESIAN_POINT ( 'NONE',  ( -17.14499999999999957, 71.11999999999999034, 5.016499999999999737 ) ) ;
#8947 = CARTESIAN_POINT ( 'NONE',  ( 8.462540607029417572, 119.4400513420865906, -1.051277921553159356 ) ) ;
#8948 = CARTESIAN_POINT ( 'NONE',  ( -5.090087584497108075, 118.2545999410811106, -0.7183934583778603944 ) ) ;
#8949 = CARTESIAN_POINT ( 'NONE',  ( 4.794056055625289581, 117.6746627338869047, 1.099109741275124952 ) ) ;
#8950 = AXIS2_PLACEMENT_3D ( 'NONE', #24794, #21578, #14780 ) ;
#8951 = CARTESIAN_POINT ( 'NONE',  ( 2.233078627056604759, -15.14192004606506536, 5.083345892419886880 ) ) ;
#8952 = CARTESIAN_POINT ( 'NONE',  ( -0.1041500444720373508, 106.1822392402443143, 5.212094112990285133 ) ) ;
#8953 = CARTESIAN_POINT ( 'NONE',  ( -3.178183004559932190, -7.902942162671289239, -3.366045245292264010 ) ) ;
#8954 = CARTESIAN_POINT ( 'NONE',  ( -50.15972161391663064, 17.13814111569222121, 4.955022299345066550 ) ) ;
#8955 = CARTESIAN_POINT ( 'NONE',  ( -29.82321757229076908, 71.17901112636586447, -1.270000000000007123 ) ) ;
#8956 = CARTESIAN_POINT ( 'NONE',  ( 4.405468973772799224, 113.1344509532474376, -2.291157639236350185 ) ) ;
#8957 = CARTESIAN_POINT ( 'NONE',  ( -10.57849499609994304, 123.4307455932968765, -1.421577474458307400 ) ) ;
#8958 = CARTESIAN_POINT ( 'NONE',  ( 6.997680356709169658, 121.9559740633448115, 0.1243954239949175838 ) ) ;
#8959 = DIRECTION ( 'NONE',  ( 0.1548479172700143736, -0.9876883405951387696, -0.02222305941043778779 ) ) ;
#8960 = CARTESIAN_POINT ( 'NONE',  ( -1.944923406237783814, 115.7029431175197658, 1.643877071207305418 ) ) ;
#8961 = CARTESIAN_POINT ( 'NONE',  ( -3.158589313471108273, 4.191505055319899142, 3.400481138232230194 ) ) ;
#8963 = ORIENTED_EDGE ( 'NONE', *, *, #40501, .T. ) ;
#8962 = CARTESIAN_POINT ( 'NONE',  ( 11.50728102546029064, 118.8226552325407397, 0.6924515317502046852 ) ) ;
#8964 = CARTESIAN_POINT ( 'NONE',  ( 1.773712854446913623, 104.6144662015413758, -5.033492136046540111 ) ) ;
#8965 = CARTESIAN_POINT ( 'NONE',  ( 3.297442402085044133, -15.64565814434701352, 4.209479195861737466 ) ) ;
#8966 = CARTESIAN_POINT ( 'NONE',  ( -17.85428843624176665, 135.5811125208551857, 1.719929978336786514 ) ) ;
#8967 = CARTESIAN_POINT ( 'NONE',  ( 0.7510871189337386955, -11.68616409646884158, 0.6196617644748384501 ) ) ;
#8968 = AXIS2_PLACEMENT_3D ( 'NONE', #3517, #25855, #3728 ) ;
#8969 = CARTESIAN_POINT ( 'NONE',  ( 0.1178611003048646577, 6.342877585758503578, 0.9680126135609015137 ) ) ;
#8970 = VERTEX_POINT ( 'NONE', #11963 ) ;
#8971 = CIRCLE ( 'NONE', #10903, 0.5080000000000000071 ) ;
#8972 = ORIENTED_EDGE ( 'NONE', *, *, #27922, .F. ) ;
#8973 = CARTESIAN_POINT ( 'NONE',  ( -8.095114962461808616, 74.19100168833409725, 1.270000000000002460 ) ) ;
#8974 = CARTESIAN_POINT ( 'NONE',  ( 4.531575537551966626, 119.7344140837147819, 0.5249638875923486880 ) ) ;
#8975 = CARTESIAN_POINT ( 'NONE',  ( -5.884536728138022532, 121.1554468101848130, 0.4284271420130267849 ) ) ;
#8976 = CARTESIAN_POINT ( 'NONE',  ( -6.559134203278485842, 78.24119908707510263, -1.523999999999996469 ) ) ;
#8977 = CARTESIAN_POINT ( 'NONE',  ( 3.449548791184131602, -12.83738641323306595, 1.613555780903996206 ) ) ;
#8978 = CARTESIAN_POINT ( 'NONE',  ( 5.108784305046350838, 120.0747842884402132, -0.7604166522187120192 ) ) ;
#8979 = CARTESIAN_POINT ( 'NONE',  ( -19.69933843609255675, 149.7343351798865285, -2.455316921491699222 ) ) ;
#8980 = CARTESIAN_POINT ( 'NONE',  ( 12.21488373879589417, 55.24500000000000455, -5.016499999999999737 ) ) ;
#8981 = CARTESIAN_POINT ( 'NONE',  ( 3.131015516031846690, -14.62848841321586946, 3.524024012273756501 ) ) ;
#8982 = CARTESIAN_POINT ( 'NONE',  ( -0.05411207418350773291, 38.74323431000957640, 0.9275608492890762280 ) ) ;
#8983 = CARTESIAN_POINT ( 'NONE',  ( 15.82110658236419631, 145.7390459690742830, -0.1389873312028085395 ) ) ;
#8984 = EDGE_CURVE ( 'NONE', #39579, #20685, #13596, .T. ) ;
#8985 = ORIENTED_EDGE ( 'NONE', *, *, #14121, .T. ) ;
#8986 = CARTESIAN_POINT ( 'NONE',  ( -10.53334313995851801, 65.32054992887103140, -1.523999999999996469 ) ) ;
#8987 = FACE_OUTER_BOUND ( 'NONE', #37407, .T. ) ;
#8988 = ADVANCED_FACE ( 'NONE', ( #7990 ), #31981, .T. ) ;
#8989 = CARTESIAN_POINT ( 'NONE',  ( 4.968851538487103703, 117.5943734491196722, 0.8206492525603533705 ) ) ;
#8990 = CARTESIAN_POINT ( 'NONE',  ( -58.82991071597915322, -0.2577532384647474029, -1.205395329641216235E-14 ) ) ;
#8991 = CARTESIAN_POINT ( 'NONE',  ( 8.327223946240280839, 23.24253473731531727, -1.329248712143314748 ) ) ;
#8992 = CARTESIAN_POINT ( 'NONE',  ( 6.627928625996522882, 155.5185402614932570, 1.342408143365148021 ) ) ;
#8993 = DIRECTION ( 'NONE',  ( 6.353134868986659519E-16, -1.000000000000000000, 0.000000000000000000 ) ) ;
#8994 = CARTESIAN_POINT ( 'NONE',  ( 22.98549031890215844, 150.1594536303649932, 0.4336790679505427293 ) ) ;
#8995 = CARTESIAN_POINT ( 'NONE',  ( -4.812383263389278021, 112.7966860322829206, 2.369499567760593450 ) ) ;
#8996 = B_SPLINE_CURVE_WITH_KNOTS ( 'NONE', 3,
 ( #1879, #5293, #34048, #41062, #5087, #40853, #34258, #11656, #11873, #14842, #21858, #14634, #18242, #5498, #3091 ),
 .UNSPECIFIED., .F., .F.,
 ( 4, 2, 2, 2, 1, 2, 2, 4 ),
 ( 0.000000000000000000, 0.06249999999999900080, 0.1249999999999978906, 0.2499999999999956701, 0.2812499999999951150, 0.3749999999999934497, 0.4374999999999933387, 0.5000000000000000000 ),
 .UNSPECIFIED. ) ;
#8997 = AXIS2_PLACEMENT_3D ( 'NONE', #11352, #37342, #8161 ) ;
#8998 = ADVANCED_FACE ( 'NONE', ( #33981 ), #32634, .F. ) ;
#8999 = CARTESIAN_POINT ( 'NONE',  ( -1.504723661876595786, -8.552649586842417051, -4.374500482163298898 ) ) ;
#9000 = CARTESIAN_POINT ( 'NONE',  ( 5.959810334499592521, 155.3892724211786742, 0.1190911940436167188 ) ) ;
#9001 = CARTESIAN_POINT ( 'NONE',  ( 7.688107727944508696, 4.450669244509953160, -3.435853896805545649 ) ) ;
#9002 = CARTESIAN_POINT ( 'NONE',  ( -2.150834356787523660, 116.6630246571967575, -0.4597420995432478508 ) ) ;
#9003 = CARTESIAN_POINT ( 'NONE',  ( 0.01635612298154385039, 119.2343925067225427, -0.8185272769043290264 ) ) ;
#9004 = CARTESIAN_POINT ( 'NONE',  ( -36.98328822617348521, 27.82293856516311692, -1.270000000000003793 ) ) ;
#9005 = EDGE_CURVE ( 'NONE', #37389, #41900, #39453, .T. ) ;
#9006 = DIRECTION ( 'NONE',  ( 0.6878275643682715268, 0.7258741224862691466, 2.626171355423258178E-14 ) ) ;
#9007 = CARTESIAN_POINT ( 'NONE',  ( -8.092465427151658730, -6.292564624861634037, 2.510960718618908238 ) ) ;
#9008 = CARTESIAN_POINT ( 'NONE',  ( 0.07507557030359549022, 117.9394488564931009, 1.409405562719200811 ) ) ;
#9009 = CARTESIAN_POINT ( 'NONE',  ( -10.34239276132902674, 65.15305678602257444, 1.270000000000002016 ) ) ;
#9010 = CARTESIAN_POINT ( 'NONE',  ( -17.14499999999999957, 71.11999999999999034, 5.016499999999999737 ) ) ;
#9011 = CARTESIAN_POINT ( 'NONE',  ( 0.7690845662405288996, 119.7070660435176279, -0.6575911349602956424 ) ) ;
#9012 = CARTESIAN_POINT ( 'NONE',  ( -7.924482676426956473, 158.6683511845044734, 0.3722227806660352578 ) ) ;
#9013 = AXIS2_PLACEMENT_3D ( 'NONE', #8787, #5812, #21961 ) ;
#9014 = ORIENTED_EDGE ( 'NONE', *, *, #28731, .F. ) ;
#9015 = CARTESIAN_POINT ( 'NONE',  ( -58.57480556029605623, 0.6052348492003173375, -0.1017111358178830471 ) ) ;
#9016 =( BOUNDED_CURVE ( )  B_SPLINE_CURVE ( 3, ( #3685, #19422, #26455, #17070 ),
 .UNSPECIFIED., .F., .F. ) 
 B_SPLINE_CURVE_WITH_KNOTS ( ( 4, 4 ),
 ( 0.7252176650374851929, 0.9253411388830656836 ),
 .UNSPECIFIED. ) 
 CURVE ( )  GEOMETRIC_REPRESENTATION_ITEM ( )  RATIONAL_B_SPLINE_CURVE ( ( 0.5049133130095756483, 0.4784625025417720279, 0.5588101048313269814, 0.7459561198782403979 ) ) 
 REPRESENTATION_ITEM ( '' )  );
#9017 = ORIENTED_EDGE ( 'NONE', *, *, #20410, .F. ) ;
#9018 = CARTESIAN_POINT ( 'NONE',  ( -42.60041433329272564, 22.17261999083454072, -1.881317670890401361 ) ) ;
#9019 = CARTESIAN_POINT ( 'NONE',  ( -9.100602120603912937, 153.9557227532744150, -0.1238295526561323939 ) ) ;
#9020 = CARTESIAN_POINT ( 'NONE',  ( 6.478224611219328466, -13.79365725417489053, 0.02984861787792387686 ) ) ;
#9021 = CARTESIAN_POINT ( 'NONE',  ( -19.44243145639594061, 150.5708382285403388, 1.622132703307645807 ) ) ;
#9022 = CARTESIAN_POINT ( 'NONE',  ( 2.057861540686706459, 117.3535355059730705, -0.5007145131239726377 ) ) ;
#9023 = CARTESIAN_POINT ( 'NONE',  ( 2.003160574663116034, 15.61121511114846960, 4.187759092076685619 ) ) ;
#9024 = CARTESIAN_POINT ( 'NONE',  ( -15.09710430809812642, 156.1437908837410191, -0.6951944926208389886 ) ) ;
#9025 = CARTESIAN_POINT ( 'NONE',  ( -58.16583728925170504, 0.7033174012466524294, -1.177358567970812508 ) ) ;
#9026 = ORIENTED_EDGE ( 'NONE', *, *, #14841, .F. ) ;
#9027 = FACE_OUTER_BOUND ( 'NONE', #6994, .T. ) ;
#9028 = CARTESIAN_POINT ( 'NONE',  ( 13.85159022459153988, 12.96416000000000146, -5.016499999999999737 ) ) ;
#9029 = CARTESIAN_POINT ( 'NONE',  ( -13.47719143446468948, 152.3772590505219569, 1.474657383304484259 ) ) ;
#9030 = CARTESIAN_POINT ( 'NONE',  ( 1.925929944387235853E-31, 3.469446951953614189E-15, 0.000000000000000000 ) ) ;
#9031 = CARTESIAN_POINT ( 'NONE',  ( 13.98553986197810062, 125.7699432187419575, -1.444593012458400105 ) ) ;
#9032 = CARTESIAN_POINT ( 'NONE',  ( -4.922209265113230536, 118.1424809852657773, -0.9875327093606014461 ) ) ;
#9033 = CARTESIAN_POINT ( 'NONE',  ( -57.09878488423309051, 3.216020309495956742, -2.217633722229552351 ) ) ;
#9034 = CIRCLE ( 'NONE', #24669, 4.826000000000001400 ) ;
#9035 = B_SPLINE_CURVE_WITH_KNOTS ( 'NONE', 3,
 ( #21401, #37620, #28024, #21201, #8443, #28242 ),
 .UNSPECIFIED., .F., .F.,
 ( 4, 2, 4 ),
 ( 0.000000000000000000, 0.0002825957426950183467, 0.0005651914853900366935 ),
 .UNSPECIFIED. ) ;
#9036 = CARTESIAN_POINT ( 'NONE',  ( 5.888833980634776921, 121.2452591720019370, -0.3608419296047722380 ) ) ;
#9037 = CARTESIAN_POINT ( 'NONE',  ( -17.78478073489628031, 148.4245508482893854, -2.330447787059697795 ) ) ;
#9038 = CARTESIAN_POINT ( 'NONE',  ( 3.431757876926103012, -15.17734022545018391, 2.935651181724953318 ) ) ;
#9039 = CARTESIAN_POINT ( 'NONE',  ( -4.065972646788793554, 118.2429491485453070, -0.3080848862740693250 ) ) ;
#9040 = CARTESIAN_POINT ( 'NONE',  ( -58.73801720703743001, -0.4998429216807459552, -1.049519136981926467E-14 ) ) ;
#9041 = CARTESIAN_POINT ( 'NONE',  ( -4.793595683501052918, 117.7335357436302559, 0.8914022784051079951 ) ) ;
#9042 = CARTESIAN_POINT ( 'NONE',  ( 3.724242145611105670, 156.8112981010400802, 1.651639321868204613 ) ) ;
#9043 = CARTESIAN_POINT ( 'NONE',  ( -47.26619606798132622, 24.98193397792429593, 1.785901896324509019 ) ) ;
#9044 = ADVANCED_FACE ( 'NONE', ( #35187 ), #7475, .T. ) ;
#9045 = CARTESIAN_POINT ( 'NONE',  ( 0.1224881284885083327, 5.266211660758980173, 8.431793989537572642 ) ) ;
#9046 = CARTESIAN_POINT ( 'NONE',  ( 4.292261259499645654, 155.8363458669846864, 0.4108933393057505601 ) ) ;
#9047 = CARTESIAN_POINT ( 'NONE',  ( -32.51099854767154085, 68.28336360077705081, -1.270000000000008233 ) ) ;
#9048 = ADVANCED_FACE ( 'NONE', ( #8987 ), #30561, .T. ) ;
#9050 = ORIENTED_EDGE ( 'NONE', *, *, #19791, .T. ) ;
#9049 = CARTESIAN_POINT ( 'NONE',  ( -41.33672448130794663, 22.78954268934618810, -1.170983984347497842 ) ) ;
#9051 = CARTESIAN_POINT ( 'NONE',  ( -0.5175973550576450366, 118.1588899065644966, 0.8875034609994335577 ) ) ;
#9052 = CARTESIAN_POINT ( 'NONE',  ( -58.70413935429054675, 0.2332485698458008905, 0.6626129746612759996 ) ) ;
#9053 = CARTESIAN_POINT ( 'NONE',  ( -49.98362463941607814, 16.32256260904422618, 4.928702286786347919 ) ) ;
#9054 = CARTESIAN_POINT ( 'NONE',  ( -7.851552067626940357, 122.2419137942978864, -0.7720006874763839511 ) ) ;
#9055 = VECTOR ( 'NONE', #39192, 1000.000000000000000 ) ;
#9056 = CARTESIAN_POINT ( 'NONE',  ( 6.113380087472956159E-17, 0.6350000000000001199, 0.000000000000000000 ) ) ;
#9057 = CARTESIAN_POINT ( 'NONE',  ( -52.41299847468118855, 17.00754718993399095, 1.481513115354232024 ) ) ;
#9058 = CARTESIAN_POINT ( 'NONE',  ( -16.84917212821883581, 155.2300590059875844, -0.1976545469556808265 ) ) ;
#9059 = EDGE_LOOP ( 'NONE', ( #15896, #6491, #22265, #36267 ) ) ;
#9060 = CARTESIAN_POINT ( 'NONE',  ( -51.38196307026375820, 20.99359797579823805, -1.083509735914620812E-14 ) ) ;
#9061 = CARTESIAN_POINT ( 'NONE',  ( -6.015894240732284182, 121.4385361577320595, -0.1720725319338911041 ) ) ;
#9062 = CARTESIAN_POINT ( 'NONE',  ( -7.878666962121352313, 122.2304107671814251, 0.4668939114535545221 ) ) ;
#9063 = VERTEX_POINT ( 'NONE', #15778 ) ;
#9064 = CARTESIAN_POINT ( 'NONE',  ( 1.895611262766748295, 115.7029491485453434, -1.647518854579561820 ) ) ;
#9065 = CARTESIAN_POINT ( 'NONE',  ( 0.001255909994487175050, 120.9722815239556439, -0.06285087176068875070 ) ) ;
#9066 = CARTESIAN_POINT ( 'NONE',  ( 5.009217890960311337, -13.99182267686448178, 3.873128360714999552 ) ) ;
#9067 = CARTESIAN_POINT ( 'NONE',  ( -20.26345141861418142, 136.2683111393718320, 1.346723181737012665 ) ) ;
#9068 = CARTESIAN_POINT ( 'NONE',  ( 4.792324638223571576, 56.51998046905274009, -4.972049999999996750 ) ) ;
#9069 = VECTOR ( 'NONE', #12504, 1000.000000000000000 ) ;
#9070 = CARTESIAN_POINT ( 'NONE',  ( 0.3042230016542175619, 116.5226405152084652, 0.1306790058978156699 ) ) ;
#9071 = CARTESIAN_POINT ( 'NONE',  ( 15.19842606723472400, 143.4031501637221879, 0.4388155327730876021 ) ) ;
#9072 = CARTESIAN_POINT ( 'NONE',  ( -10.18297664959815663, 77.66688486464208552, -1.269999999999998019 ) ) ;
#9073 = CARTESIAN_POINT ( 'NONE',  ( 0.2560056206704328097, 6.564126901726701213, 0.9442708342526761056 ) ) ;
#9074 = CARTESIAN_POINT ( 'NONE',  ( -15.69471450241215571, 120.8333755831694702, -0.3643268586347850335 ) ) ;
#9075 = DIRECTION ( 'NONE',  ( 1.000000000000000000, 0.000000000000000000, -4.553079989440420948E-16 ) ) ;
#9076 = CARTESIAN_POINT ( 'NONE',  ( -5.152689475313444234, 116.8412042432202185, -0.1029630068797482562 ) ) ;
#9077 = ORIENTED_EDGE ( 'NONE', *, *, #15470, .T. ) ;
#9078 = CARTESIAN_POINT ( 'NONE',  ( -8.651804384430541006, 118.4863469498705797, 0.7357695435087184821 ) ) ;
#9079 = DIRECTION ( 'NONE',  ( 0.7517731442105912709, -0.6594218222380281436, 8.537024980200781389E-16 ) ) ;
#9080 = CARTESIAN_POINT ( 'NONE',  ( 20.19347568108150526, 136.2683111393718320, 2.155148867324337747 ) ) ;
#9081 = CARTESIAN_POINT ( 'NONE',  ( 14.15994444794823259, 154.3735777161816429, -1.715400944796409144 ) ) ;
#9082 = CARTESIAN_POINT ( 'NONE',  ( -2.276242205911199523, 25.81146128161704567, -8.137376054096339573 ) ) ;
#9083 = CARTESIAN_POINT ( 'NONE',  ( -22.02091170609381976, 149.7938220333360846, -1.879853634988783329 ) ) ;
#9084 = CARTESIAN_POINT ( 'NONE',  ( 4.811064755782845204, 117.8746741567870373, -0.6667383956446522042 ) ) ;
#9085 = CARTESIAN_POINT ( 'NONE',  ( 5.281229466409561368, 116.7000894413872629, 1.021210189368793486 ) ) ;
#9086 = CARTESIAN_POINT ( 'NONE',  ( -15.53315888837599168, 147.5314071815517138, -0.1823436108899490204 ) ) ;
#9087 = CARTESIAN_POINT ( 'NONE',  ( -18.07722773961213747, 140.6071502257508143, -2.476399831607924096 ) ) ;
#9088 = CARTESIAN_POINT ( 'NONE',  ( 6.311525104866394287, -14.07095602924590594, 0.9561848504773229340 ) ) ;
#9089 = AXIS2_PLACEMENT_3D ( 'NONE', #37920, #21494, #8743 ) ;
#9090 = FACE_BOUND ( 'NONE', #33686, .T. ) ;
#9091 = B_SPLINE_CURVE_WITH_KNOTS ( 'NONE', 3,
 ( #24923, #37921, #2993, #35355, #35781, #39181, #9574, #38555, #6, #218, #15953, #9368, #19154, #5980, #35572, #6595, #13193, #3625, #22544, #6390, #22332, #18943, #25965, #28949 ),
 .UNSPECIFIED., .F., .F.,
 ( 4, 2, 2, 2, 2, 2, 2, 2, 2, 2, 2, 4 ),
 ( 0.0006020626168661550497, 0.003690437786238830956, 0.006778812955611506971, 0.008323000540297826114, 0.009095094332641003032, 0.009867188124984181685, 0.01063928191732735860, 0.01141137570967053552, 0.01218346950201371418, 0.01256951639818529483, 0.01276253984627108429, 0.01295556329435687375 ),
 .UNSPECIFIED. ) ;
#9092 = CARTESIAN_POINT ( 'NONE',  ( -0.9909088102708097923, 117.3993836601271568, -1.479711866447754876 ) ) ;
#9093 = CIRCLE ( 'NONE', #26072, 0.5080000000000002292 ) ;
#9094 = ORIENTED_EDGE ( 'NONE', *, *, #39789, .T. ) ;
#9095 = CARTESIAN_POINT ( 'NONE',  ( 0.9451225546579952175, 157.6350123088122359, 1.628263479412583870 ) ) ;
#9096 = CARTESIAN_POINT ( 'NONE',  ( -4.854024325513706550, 118.7629491485453599, 0.1807258574060142675 ) ) ;
#9097 = CIRCLE ( 'NONE', #18600, 3.175000000000001155 ) ;
#9098 = CARTESIAN_POINT ( 'NONE',  ( -2.578112510118048206, 120.6526784328644339, 0.3421008684282442203 ) ) ;
#9099 = CARTESIAN_POINT ( 'NONE',  ( 0.6424836204703546771, -8.070646579680392563, 8.395564330620057802 ) ) ;
#9100 = CARTESIAN_POINT ( 'NONE',  ( 11.72694347678944915, 128.3321206738457647, 0.9702521317530999889 ) ) ;
#9101 = EDGE_CURVE ( 'NONE', #514, #25107, #41489, .T. ) ;
#9102 = CARTESIAN_POINT ( 'NONE',  ( 22.74771312706160131, 149.7444054411783441, -0.5134062617908412562 ) ) ;
#9103 = CARTESIAN_POINT ( 'NONE',  ( 4.825814575782076510, 56.51499999999999346, -4.829586058641568869 ) ) ;
#9104 = AXIS2_PLACEMENT_3D ( 'NONE', #6583, #13390, #36194 ) ;
#9105 = CARTESIAN_POINT ( 'NONE',  ( -58.29828225616458326, -0.1403253391138825912, 0.3417568066585683906 ) ) ;
#9106 = CARTESIAN_POINT ( 'NONE',  ( -19.33375693323417011, 80.42273151551299293, -1.270000000000003570 ) ) ;
#9107 = CARTESIAN_POINT ( 'NONE',  ( -5.570375128628924699, 56.51499999999999346, 4.419987129958256489 ) ) ;
#9108 = CARTESIAN_POINT ( 'NONE',  ( 4.875296837154728280, 115.9539249584174314, -1.177764552249251917 ) ) ;
#9109 = VERTEX_POINT ( 'NONE', #16405 ) ;
#9110 = CARTESIAN_POINT ( 'NONE',  ( -4.362246989847086809, 119.4897582430469498, -0.9267953991463255825 ) ) ;
#9112 = CARTESIAN_POINT ( 'NONE',  ( 4.141126571459865069, 104.6144662015457243, 4.161112031276615220 ) ) ;
#9111 = APPLICATION_CONTEXT ( 'automotive_design' ) ;
#9113 = AXIS2_PLACEMENT_3D ( 'NONE', #30282, #37729, #17293 ) ;
#9114 = CARTESIAN_POINT ( 'NONE',  ( -9.577010982344122070, 124.1734284925964573, -0.7139017932201209282 ) ) ;
#9115 = CARTESIAN_POINT ( 'NONE',  ( -28.99017888265885645, 62.64366196043476265, 1.523999999999993138 ) ) ;
#9116 = CARTESIAN_POINT ( 'NONE',  ( 13.43845804798103316, 156.9141898299356512, 0.2685323735513602261 ) ) ;
#9117 = EDGE_LOOP ( 'NONE', ( #17167, #36828, #12871, #22664, #29614, #34122, #12514, #38042 ) ) ;
#9118 = CARTESIAN_POINT ( 'NONE',  ( -1.756104463947763206, 14.33678105357426702, 4.288642365192034234 ) ) ;
#9119 = CARTESIAN_POINT ( 'NONE',  ( -30.15519950990045217, 69.97033940222175374, 1.523999999999994914 ) ) ;
#9120 = CARTESIAN_POINT ( 'NONE',  ( -4.828962989263914984, 117.4049964369462060, 1.009641684917192306 ) ) ;
#9121 = CARTESIAN_POINT ( 'NONE',  ( -5.008948584507881385, 27.92152162925472325, 0.4889012661100834434 ) ) ;
#9122 = AXIS2_PLACEMENT_3D ( 'NONE', #4776, #33945, #14534 ) ;
#9123 = DIRECTION ( 'NONE',  ( 0.01997839162482749689, 1.040247600000945640E-18, -0.9998004120163610509 ) ) ;
#9124 = CARTESIAN_POINT ( 'NONE',  ( 7.784332241379921413, 122.6279634482064154, 0.1742627236427056192 ) ) ;
#9125 = CARTESIAN_POINT ( 'NONE',  ( 3.308978306493741250, 24.09187545982852541, -3.235542752117448018 ) ) ;
#9126 = CARTESIAN_POINT ( 'NONE',  ( 13.03166249679904354, 119.8917521002241955, 1.045815086349644929 ) ) ;
#9127 = CARTESIAN_POINT ( 'NONE',  ( -4.074141608589817665, 104.6144662015457669, -2.607666899705321395 ) ) ;
#9129 = CARTESIAN_POINT ( 'NONE',  ( 21.19479858968361796, 149.1058327099893290, -1.460163390594824806 ) ) ;
#9128 = CARTESIAN_POINT ( 'NONE',  ( -14.80692295515835255, 78.04183178746349370, 5.016499999999999737 ) ) ;
#9130 = CARTESIAN_POINT ( 'NONE',  ( -11.45258232062230697, 123.1738952066917534, 1.204891439250160623 ) ) ;
#9131 = CARTESIAN_POINT ( 'NONE',  ( 2.264360804680111805, 21.29314879275315064, 4.027482774281332389 ) ) ;
#9132 = CARTESIAN_POINT ( 'NONE',  ( -11.33669861507968157, 118.9804978796424706, -0.9069902030348426791 ) ) ;
#9133 = AXIS2_PLACEMENT_3D ( 'NONE', #13322, #39318, #35282 ) ;
#9134 = CARTESIAN_POINT ( 'NONE',  ( 0.6271221672387817803, 4.229989959315594739, -0.7487545302041328510 ) ) ;
#9135 = ORIENTED_EDGE ( 'NONE', *, *, #37081, .T. ) ;
#9136 = CARTESIAN_POINT ( 'NONE',  ( -55.14069116334857767, 5.401725095812811794, 0.2259897844577825055 ) ) ;
#9137 = CARTESIAN_POINT ( 'NONE',  ( -15.96529520877018626, 145.8030804522035737, 0.4114451159501718580 ) ) ;
#9138 = CARTESIAN_POINT ( 'NONE',  ( 5.061152751093137780, -13.25450807444039647, 3.067510535416694495 ) ) ;
#9139 = CARTESIAN_POINT ( 'NONE',  ( 15.84185526851198489, 139.7295799824062499, -1.277977597745375560 ) ) ;
#9140 = CIRCLE ( 'NONE', #32953, 5.588000000000006295 ) ;
#9141 = DIRECTION ( 'NONE',  ( 4.017660918040594346E-17, -1.000000000000000000, -2.376309959284834438E-19 ) ) ;
#9142 = CARTESIAN_POINT ( 'NONE',  ( -4.820638971607948520, 117.6752190542308227, -1.075962066314599008 ) ) ;
#9143 = CARTESIAN_POINT ( 'NONE',  ( 8.487687333566158898, 123.3253871723413368, 0.1696041924978712867 ) ) ;
#9144 = VERTEX_POINT ( 'NONE', #33041 ) ;
#9145 = CARTESIAN_POINT ( 'NONE',  ( 13.17434061382155441, 122.5785676075921060, 1.825321299320728397 ) ) ;
#9146 = CARTESIAN_POINT ( 'NONE',  ( 10.39928917620358817, 153.1223395828141918, 0.2078025466733119664 ) ) ;
#9147 = DIRECTION ( 'NONE',  ( -0.7548010569845216011, -0.6559537821943317581, -2.801824109679580762E-16 ) ) ;
#9148 = EDGE_CURVE ( 'NONE', #27418, #36699, #22389, .T. ) ;
#9149 = CARTESIAN_POINT ( 'NONE',  ( 4.828127062081292387, 117.4060377263907213, -1.008211717711906541 ) ) ;
#9150 = CARTESIAN_POINT ( 'NONE',  ( 16.78241155767104331, 155.2615993841311877, -0.07296080027729302808 ) ) ;
#9151 = PLANE ( 'NONE',  #22684 ) ;
#9152 = CARTESIAN_POINT ( 'NONE',  ( -46.85193236286590945, 25.57103397218990182, 1.585296040148151286 ) ) ;
#9153 = CARTESIAN_POINT ( 'NONE',  ( -46.72388148998840762, 26.09838203902186393, -8.130785423271672580E-15 ) ) ;
#9154 = CARTESIAN_POINT ( 'NONE',  ( 1.912964346608580835, -15.38803350473924603, 5.361940315677870217 ) ) ;
#9155 = CARTESIAN_POINT ( 'NONE',  ( -43.24646561529713296, 21.63922848039483071, 2.381786957946262273 ) ) ;
#9156 = CARTESIAN_POINT ( 'NONE',  ( -6.059261036834474368, 56.51499999999998636, -4.381499999999999950 ) ) ;
#9157 = EDGE_CURVE ( 'NONE', #31300, #18130, #25811, .T. ) ;
#9158 = CARTESIAN_POINT ( 'NONE',  ( -4.625240786758006095, 118.0596839624423495, 0.5387667837598054676 ) ) ;
#9159 = ORIENTED_EDGE ( 'NONE', *, *, #20134, .F. ) ;
#9160 = VERTEX_POINT ( 'NONE', #26423 ) ;
#9161 = CARTESIAN_POINT ( 'NONE',  ( -1.378789611427061912, 115.6909491485452577, -1.738307004888806961 ) ) ;
#9162 = CARTESIAN_POINT ( 'NONE',  ( 3.566060519644585369, 118.7008415277600903, -0.7946426777497477278 ) ) ;
#9163 = CARTESIAN_POINT ( 'NONE',  ( -4.979866836074960723, 117.8491495069952748, -0.7948704875671745995 ) ) ;
#9164 = CARTESIAN_POINT ( 'NONE',  ( 4.648305118706619332, 118.0133915895967931, 0.7935454642018273663 ) ) ;
#9165 = CARTESIAN_POINT ( 'NONE',  ( -54.78025980062105305, 10.68576047822487141, -1.034243702897348038E-14 ) ) ;
#9166 = CARTESIAN_POINT ( 'NONE',  ( -0.2562694446383195213, 108.5751225745497806, 4.260274975123000019 ) ) ;
#9167 = PRESENTATION_STYLE_ASSIGNMENT (( #18942 ) ) ;
#9168 = LINE ( 'NONE', #22124, #19660 ) ;
#9169 = DIRECTION ( 'NONE',  ( 5.188838149069472160E-16, -1.699382548006136559E-16, -1.000000000000000000 ) ) ;
#9170 = CARTESIAN_POINT ( 'NONE',  ( 0.1065646865914871566, 105.8844662015456777, -5.332932678536312032 ) ) ;
#9171 = CARTESIAN_POINT ( 'NONE',  ( -10.79132569999989144, 123.6843197456346672, -1.443847663909934242 ) ) ;
#9172 = CARTESIAN_POINT ( 'NONE',  ( -3.702526914408131642, 33.15860816321391979, 4.132160499251987140 ) ) ;
#9173 = CARTESIAN_POINT ( 'NONE',  ( -2.103092518242876796, 115.7026983564594644, 1.632052075412017134 ) ) ;
#9174 = CARTESIAN_POINT ( 'NONE',  ( 4.636458409304901274, 17.36039413176390411, -0.09481320587925551324 ) ) ;
#9176 = EDGE_LOOP ( 'NONE', ( #14854, #40929, #14912, #35893, #16485 ) ) ;
#9175 = CARTESIAN_POINT ( 'NONE',  ( 16.79208607122037833, 122.6968688451475771, 0.8807046615161950864 ) ) ;
#9177 = CARTESIAN_POINT ( 'NONE',  ( 3.700855694654260564, 104.6144662015545208, -3.857327698788455717 ) ) ;
#9178 = CARTESIAN_POINT ( 'NONE',  ( 3.184821769958268600, -15.26663968290864482, 3.758507235160873261 ) ) ;
#9179 = CARTESIAN_POINT ( 'NONE',  ( -5.043395383124352982, 119.2220797256985350, 0.8992592568097313999 ) ) ;
#9180 = CARTESIAN_POINT ( 'NONE',  ( 0.9697834966998255535, 21.94565095173003400, 0.09096683575692042500 ) ) ;
#9181 = CARTESIAN_POINT ( 'NONE',  ( -0.5327793704965378963, 2.243135046448306191, -0.8176680881360027797 ) ) ;
#9182 = EDGE_CURVE ( 'NONE', #23570, #11667, #6128, .T. ) ;
#9183 = EDGE_LOOP ( 'NONE', ( #17530, #5853, #23490, #30392 ) ) ;
#9184 = ORIENTED_EDGE ( 'NONE', *, *, #15618, .T. ) ;
#9185 = LINE ( 'NONE', #34749, #37843 ) ;
#9186 = CARTESIAN_POINT ( 'NONE',  ( 3.197921176416294919, 118.4615047536228047, 0.7906167528392611388 ) ) ;
#9187 = CARTESIAN_POINT ( 'NONE',  ( -13.84625834149343326, 134.3516747369166069, 0.8047173373260270157 ) ) ;
#9188 = LINE ( 'NONE', #12166, #36822 ) ;
#9189 = CARTESIAN_POINT ( 'NONE',  ( 3.107604131292615257, -12.52806217606054773, 0.6782401946156415562 ) ) ;
#9190 = CARTESIAN_POINT ( 'NONE',  ( 10.06933303711900507, 122.3915136462027817, -1.070338282017660791 ) ) ;
#9191 = CARTESIAN_POINT ( 'NONE',  ( -17.37713502592725590, 151.5007859583534753, -2.430116715062250243 ) ) ;
#9192 = LINE ( 'NONE', #5799, #21534 ) ;
#9193 = CARTESIAN_POINT ( 'NONE',  ( 7.931513209474629456, 121.8264860997418140, 1.035788693698372676 ) ) ;
#9194 = CARTESIAN_POINT ( 'NONE',  ( 4.122826845240182614, 118.2429491485453354, -0.1811473218594779611 ) ) ;
#9195 = CARTESIAN_POINT ( 'NONE',  ( 15.76950829013769351, 146.9135488020124001, -0.01503653553346920996 ) ) ;
#9196 = ORIENTED_EDGE ( 'NONE', *, *, #40122, .T. ) ;
#9197 = CARTESIAN_POINT ( 'NONE',  ( 0.1066086480732678088, 105.8844037013956410, -5.332931792593708309 ) ) ;
#9198 = PLANE ( 'NONE',  #30594 ) ;
#9199 = CYLINDRICAL_SURFACE ( 'NONE', #26574, 0.2539999999999998925 ) ;
#9200 = CARTESIAN_POINT ( 'NONE',  ( -13.76130258807007678, 16.83823567964706314, 5.016499999999998849 ) ) ;
#9201 = CARTESIAN_POINT ( 'NONE',  ( -7.300781474974964880, 17.39199087320084658, -4.267473507878162486 ) ) ;
#9202 = CARTESIAN_POINT ( 'NONE',  ( 12.92681072397279074, 152.2092440956282076, 1.775214794609845548 ) ) ;
#9203 = CARTESIAN_POINT ( 'NONE',  ( -17.14499999999999957, 71.11999999999999034, 5.016499999999999737 ) ) ;
#9204 = CARTESIAN_POINT ( 'NONE',  ( 18.63485108555815373, 154.1203422869290023, 0.3484461891417475754 ) ) ;
#9205 = B_SPLINE_CURVE_WITH_KNOTS ( 'NONE', 3,
 ( #29685, #10085, #16257, #26489, #944, #26703, #106, #3934, #20284, #36303, #3511, #33312, #19454 ),
 .UNSPECIFIED., .F., .F.,
 ( 4, 1, 1, 1, 1, 1, 1, 1, 1, 1, 4 ),
 ( 0.000000000000000000, 0.1250000000000002498, 0.2500000000000004996, 0.3750000000000000555, 0.4109712969816595729, 0.4999999999999996669, 0.6249999999999995559, 0.7500000000000001110, 0.8232913890944979496, 0.8750000000000001110, 1.000000000000000000 ),
 .UNSPECIFIED. ) ;
#9206 = CARTESIAN_POINT ( 'NONE',  ( -7.450817465826296448, 123.6645382909113664, -0.1143006167400526935 ) ) ;
#9207 = CARTESIAN_POINT ( 'NONE',  ( -2.070226828232369254, -8.352695179381779411, -4.151654383260235726 ) ) ;
#9208 = CARTESIAN_POINT ( 'NONE',  ( 8.935197197525127422, 123.9063447689825779, 0.1785465045940572426 ) ) ;
#9209 = EDGE_CURVE ( 'NONE', #38242, #32125, #25582, .T. ) ;
#9210 = CARTESIAN_POINT ( 'NONE',  ( 11.72614449088015043, 156.4111399680655552, 2.003450915338490734 ) ) ;
#9211 = PRESENTATION_LAYER_ASSIGNMENT (  '', '', ( #2412 ) ) ;
#9212 = CARTESIAN_POINT ( 'NONE',  ( 0.8732425085435751022, -3.549726780817298977, -8.398906084147368389 ) ) ;
#9213 = CARTESIAN_POINT ( 'NONE',  ( -2.190167605149390351, 116.8639141099391452, -0.5450301620853724716 ) ) ;
#9214 = CARTESIAN_POINT ( 'NONE',  ( 0.02135216056670925094, 118.1497763966934258, -1.068549427312529554 ) ) ;
#9215 = DIRECTION ( 'NONE',  ( -4.017660918040594346E-17, 1.000000000000000000, 2.376309959284834438E-19 ) ) ;
#9216 = DIRECTION ( 'NONE',  ( 5.188838149069472160E-16, -1.699382548006136559E-16, -1.000000000000000000 ) ) ;
#9217 = CARTESIAN_POINT ( 'NONE',  ( 2.598967704003971146, -9.625211180298204994, -8.041545772114961466 ) ) ;
#9218 = CARTESIAN_POINT ( 'NONE',  ( 0.4816777417134468497, 118.1588880427148212, 0.9074776130548274367 ) ) ;
#9219 = CYLINDRICAL_SURFACE ( 'NONE', #23944, 6.349999999999999645 ) ;
#9220 = CARTESIAN_POINT ( 'NONE',  ( 2.766857707386623400, -13.29092698609396450, 0.4080254275553683585 ) ) ;
#9221 = CARTESIAN_POINT ( 'NONE',  ( 0.3095834102097976270, 110.3683645023726427, -3.577238406694227546 ) ) ;
#9222 = CARTESIAN_POINT ( 'NONE',  ( -18.19405586666668739, 125.1529741258727597, 0.3179404471852275704 ) ) ;
#9223 = ORIENTED_EDGE ( 'NONE', *, *, #23245, .T. ) ;
#9224 = EDGE_CURVE ( 'NONE', #1883, #37954, #10180, .T. ) ;
#9225 = CARTESIAN_POINT ( 'NONE',  ( 5.664977208693820820, 53.58606249999999704, 5.033228321271210781 ) ) ;
#9226 = EDGE_LOOP ( 'NONE', ( #39033, #15868, #33796, #5140 ) ) ;
#9227 = CARTESIAN_POINT ( 'NONE',  ( -5.078986093043185157, 75.27746620154573520, -0.1014902294541231847 ) ) ;
#9228 = CARTESIAN_POINT ( 'NONE',  ( 3.628834229889370544, -15.44114452258853198, 5.288308529986511353 ) ) ;
#9229 = CARTESIAN_POINT ( 'NONE',  ( -4.979196860906144551, 118.3881331334009985, 0.8414419690753370817 ) ) ;
#9230 = CARTESIAN_POINT ( 'NONE',  ( 22.14298845881043221, 148.3267584643486146, -1.148356825654135438 ) ) ;
#9231 = CARTESIAN_POINT ( 'NONE',  ( -3.998286381996895233, 3.741657206818807424, 2.332027183294827832 ) ) ;
#9232 = CARTESIAN_POINT ( 'NONE',  ( -55.72094646625244252, 5.847107909200485842, -2.941330550160955681 ) ) ;
#9233 = ORIENTED_EDGE ( 'NONE', *, *, #26102, .T. ) ;
#9234 = CARTESIAN_POINT ( 'NONE',  ( -58.31893842775842529, -0.1844529990628340776, -0.2851935484599126269 ) ) ;
#9235 = DIRECTION ( 'NONE',  ( 1.011795553208986377E-16, 1.000000000000000000, -0.000000000000000000 ) ) ;
#9236 = FACE_OUTER_BOUND ( 'NONE', #33251, .T. ) ;
#9237 = B_SPLINE_SURFACE_WITH_KNOTS ( 'NONE', 3, 3, ( 
 ( #22009, #41426, #32251, #35040, #2663, #3081, #38647, #16040, #42061, #3503, #309, #3927, #13908, #23050, #32669, #29679, #3715 ),
 ( #13279, #39913, #17094, #26263, #10291, #10706, #23903, #23685, #10914, #522, #36706, #19653, #16887, #40120, #36296, #29888, #16462 ),
 ( #13495, #30097, #726, #938, #16674, #23473, #23261, #29469, #39702, #10502, #7116, #20074, #39273, #10079, #4135, #36084, #7527 ),
 ( #13701, #33515, #33096, #39485, #6898, #36498, #20488, #26695, #7318, #6686, #19868, #26900, #1143, #4349, #17311, #32883, #20278 ),
 ( #26481, #33305, #30300, #14110, #27108, #31141, #37123, #24115, #4553, #17717, #33730, #27944, #18346, #11757, #24745, #4765, #17928 ),
 ( #21117, #37747, #8571, #24526, #11128, #8356, #34143, #30933, #14942, #1568, #24324, #21532, #1772, #40745, #33937, #11542, #2195 ),
 ( #40952, #30511, #4970, #7945, #30716, #14732, #18136, #11969, #14524, #15153, #34564, #5391, #20914, #1351, #27734, #31352, #28157 ),
 ( #20704, #27321, #41163, #36920, #27534, #7738, #37531, #8146, #17513, #21324, #1980, #14308, #40541, #40334, #11336, #34352, #37330 ) ),
 .UNSPECIFIED., .F., .F., .F.,
 ( 4, 1, 2, 1, 4 ),
 ( 4, 1, 1, 1, 1, 1, 1, 1, 1, 1, 1, 1, 1, 1, 4 ),
 ( 0.000000000000000000, 0.2500000000000000000, 0.4999999999999996669, 0.7500000000000000000, 1.000000000000000000 ),
 ( 0.000000000000000000, 0.08300113939718137268, 0.1732806554784933895, 0.2717672377176819087, 0.3752096606209606167, 0.4787223716043260135, 0.5772295444745598747, 0.6668133826162351285, 0.7470991451079272982, 0.7815930070524458317, 0.8169452614683294644, 0.8547689062991584708, 0.8968063284581728745, 0.9447228702782888288, 1.000000000000000000 ),
 .UNSPECIFIED. ) ;
#9238 = CARTESIAN_POINT ( 'NONE',  ( -13.27577938203614316, 128.5100244389050204, 1.209575533060950114 ) ) ;
#9239 = DIRECTION ( 'NONE',  ( -0.9963102427714440879, 0.000000000000000000, 0.08582482245076958338 ) ) ;
#9240 = ADVANCED_FACE ( 'NONE', ( #3869 ), #38589, .F. ) ;
#9241 = CARTESIAN_POINT ( 'NONE',  ( 0.03212616895145502249, 157.6269964811067155, -1.607724863813388971 ) ) ;
#9242 = CARTESIAN_POINT ( 'NONE',  ( -21.07518769967747119, 148.4376209648218321, -2.358402543220755820 ) ) ;
#9243 = CARTESIAN_POINT ( 'NONE',  ( -52.30895062419047292, 13.66434875625866674, -4.401212925246500873 ) ) ;
#9244 = ADVANCED_FACE ( 'NONE', ( #19187 ), #22782, .T. ) ;
#9245 = CARTESIAN_POINT ( 'NONE',  ( 9.867693216206284035, 124.1914461168675530, -0.5013480754756757252 ) ) ;
#9246 = AXIS2_PLACEMENT_3D ( 'NONE', #32531, #28702, #15495 ) ;
#9247 = ORIENTED_EDGE ( 'NONE', *, *, #30525, .T. ) ;
#9248 = CARTESIAN_POINT ( 'NONE',  ( -15.61558020634891975, 150.8349565870724120, -2.213412335539846509 ) ) ;
#9249 = CARTESIAN_POINT ( 'NONE',  ( 3.525547644170144324, -15.07001638954266731, 1.996499786560847367 ) ) ;
#9250 = CARTESIAN_POINT ( 'NONE',  ( -4.233202534921607807, 118.2249641308060859, -0.4810777853349767486 ) ) ;
#9251 = DIRECTION ( 'NONE',  ( 6.353134868986659519E-16, -1.000000000000000000, 0.000000000000000000 ) ) ;
#9252 = EDGE_CURVE ( 'NONE', #36653, #5054, #9496, .T. ) ;
#9253 = CARTESIAN_POINT ( 'NONE',  ( -4.935446760104023944, 117.6551691763225875, 0.7496835391351150957 ) ) ;
#9254 = CARTESIAN_POINT ( 'NONE',  ( 16.55051581791493476, 149.4842840675632658, 2.199106316832546870 ) ) ;
#9255 = DIRECTION ( 'NONE',  ( -0.6294287539883980376, -0.7770581983690878491, -1.945484789722745799E-16 ) ) ;
#9256 = CARTESIAN_POINT ( 'NONE',  ( 8.411406395146093118, -11.38171290258811119, -0.9481482025471229536 ) ) ;
#9257 = CARTESIAN_POINT ( 'NONE',  ( 4.562414174745239137, 121.1702857069421100, 0.2029539227048861583 ) ) ;
#9258 = CARTESIAN_POINT ( 'NONE',  ( -53.00789483126595769, 12.40033530745290236, -4.180047681284821515 ) ) ;
#9260 = VERTEX_POINT ( 'NONE', #42000 ) ;
#9259 = CARTESIAN_POINT ( 'NONE',  ( -49.58053446479453186, 16.59387910164543456, -4.528212452174721570 ) ) ;
#9261 = CARTESIAN_POINT ( 'NONE',  ( -5.809227842914837403, 77.60418761620948658, -1.523999999999996025 ) ) ;
#9262 = CARTESIAN_POINT ( 'NONE',  ( -56.78650302187183740, 3.241477563879227475, 2.205756828360251109 ) ) ;
#9263 = CARTESIAN_POINT ( 'NONE',  ( -51.64658268050072820, 13.54811038370313447, 4.518953239828090496 ) ) ;
#9264 = CARTESIAN_POINT ( 'NONE',  ( -8.517743499764725001, 118.9454930948057125, -1.260829469820966553 ) ) ;
#9265 = CARTESIAN_POINT ( 'NONE',  ( -5.305748947172281405, 65.30181249999998272, -5.247078976224250013 ) ) ;
#9266 = CARTESIAN_POINT ( 'NONE',  ( -56.10358335640970751, 6.949471795635917104, 1.762666882438575611 ) ) ;
#9267 = ADVANCED_FACE ( 'NONE', ( #13438 ), #38, .F. ) ;
#9268 = CARTESIAN_POINT ( 'NONE',  ( -3.286349204026867810, 159.4678586119998442, 0.07386938312792028227 ) ) ;
#9269 = CIRCLE ( 'NONE', #33088, 0.2539999999999989488 ) ;
#9270 = EDGE_LOOP ( 'NONE', ( #84, #8091, #6251, #5672 ) ) ;
#9271 = CARTESIAN_POINT ( 'NONE',  ( -54.91040913962392978, 10.45702928859090086, -1.592171597931419491 ) ) ;
#9272 = CARTESIAN_POINT ( 'NONE',  ( -7.804241651921540956, 122.5006630351903709, -0.4842881838540384343 ) ) ;
#9273 = CARTESIAN_POINT ( 'NONE',  ( 4.901481263995191462, 117.4107946624300638, -0.9679066200967618716 ) ) ;
#9274 = ORIENTED_EDGE ( 'NONE', *, *, #877, .F. ) ;
#9275 = CARTESIAN_POINT ( 'NONE',  ( 2.448094588128645110, 115.7029487073275504, -1.604675776025721978 ) ) ;
#9276 = CARTESIAN_POINT ( 'NONE',  ( -11.10900461081884494, 128.0707465396788507, -0.3225556591789269789 ) ) ;
#9277 = CARTESIAN_POINT ( 'NONE',  ( 5.061152751093137780, -13.25450807444039647, 3.067510535416694495 ) ) ;
#9278 = CARTESIAN_POINT ( 'NONE',  ( -21.60128648486327663, 148.1022500232506616, 1.385191265705788322 ) ) ;
#9279 = CARTESIAN_POINT ( 'NONE',  ( -6.559134203278485842, 78.24119908707510263, -1.269999999999996465 ) ) ;
#9280 = CARTESIAN_POINT ( 'NONE',  ( 17.10498822929443108, 122.7072422303320707, 0.5849822763170867690 ) ) ;
#9281 = CARTESIAN_POINT ( 'NONE',  ( 6.513934358062148711, 121.7796322531078346, 0.2438456569635198967 ) ) ;
#9282 = CARTESIAN_POINT ( 'NONE',  ( 4.851371946308560723, 115.6909491485453145, -1.282097887966950900 ) ) ;
#9283 = CARTESIAN_POINT ( 'NONE',  ( 0.5069063945870452281, 6.992850521020996801, 0.8331330811856124674 ) ) ;
#9284 = CARTESIAN_POINT ( 'NONE',  ( -10.82257311662895916, 157.9086237439880733, -0.2761350859956693826 ) ) ;
#9285 = DIRECTION ( 'NONE',  ( 5.188838149069472160E-16, -1.699382548006136559E-16, -1.000000000000000000 ) ) ;
#9286 = CYLINDRICAL_SURFACE ( 'NONE', #32960, 0.2540000000000000036 ) ;
#9287 = ORIENTED_EDGE ( 'NONE', *, *, #31822, .F. ) ;
#9288 = CARTESIAN_POINT ( 'NONE',  ( 2.333515971706682013, 116.4819875861390841, 0.3626728605129332927 ) ) ;
#9289 = CARTESIAN_POINT ( 'NONE',  ( -58.36875020124374913, -0.2893854339803315634, -0.03832961079136332910 ) ) ;
#9290 = CARTESIAN_POINT ( 'NONE',  ( 4.901975893987065902, 117.8999350694477926, 0.9234475893805553781 ) ) ;
#9291 = CARTESIAN_POINT ( 'NONE',  ( 12.27107220260955067, 121.7247091083657153, -1.253333917061305147 ) ) ;
#9292 = CARTESIAN_POINT ( 'NONE',  ( -4.837940364245437941, 10.07446788996644038, 6.911991265526966188 ) ) ;
#9293 = CARTESIAN_POINT ( 'NONE',  ( -20.95410280040443496, 151.1643092826112138, -1.845047842948928540 ) ) ;
#9294 = CARTESIAN_POINT ( 'NONE',  ( 4.725550995308940294, 117.9581936019243642, -0.6734248769522227507 ) ) ;
#9295 = ADVANCED_FACE ( 'NONE', ( #13003 ), #5464, .F. ) ;
#9296 = CARTESIAN_POINT ( 'NONE',  ( 7.639005212201189998, 124.2918010433613745, 0.1615048153450350521 ) ) ;
#9297 = CARTESIAN_POINT ( 'NONE',  ( -8.831233598306610588, 123.6950213215744583, -0.09329271932673267875 ) ) ;
#9298 = CARTESIAN_POINT ( 'NONE',  ( -18.70459055478416488, 148.4604323410545987, -2.472120825861215732 ) ) ;
#9299 = CARTESIAN_POINT ( 'NONE',  ( 2.631220017305710090, -15.63525587843500553, 5.668892982663133573 ) ) ;
#9300 = DIRECTION ( 'NONE',  ( 5.188838149069472160E-16, -1.699382548006136559E-16, -1.000000000000000000 ) ) ;
#9301 = AXIS2_PLACEMENT_3D ( 'NONE', #24497, #5360, #37718 ) ;
#9302 = CARTESIAN_POINT ( 'NONE',  ( -47.11704014324645584, 20.18577099567727373, -5.127035723291441194 ) ) ;
#9304 = EDGE_LOOP ( 'NONE', ( #12848, #8918, #14565, #2645 ) ) ;
#9303 = AXIS2_PLACEMENT_3D ( 'NONE', #1146, #7742, #314 ) ;
#9305 = CARTESIAN_POINT ( 'NONE',  ( 2.387603053075636250, 119.2205458019918751, 0.7760930522211749727 ) ) ;
#9306 = CARTESIAN_POINT ( 'NONE',  ( -15.64207015331068185, 147.2204672151589193, -0.3125657877211906466 ) ) ;
#9307 = CARTESIAN_POINT ( 'NONE',  ( -46.38316532014824389, 26.05065462784537900, -1.270000000000008233 ) ) ;
#9308 = CARTESIAN_POINT ( 'NONE',  ( -2.294838902200274422, 118.2243428780609662, 0.8383363118275912740 ) ) ;
#9309 = CARTESIAN_POINT ( 'NONE',  ( -3.973931221679809056, 20.38425861574787490, -7.466160517099206473 ) ) ;
#9310 = CARTESIAN_POINT ( 'NONE',  ( 5.204851039067889040, 121.0999079655412203, 0.5006067476712320330 ) ) ;
#9311 = CARTESIAN_POINT ( 'NONE',  ( 22.52700986351711165, 149.9757045183965261, -0.6247156920787646506 ) ) ;
#9312 = CARTESIAN_POINT ( 'NONE',  ( -4.929842468146641288, 117.6425979561673785, -0.8692111560381230451 ) ) ;
#9313 = AXIS2_PLACEMENT_3D ( 'NONE', #23460, #36487, #21521 ) ;
#9314 = CARTESIAN_POINT ( 'NONE',  ( 4.659827697873120123, 112.0094687158754994, -2.672315607338379362 ) ) ;
#9315 = EDGE_LOOP ( 'NONE', ( #21764, #6215, #31541, #40724 ) ) ;
#9316 = CARTESIAN_POINT ( 'NONE',  ( 4.469912121137109118, 119.5537132673701137, -0.7488809508603075926 ) ) ;
#9317 = DIRECTION ( 'NONE',  ( 0.8745520943968235761, -0.4849315768086558398, 4.268512490100410909E-16 ) ) ;
#9318 = CARTESIAN_POINT ( 'NONE',  ( -9.078381139985740589, 123.6795089456687577, -0.5923855214342146347 ) ) ;
#9319 = CARTESIAN_POINT ( 'NONE',  ( 6.059261036834404202, 56.58343591620776181, -4.712961528314684401 ) ) ;
#9320 = CARTESIAN_POINT ( 'NONE',  ( 8.078287538471617069, 158.6595088495342338, 0.1614234102745199240 ) ) ;
#9321 = ORIENTED_EDGE ( 'NONE', *, *, #3768, .T. ) ;
#9322 = CARTESIAN_POINT ( 'NONE',  ( 2.584458374606236841, 15.83607344512877368, 3.832284875798456447 ) ) ;
#9323 = CARTESIAN_POINT ( 'NONE',  ( -28.96638701337642985, 63.08302880242272437, 1.523999999999993582 ) ) ;
#9324 = CARTESIAN_POINT ( 'NONE',  ( -4.923499976822237834, 117.4076456904317638, 0.9491661484678960425 ) ) ;
#9325 = DIRECTION ( 'NONE',  ( -5.188838149069471174E-16, 1.699382548006136313E-16, 1.000000000000000000 ) ) ;
#9326 = CIRCLE ( 'NONE', #9979, 0.2540000000000052771 ) ;
#9327 = CARTESIAN_POINT ( 'NONE',  ( -8.584014518950162653, 73.13423810798758495, 1.524000000000002686 ) ) ;
#9328 = CARTESIAN_POINT ( 'NONE',  ( 6.998514830026701716, 121.6887508624515704, 0.6757143304067796397 ) ) ;
#9329 = CARTESIAN_POINT ( 'NONE',  ( -2.961220487682185265, 16.77021669962341477, -3.573240411402743621 ) ) ;
#9330 = CARTESIAN_POINT ( 'NONE',  ( 22.55218723263367764, 148.5212373274837319, 1.758973660241909709 ) ) ;
#9331 = CARTESIAN_POINT ( 'NONE',  ( -50.55264109713811393, 15.40887103989715889, -4.805487048246964932 ) ) ;
#9333 = CARTESIAN_POINT ( 'NONE',  ( 19.85075266274209937, 150.7280352275851101, -1.521773064777484086 ) ) ;
#9332 = CARTESIAN_POINT ( 'NONE',  ( 0.4201230711237894933, 106.0157732049497241, 5.283348651899852477 ) ) ;
#9334 = CARTESIAN_POINT ( 'NONE',  ( -12.23061257473133878, 124.2599011343719155, 1.262879005329815563 ) ) ;
#9335 = CARTESIAN_POINT ( 'NONE',  ( 2.776928087254650013, 2.301956178644051221, 3.707541451904531105 ) ) ;
#9336 = CARTESIAN_POINT ( 'NONE',  ( -22.14168286312786549, 150.6715983490228723, -1.403651840795990813 ) ) ;
#9337 = ORIENTED_EDGE ( 'NONE', *, *, #34423, .T. ) ;
#9338 = CARTESIAN_POINT ( 'NONE',  ( -15.40459090795135566, 148.0444422243178337, 0.2810841713230233241 ) ) ;
#9339 = CARTESIAN_POINT ( 'NONE',  ( 4.440325138859688714, -14.57630248335078882, 4.728313687495418804 ) ) ;
#9340 = DIRECTION ( 'NONE',  ( -5.188838149069472160E-16, 1.699382548006136559E-16, 1.000000000000000000 ) ) ;
#9341 = CIRCLE ( 'NONE', #34526, 7.461249999999999716 ) ;
#9342 = CARTESIAN_POINT ( 'NONE',  ( -4.700796422664683227, 117.9670161556764896, -0.8081787690371831090 ) ) ;
#9343 = CARTESIAN_POINT ( 'NONE',  ( 8.770618086120967050, 123.6813396614493712, 0.1752578222716852097 ) ) ;
#9344 = ORIENTED_EDGE ( 'NONE', *, *, #7412, .F. ) ;
#9345 = CARTESIAN_POINT ( 'NONE',  ( 19.09066119453645172, 140.9752145814059645, 2.516632075137499314 ) ) ;
#9346 = DIRECTION ( 'NONE',  ( 5.206863593109713661E-17, -1.000000000000000000, 1.077750396879097183E-30 ) ) ;
#9347 = CYLINDRICAL_SURFACE ( 'NONE', #30704, 0.6350000000000001199 ) ;
#9348 = CARTESIAN_POINT ( 'NONE',  ( -15.30245393414170074, 121.3917326167944708, 0.5382413912410557444 ) ) ;
#9349 = CARTESIAN_POINT ( 'NONE',  ( 4.814838716269237651, 117.4047667081807305, -1.012532368900667556 ) ) ;
#9350 = VECTOR ( 'NONE', #25753, 1000.000000000000000 ) ;
#9351 = CARTESIAN_POINT ( 'NONE',  ( 18.55749356256734117, 125.2038358216989735, 0.01254332324266071129 ) ) ;
#9352 = CARTESIAN_POINT ( 'NONE',  ( -29.91360363449004822, 70.04874496952839991, 1.523999999999992250 ) ) ;
#9353 = CARTESIAN_POINT ( 'NONE',  ( 5.319550251556916187, 115.6909491485453145, -0.5107772461581731038 ) ) ;
#9354 = CARTESIAN_POINT ( 'NONE',  ( -46.69554899239189183, 26.06112269829689865, 0.4657571695567544467 ) ) ;
#9355 = CARTESIAN_POINT ( 'NONE',  ( 2.037787548254768488, -15.06252990901250932, 5.718409153091174701 ) ) ;
#9356 = CARTESIAN_POINT ( 'NONE',  ( -47.67648637180144533, 19.71513033058998232, 5.327979952964769339 ) ) ;
#9357 = CARTESIAN_POINT ( 'NONE',  ( 3.631129234170231257, -15.30172121837498445, -0.5308806197736579691 ) ) ;
#9358 = CARTESIAN_POINT ( 'NONE',  ( -4.596941264179941200, 118.0790773607558606, 0.5324384840013657305 ) ) ;
#9359 = ORIENTED_EDGE ( 'NONE', *, *, #392, .T. ) ;
#9360 = ORIENTED_EDGE ( 'NONE', *, *, #33182, .F. ) ;
#9361 = CARTESIAN_POINT ( 'NONE',  ( -0.4700442440780402964, 115.6909491485452435, -1.765047585021120469 ) ) ;
#9362 = CARTESIAN_POINT ( 'NONE',  ( -5.861813178617722109, 119.0059073072438167, -1.257136650504465658 ) ) ;
#9363 = CARTESIAN_POINT ( 'NONE',  ( -5.567295163420557635, 119.7830797108918688, -0.4963393297495871659 ) ) ;
#9364 = CARTESIAN_POINT ( 'NONE',  ( 4.641264194575597024, 117.9844048130280640, 0.8831379620347793447 ) ) ;
#9365 = DIRECTION ( 'NONE',  ( 6.353134868986659519E-16, -1.000000000000000000, 0.000000000000000000 ) ) ;
#9366 = CARTESIAN_POINT ( 'NONE',  ( -16.02795213054451651, 143.8376908863262997, -1.609587254066635165 ) ) ;
#9367 = CARTESIAN_POINT ( 'NONE',  ( -3.160447555344903403, 115.7029629790199863, -1.658213846050050622 ) ) ;
#9368 = CARTESIAN_POINT ( 'NONE',  ( -2.461970253143333842, 107.2456962212051224, 4.635069176697791171 ) ) ;
#9369 = CARTESIAN_POINT ( 'NONE',  ( -4.808149584360944750, 104.6144662015457243, 0.4147572885131461939 ) ) ;
#9370 = CARTESIAN_POINT ( 'NONE',  ( 6.497658445673516248, 120.6500652548963899, -0.1353193420278798464 ) ) ;
#9371 = CARTESIAN_POINT ( 'NONE',  ( -17.48541186233178024, 146.4615580561186050, -2.166240883089540770 ) ) ;
#9372 = DIRECTION ( 'NONE',  ( -0.9891443546370349837, 0.000000000000000000, -0.1469470846586743706 ) ) ;
#9373 = CARTESIAN_POINT ( 'NONE',  ( -0.7326219338007132764, 37.28220708697721619, 2.048504824603447627 ) ) ;
#9374 = CARTESIAN_POINT ( 'NONE',  ( -3.034780876608168754, 115.7029491485453292, 1.550823147752200315 ) ) ;
#9375 = CARTESIAN_POINT ( 'NONE',  ( 0.1710433496020407063, 14.98650505531991683, 4.637963194678765610 ) ) ;
#9377 = EDGE_LOOP ( 'NONE', ( #16271, #25100, #2920, #22073 ) ) ;
#9376 = CARTESIAN_POINT ( 'NONE',  ( 22.90231444567481489, 149.5023856264156450, 1.310353656364537045 ) ) ;
#9378 = CARTESIAN_POINT ( 'NONE',  ( 4.270515072716039029, 104.6144662015391589, -3.200693163871419333 ) ) ;
#9379 = CARTESIAN_POINT ( 'NONE',  ( 3.246941722412215459, -15.25025356868572857, 3.602141857564104210 ) ) ;
#9380 = CARTESIAN_POINT ( 'NONE',  ( -18.83801864273527471, 140.8526363637247982, 1.765582951612574503 ) ) ;
#9381 = CARTESIAN_POINT ( 'NONE',  ( 0.6271221672387817803, 4.229989959315594739, -0.7487545302041328510 ) ) ;
#9382 = CARTESIAN_POINT ( 'NONE',  ( 0.4552753346810295421, 10.21665217803766268, -0.8656630863528285147 ) ) ;
#9383 = ORIENTED_EDGE ( 'NONE', *, *, #25098, .T. ) ;
#9384 = ORIENTED_EDGE ( 'NONE', *, *, #18506, .T. ) ;
#9385 = LINE ( 'NONE', #5791, #39904 ) ;
#9386 = CARTESIAN_POINT ( 'NONE',  ( 3.231430644863403590, 118.6786177306206014, 0.7432888438146501020 ) ) ;
#9387 =( NAMED_UNIT ( * ) SI_UNIT ( $, .STERADIAN. ) SOLID_ANGLE_UNIT ( ) );
#9388 = CARTESIAN_POINT ( 'NONE',  ( -16.29799532358069669, 145.9442052555630767, 0.7927408685852875836 ) ) ;
#9389 = CARTESIAN_POINT ( 'NONE',  ( -14.95453923199683288, 61.75387968257833649, -5.016499999999999737 ) ) ;
#9390 = CARTESIAN_POINT ( 'NONE',  ( 3.187032726610941946, -14.26951854355915117, 4.096494115788091861 ) ) ;
#9391 = CARTESIAN_POINT ( 'NONE',  ( 11.15120438727540630, 123.3376105302527037, -1.132373765670515287 ) ) ;
#9392 = CARTESIAN_POINT ( 'NONE',  ( -4.110343450561661172, 118.7489093234570561, -1.002437571585374609 ) ) ;
#9393 = CARTESIAN_POINT ( 'NONE',  ( 8.537663472096003403, 118.8514694301399572, 1.229114518489605290 ) ) ;
#9394 = CARTESIAN_POINT ( 'NONE',  ( -0.1060743468339773732, 38.40290746171823599, -0.3145143346692479414 ) ) ;
#9395 = CARTESIAN_POINT ( 'NONE',  ( 14.75792966017384344, 148.8440819608433969, -0.1510343195432201913 ) ) ;
#9396 = ORIENTED_EDGE ( 'NONE', *, *, #9706, .T. ) ;
#9397 = CARTESIAN_POINT ( 'NONE',  ( -17.64290547347870941, 83.78857423953914463, -1.524000000000003130 ) ) ;
#9398 = CARTESIAN_POINT ( 'NONE',  ( -2.690315046239569075, 30.48488075981191159, 3.827843980145978264 ) ) ;
#9399 =( GEOMETRIC_REPRESENTATION_CONTEXT ( 3 ) GLOBAL_UNCERTAINTY_ASSIGNED_CONTEXT ( ( #6966 ) ) GLOBAL_UNIT_ASSIGNED_CONTEXT ( ( #37731, #25368, #30916 ) ) REPRESENTATION_CONTEXT ( 'NONE', 'WORKASPACE' ) );
#9400 = CARTESIAN_POINT ( 'NONE',  ( 5.018724313895222444, 117.3993830154766584, -0.7021450163807499978 ) ) ;
#9401 = CARTESIAN_POINT ( 'NONE',  ( -1.740095136297252543, 16.12223834230618635, -8.265420891812045312 ) ) ;
#9402 = CARTESIAN_POINT ( 'NONE',  ( 10.11490785437005435, 123.9924233945428682, 1.115122180374878091 ) ) ;
#9403 = CARTESIAN_POINT ( 'NONE',  ( 23.34374616560282689, 149.0672090665632936, 0.4407082534803009044 ) ) ;
#9404 = CARTESIAN_POINT ( 'NONE',  ( -5.300219172352997887, 116.7134249176580028, 0.8085863681920515411 ) ) ;
#9405 = CARTESIAN_POINT ( 'NONE',  ( -1.949331898794882667, 118.1189800858121117, 0.8693949517531047722 ) ) ;
#9406 = CARTESIAN_POINT ( 'NONE',  ( 4.560200836559435977, -11.68919918208664122, 0.6963878748952898601 ) ) ;
#9407 = FACE_OUTER_BOUND ( 'NONE', #31259, .T. ) ;
#9408 = CARTESIAN_POINT ( 'NONE',  ( 20.91063213905296791, 147.8517002469272370, 2.402771019925620255 ) ) ;
#9409 = CARTESIAN_POINT ( 'NONE',  ( -7.647780498939813931, -9.906183224868927439, 3.644365410659974991 ) ) ;
#9410 = CARTESIAN_POINT ( 'NONE',  ( -2.160025851330804159, 116.7207721880314324, -0.4861172116870683402 ) ) ;
#9411 = CARTESIAN_POINT ( 'NONE',  ( -0.3557992751142647903, 119.2343925067223722, -0.8259638274389486945 ) ) ;
#9412 = CARTESIAN_POINT ( 'NONE',  ( -7.842268484490568348, 73.30875693322846587, 1.270000000000002904 ) ) ;
#9413 = DIRECTION ( 'NONE',  ( -0.6294287539884013682, -0.7770581983690854067, 6.679558114607144468E-15 ) ) ;
#9414 = CARTESIAN_POINT ( 'NONE',  ( -3.947349438182777615, 105.1227439526176681, 3.603969139096321772 ) ) ;
#9415 = CARTESIAN_POINT ( 'NONE',  ( 8.369577038434204752, -11.69170392490758381, 0.7719616968112763544 ) ) ;
#9416 = DIRECTION ( 'NONE',  ( -1.000000000000000000, 0.000000000000000000, 0.000000000000000000 ) ) ;
#9417 = PLANE ( 'NONE',  #11718 ) ;
#9418 = CARTESIAN_POINT ( 'NONE',  ( 2.672745566561993247, -14.90124427853171873, 4.600530618394071070 ) ) ;
#9419 = CARTESIAN_POINT ( 'NONE',  ( 0.9965922269826466007, 107.7619142660649203, -4.530701086038176228 ) ) ;
#9420 = CARTESIAN_POINT ( 'NONE',  ( -6.914686169612833666, 117.4533518774869947, 0.3713220847589206453 ) ) ;
#9421 = ORIENTED_EDGE ( 'NONE', *, *, #33484, .T. ) ;
#9422 = CARTESIAN_POINT ( 'NONE',  ( 5.241362157049035631, 77.01756249999996840, 5.310945289804168468 ) ) ;
#9423 = ORIENTED_EDGE ( 'NONE', *, *, #586, .F. ) ;
#9424 = CARTESIAN_POINT ( 'NONE',  ( -41.63373767251972168, 22.51256436878228939, -1.325597493795125370 ) ) ;
#9425 = CARTESIAN_POINT ( 'NONE',  ( 5.478045763647380717, -15.20773871853380044, 2.260320276039294640 ) ) ;
#9426 = CARTESIAN_POINT ( 'NONE',  ( -4.077592138694987156, 118.2594131075661608, 0.7845094026950486521 ) ) ;
#9427 = CARTESIAN_POINT ( 'NONE',  ( 0.3953301572311454515, 117.5049145548240972, -0.4632619789290191581 ) ) ;
#9428 = CARTESIAN_POINT ( 'NONE',  ( 3.102408547967445696, -0.5812848888516047863, -3.453265078539196509 ) ) ;
#9429 = EDGE_CURVE ( 'NONE', #14379, #35331, #2056, .T. ) ;
#9430 = CARTESIAN_POINT ( 'NONE',  ( -58.44674015341568918, 0.09518567107959752249, -0.7847720614711276577 ) ) ;
#9431 = ORIENTED_EDGE ( 'NONE', *, *, #40256, .F. ) ;
#9432 = CARTESIAN_POINT ( 'NONE',  ( -58.62884620442462591, -0.7615560826026042118, -0.07633319197460453065 ) ) ;
#9433 = CARTESIAN_POINT ( 'NONE',  ( -0.03040743767366425876, 116.4813942609868178, 1.521712522323299677 ) ) ;
#9434 = CARTESIAN_POINT ( 'NONE',  ( 0.09641566778496790668, 105.7853610664053008, -4.825034276358896257 ) ) ;
#9435 = CARTESIAN_POINT ( 'NONE',  ( -17.30559516374544771, 146.8699245690979751, 1.364999074652126110 ) ) ;
#9436 = FACE_OUTER_BOUND ( 'NONE', #30737, .T. ) ;
#9437 = CIRCLE ( 'NONE', #8069, 0.5080000000000000071 ) ;
#9438 = CARTESIAN_POINT ( 'NONE',  ( 4.149433946629322634, 157.3082466949932723, -1.660590259719063377 ) ) ;
#9439 = CIRCLE ( 'NONE', #38699, 0.3810000000000015041 ) ;
#9440 = CARTESIAN_POINT ( 'NONE',  ( -9.223174309219253075, 157.2521837264336853, -1.945851059610182343 ) ) ;
#9441 = CARTESIAN_POINT ( 'NONE',  ( -58.73801720703743001, -0.4998429216807459552, -1.049519136981926467E-14 ) ) ;
#9442 = ORIENTED_EDGE ( 'NONE', *, *, #3453, .T. ) ;
#9443 = EDGE_CURVE ( 'NONE', #15268, #12250, #27219, .T. ) ;
#9444 = CARTESIAN_POINT ( 'NONE',  ( 13.50624371993741768, 134.2048320552371763, -0.5584564168634338355 ) ) ;
#9445 = ORIENTED_EDGE ( 'NONE', *, *, #20644, .T. ) ;
#9446 = CARTESIAN_POINT ( 'NONE',  ( -9.425008295912185474, 155.1592096034013366, -1.957465225861826363 ) ) ;
#9447 = CARTESIAN_POINT ( 'NONE',  ( 3.303734845180175128, -14.82389436555148166, -0.08037074644983704941 ) ) ;
#9448 = CARTESIAN_POINT ( 'NONE',  ( -6.472048963935522405E-14, 69.43546620154573645, -1.207165458941418601E-19 ) ) ;
#9449 = CARTESIAN_POINT ( 'NONE',  ( -48.50421218116025557, 14.67712143704001626, -8.170758227952415863E-15 ) ) ;
#9450 = PRODUCT_RELATED_PRODUCT_CATEGORY ( 'part', '', ( #29310 ) ) ;
#9451 = CARTESIAN_POINT ( 'NONE',  ( -4.891214509481254247, 117.7454895227670448, 0.7291075753013545047 ) ) ;
#9452 = CARTESIAN_POINT ( 'NONE',  ( 11.90495122372358594, 153.4554508723442439, 1.948344234133813302 ) ) ;
#9453 = CARTESIAN_POINT ( 'NONE',  ( -14.39766717389550443, 30.83083951148099189, -1.904999999999999805 ) ) ;
#9454 = CARTESIAN_POINT ( 'NONE',  ( -4.631227783250409402, 22.10816835407601744, -0.05711764529929251599 ) ) ;
#9455 = CARTESIAN_POINT ( 'NONE',  ( 1.598479218588785944, 156.2658572007470639, 0.3094434466263951133 ) ) ;
#9456 = LINE ( 'NONE', #13066, #14029 ) ;
#9457 = EDGE_CURVE ( 'NONE', #3896, #31942, #24, .T. ) ;
#9458 = ADVANCED_FACE ( 'NONE', ( #35603 ), #41624, .T. ) ;
#9459 = CIRCLE ( 'NONE', #29193, 2.540000000000000480 ) ;
#9461 = ORIENTED_EDGE ( 'NONE', *, *, #42058, .T. ) ;
#9460 = CARTESIAN_POINT ( 'NONE',  ( -45.37978287637889707, 19.43610829578849675, -1.699483007375131249 ) ) ;
#9462 = DIRECTION ( 'NONE',  ( 4.017660918040594346E-17, -1.000000000000000000, -2.376309959284834438E-19 ) ) ;
#9463 = CARTESIAN_POINT ( 'NONE',  ( -47.01877684503696742, 24.36789988528162354, 2.430126310640454257 ) ) ;
#9464 = CARTESIAN_POINT ( 'NONE',  ( -56.40692165385873125, 4.437999542203786341, 2.560908555091980787 ) ) ;
#9465 = CARTESIAN_POINT ( 'NONE',  ( -8.264889197776337681, 120.1602524387331243, -1.449212996374321438 ) ) ;
#9466 = EDGE_CURVE ( 'NONE', #30610, #40365, #36081, .T. ) ;
#9467 = FACE_OUTER_BOUND ( 'NONE', #32191, .T. ) ;
#9468 = CARTESIAN_POINT ( 'NONE',  ( -53.89938688035451975, 11.68864614896874343, 3.017114338529855111 ) ) ;
#9469 = CARTESIAN_POINT ( 'NONE',  ( -0.003550357976012296669, 159.5989787797044812, 0.1776744311461875836 ) ) ;
#9470 = ORIENTED_EDGE ( 'NONE', *, *, #5123, .F. ) ;
#9471 = CARTESIAN_POINT ( 'NONE',  ( -55.45615287082594591, 8.171946630687445534, -2.478682617993501758 ) ) ;
#9472 = CARTESIAN_POINT ( 'NONE',  ( 6.049355777633639519, 121.4441731105445967, 0.09395347381935742481 ) ) ;
#9473 = ORIENTED_EDGE ( 'NONE', *, *, #19413, .F. ) ;
#9474 = CARTESIAN_POINT ( 'NONE',  ( 1.240160200305893134, 115.7029491485453576, -1.694595060456987712 ) ) ;
#9475 = CARTESIAN_POINT ( 'NONE',  ( -11.85612367793094535, 151.9842433124228762, -0.4520816642129336094 ) ) ;
#9476 = CARTESIAN_POINT ( 'NONE',  ( 2.467627578834723057, -15.39586678991472546, 5.881674146221526733 ) ) ;
#9477 = CARTESIAN_POINT ( 'NONE',  ( -0.4156903444693582084, 117.7785671674745771, 0.5149838300002416158 ) ) ;
#9478 = CYLINDRICAL_SURFACE ( 'NONE', #17257, 0.6350000000000006750 ) ;
#9479 = CARTESIAN_POINT ( 'NONE',  ( 21.47487836045312903, 132.5742979909900328, 0.7254175812904737342 ) ) ;
#9480 = CARTESIAN_POINT ( 'NONE',  ( 8.833705352582880366, 123.8898140529132803, 0.3087918532372332381 ) ) ;
#9481 = CARTESIAN_POINT ( 'NONE',  ( 4.765923672690803414, 118.5266822147775940, -0.8411494563746799713 ) ) ;
#9482 = CARTESIAN_POINT ( 'NONE',  ( -0.9350042896817728488, 3.318609271805546435, -0.2773724203853295545 ) ) ;
#9483 = CARTESIAN_POINT ( 'NONE',  ( -15.43849248880397873, 120.7004057517279989, -0.4663222373074406568 ) ) ;
#9484 = DIRECTION ( 'NONE',  ( 5.188838149069472160E-16, -1.699382548006136559E-16, -1.000000000000000000 ) ) ;
#9485 = FACE_OUTER_BOUND ( 'NONE', #41835, .T. ) ;
#9486 = ORIENTED_EDGE ( 'NONE', *, *, #20344, .T. ) ;
#9487 = CARTESIAN_POINT ( 'NONE',  ( -2.573107000771836628, 116.8397100664982986, 0.4471336313416622854 ) ) ;
#9488 = VERTEX_POINT ( 'NONE', #10447 ) ;
#9489 = CARTESIAN_POINT ( 'NONE',  ( -58.34965918702084764, -0.2493686153283701523, -0.1767538080080786056 ) ) ;
#9490 = CARTESIAN_POINT ( 'NONE',  ( 14.06037840947770867, 121.6707806233237363, 1.579157835890536710 ) ) ;
#9491 = CARTESIAN_POINT ( 'NONE',  ( 5.882864265865802800, 118.8996324090661147, -0.9452689120681908586 ) ) ;
#9492 = CARTESIAN_POINT ( 'NONE',  ( 8.413794655563325620, 13.29309125005104164, 0.5966991197660089785 ) ) ;
#9493 = CARTESIAN_POINT ( 'NONE',  ( -18.27285712481730684, 128.6097515361309149, -1.839992588890194458 ) ) ;
#9494 = CARTESIAN_POINT ( 'NONE',  ( 4.617617679964085120, 117.9735077130049206, -0.7424316868072086129 ) ) ;
#9495 = CARTESIAN_POINT ( 'NONE',  ( 5.246745461247972919, 116.0761519159950552, 1.241752167516083194 ) ) ;
#9496 = CIRCLE ( 'NONE', #33348, 3.111499999999999932 ) ;
#9497 = CARTESIAN_POINT ( 'NONE',  ( -5.940729632618867662, 121.5467800236367424, -0.09028238529180369898 ) ) ;
#9498 = CARTESIAN_POINT ( 'NONE',  ( -13.91666582400481644, 125.7699432187419575, -2.002145485623346932 ) ) ;
#9500 = CARTESIAN_POINT ( 'NONE',  ( 5.683854215195817794, -15.08228171793801664, 1.486458664383613293 ) ) ;
#9499 = CIRCLE ( 'NONE', #29223, 9.048749999999994742 ) ;
#9501 = DIRECTION ( 'NONE',  ( -0.8745520943968250194, 0.4849315768086535083, -5.424246918827963022E-16 ) ) ;
#9502 = CARTESIAN_POINT ( 'NONE',  ( -42.79661761208809168, 21.81806929429799879, -2.089873509012822428 ) ) ;
#9503 = ADVANCED_FACE ( 'NONE', ( #23418 ), #29249, .T. ) ;
#9504 = ORIENTED_EDGE ( 'NONE', *, *, #14506, .T. ) ;
#9505 = CARTESIAN_POINT ( 'NONE',  ( 16.73131056987022092, 135.2943057719725459, 2.348795921478700865 ) ) ;
#9506 = DIRECTION ( 'NONE',  ( -4.017660918040594346E-17, 1.000000000000000000, 2.376309959284834438E-19 ) ) ;
#9507 = LINE ( 'NONE', #9718, #35961 ) ;
#9508 = CARTESIAN_POINT ( 'NONE',  ( -0.2613516939666690186, 106.0087397856094356, 5.279363957283110587 ) ) ;
#9509 = CARTESIAN_POINT ( 'NONE',  ( -8.368269197548203309, 31.49133049583987187, -0.7708832981534754492 ) ) ;
#9510 = CARTESIAN_POINT ( 'NONE',  ( 16.05307823990497340, 146.0544122543811341, 1.176040581308522404 ) ) ;
#9511 = CARTESIAN_POINT ( 'NONE',  ( 5.858194661467363673, 117.3723397083485622, -0.4592760973624643861 ) ) ;
#9512 = LINE ( 'NONE', #22900, #23306 ) ;
#9513 = DIRECTION ( 'NONE',  ( 1.011795553208986377E-16, 1.000000000000000000, -0.000000000000000000 ) ) ;
#9514 = EDGE_CURVE ( 'NONE', #23040, #38078, #8860, .T. ) ;
#9515 = AXIS2_PLACEMENT_3D ( 'NONE', #11913, #24901, #2131 ) ;
#9516 = CARTESIAN_POINT ( 'NONE',  ( -0.0002734175339917587714, 159.6054662015457382, 0.01368293144939993107 ) ) ;
#9517 = EDGE_CURVE ( 'NONE', #4652, #449, #14772, .T. ) ;
#9518 = ORIENTED_EDGE ( 'NONE', *, *, #34479, .T. ) ;
#9519 = CARTESIAN_POINT ( 'NONE',  ( -8.133793902695101607, 120.8064541497650310, -1.378343526931617102 ) ) ;
#9520 = CARTESIAN_POINT ( 'NONE',  ( 23.36121599383890768, 148.8756354987169175, 0.4668126921610644131 ) ) ;
#9521 = CARTESIAN_POINT ( 'NONE',  ( -7.977778825752325886, 154.6030710842251494, -0.7700301581992886613 ) ) ;
#9522 = CARTESIAN_POINT ( 'NONE',  ( 4.143153066788715755, -13.73528615761443561, 4.025237717645509861 ) ) ;
#9523 = CARTESIAN_POINT ( 'NONE',  ( 7.002510704594238966, 121.9568449727899520, 0.1399268299516837899 ) ) ;
#9524 = CARTESIAN_POINT ( 'NONE',  ( 3.706843470526773654, 116.6237204831772232, 0.08772160974583174953 ) ) ;
#9525 = ORIENTED_EDGE ( 'NONE', *, *, #7643, .F. ) ;
#9526 = CARTESIAN_POINT ( 'NONE',  ( 4.326043401919948295, 8.289558097378858292, -1.648119079657388353 ) ) ;
#9527 = CARTESIAN_POINT ( 'NONE',  ( -23.29144772315980916, 149.3526176766912101, -0.4654185560736369132 ) ) ;
#9528 = CARTESIAN_POINT ( 'NONE',  ( -16.46263872254443683, 83.91929436251373886, -1.270000000000002460 ) ) ;
#9529 = CARTESIAN_POINT ( 'NONE',  ( 5.157440735887882433, 114.7154655033523198, 1.455969569964357557 ) ) ;
#9530 = CARTESIAN_POINT ( 'NONE',  ( 6.105266827213309710, 121.0439321044046039, 0.7736761210806879507 ) ) ;
#9531 = CARTESIAN_POINT ( 'NONE',  ( -1.889208318266999198, 10.27326514537015534, 4.227218769941996968 ) ) ;
#9532 = CARTESIAN_POINT ( 'NONE',  ( 14.71083544318249281, 121.0688405154646858, 1.213083844406488199 ) ) ;
#9533 = CARTESIAN_POINT ( 'NONE',  ( -7.772068811996249771, 69.25462295839062676, -1.269999999999995577 ) ) ;
#9535 = CARTESIAN_POINT ( 'NONE',  ( 1.161715739485780885, 117.9723128000925669, -0.5854012653586093684 ) ) ;
#9534 = CARTESIAN_POINT ( 'NONE',  ( 2.943565496889787525, 108.2627120386935502, 4.302928841461297615 ) ) ;
#9536 = CARTESIAN_POINT ( 'NONE',  ( 3.363087486136625337, 4.875765145370108300, -3.182472177310056605 ) ) ;
#9537 = CARTESIAN_POINT ( 'NONE',  ( -13.11470433356391929, 119.8381915656929380, -0.9809890993017411631 ) ) ;
#9538 = VERTEX_POINT ( 'NONE', #15306 ) ;
#9539 = CARTESIAN_POINT ( 'NONE',  ( -5.903620821223855231, 121.4229528491920576, 0.1845582724821507592 ) ) ;
#9540 = CARTESIAN_POINT ( 'NONE',  ( 6.072898904334845582, -12.55662260458653634, 0.7994981368886315831 ) ) ;
#9541 = AXIS2_PLACEMENT_3D ( 'NONE', #36874, #13440, #32828 ) ;
#9542 = CARTESIAN_POINT ( 'NONE',  ( -46.38316532014824389, 26.05065462784537900, 1.269999999999990914 ) ) ;
#9543 = CARTESIAN_POINT ( 'NONE',  ( -4.593215935933216088, 118.0632729301879920, -0.7325469166207362326 ) ) ;
#9544 = CARTESIAN_POINT ( 'NONE',  ( 11.83770080265064983, 152.0103986367769551, 0.1887002032782131022 ) ) ;
#9545 = ORIENTED_EDGE ( 'NONE', *, *, #19123, .T. ) ;
#9546 = CARTESIAN_POINT ( 'NONE',  ( 0.4459748878572474817, 118.5593716040226724, 0.6139719676240720236 ) ) ;
#9547 = CARTESIAN_POINT ( 'NONE',  ( -29.91139568370676116, 83.95719535527391031, -1.270000000000009566 ) ) ;
#9548 = DIRECTION ( 'NONE',  ( 0.000000000000000000, 0.000000000000000000, -1.000000000000000000 ) ) ;
#9549 = CARTESIAN_POINT ( 'NONE',  ( -4.852593915752414055, 117.2114307359545649, 0.4396237197203591296 ) ) ;
#9550 = DIRECTION ( 'NONE',  ( -0.9454731675810359448, 0.3256999990547780333, -5.459396135145339171E-16 ) ) ;
#9551 = CARTESIAN_POINT ( 'NONE',  ( 15.39314341005339948, 120.8297411738997624, -0.1127201291141931155 ) ) ;
#9552 = EDGE_CURVE ( 'NONE', #13530, #450, #8515, .T. ) ;
#9553 = PLANE ( 'NONE',  #17199 ) ;
#9554 = CARTESIAN_POINT ( 'NONE',  ( -50.94359596358804509, 14.56251409809150132, 4.558007702229759595 ) ) ;
#9555 = CARTESIAN_POINT ( 'NONE',  ( -46.93986413309943373, 25.37947832266650039, 1.074976477481959902 ) ) ;
#9556 = CIRCLE ( 'NONE', #39540, 0.2540000000000012248 ) ;
#9558 = ADVANCED_FACE ( 'NONE', ( #12335 ), #1720, .T. ) ;
#9557 = DIRECTION ( 'NONE',  ( 5.188838149069472160E-16, -1.699382548006136559E-16, -1.000000000000000000 ) ) ;
#9559 = CARTESIAN_POINT ( 'NONE',  ( -48.56815661899837977, 19.24492339269602681, 5.224590812749973168 ) ) ;
#9560 = CARTESIAN_POINT ( 'NONE',  ( -58.67901903226392335, -0.3139884119181903799, 0.3104539207526157418 ) ) ;
#9561 = CARTESIAN_POINT ( 'NONE',  ( -4.632005028902471011, 118.0396561689580324, 0.6218044277692786892 ) ) ;
#9562 = CARTESIAN_POINT ( 'NONE',  ( -58.16721443865020547, 0.09938604254088045931, -0.2878065994480087375 ) ) ;
#9563 = B_SPLINE_SURFACE_WITH_KNOTS ( 'NONE', 1, 3, ( 
 ( #19555, #16580, #35564, #18934, #9361, #15946, #38756, #29371, #6798, #9161, #28943, #3617, #9566, #22118, #35772, #39174, #32564, #6382 ),
 ( #3398, #16365, #13185, #210, #31943, #25545, #32358, #41755, #2781, #9981, #19766, #15737, #22955, #35982, #28741, #29798, #10193, #23380 ) ),
 .UNSPECIFIED., .F., .F., .F.,
 ( 2, 2 ),
 ( 4, 2, 2, 2, 2, 2, 2, 2, 4 ),
 ( 0.000000000000000000, 1.000000000000000000 ),
 ( 0.000000000000000000, 0.06250000000000000000, 0.1250000000000000000, 0.1875000000000000000, 0.2500000000000000000, 0.3750000000000000000, 0.5000000000000000000, 0.7500000000000000000, 1.000000000000000000 ),
 .UNSPECIFIED. ) ;
#9564 = ORIENTED_EDGE ( 'NONE', *, *, #32332, .T. ) ;
#9565 = ORIENTED_EDGE ( 'NONE', *, *, #19873, .F. ) ;
#9566 = CARTESIAN_POINT ( 'NONE',  ( -2.186492930797574452, 115.6909491485466646, -1.711433661021510177 ) ) ;
#9567 = CARTESIAN_POINT ( 'NONE',  ( -5.931588090995600027, 119.1690655882911329, -1.264883306644118743 ) ) ;
#9568 = CARTESIAN_POINT ( 'NONE',  ( -1.966029823418521172, 106.7001829816230725, -4.962286218837188123 ) ) ;
#9570 = CARTESIAN_POINT ( 'NONE',  ( 4.742030083010273955, 117.8490966506599307, 0.9897493978187200669 ) ) ;
#9569 = VECTOR ( 'NONE', #28982, 1000.000000000000000 ) ;
#9571 = CARTESIAN_POINT ( 'NONE',  ( 2.969447359227861405, -13.80100253337253946, 0.9847735008004718793 ) ) ;
#9572 = CARTESIAN_POINT ( 'NONE',  ( -15.17477609654696380, 139.4722935914273307, -1.590378199732649600 ) ) ;
#9573 = CARTESIAN_POINT ( 'NONE',  ( -2.528362934948840124, 115.7031097563144471, -1.694662335315127777 ) ) ;
#9574 = CARTESIAN_POINT ( 'NONE',  ( -3.523571992936364694, 109.1382962752385026, 3.814013227644438064 ) ) ;
#9575 = DIRECTION ( 'NONE',  ( 0.3256999990547876367, 0.9454731675810326141, 8.328397965208553695E-18 ) ) ;
#9576 = CARTESIAN_POINT ( 'NONE',  ( 2.658992269297059785, 107.2388417251876547, -4.621886736208384860 ) ) ;
#9577 = CARTESIAN_POINT ( 'NONE',  ( -17.04317705290392837, 148.4623951536435698, -2.145728921095965358 ) ) ;
#9578 = DIRECTION ( 'NONE',  ( 1.011795553208986377E-16, 1.000000000000000000, -0.000000000000000000 ) ) ;
#9579 = CARTESIAN_POINT ( 'NONE',  ( -0.03067001211942338088, 158.6015251912307633, 1.534852821454057770 ) ) ;
#9580 = CARTESIAN_POINT ( 'NONE',  ( -3.399038284204972449, 115.7029691290877906, 1.510463350574593022 ) ) ;
#9581 = CARTESIAN_POINT ( 'NONE',  ( -1.214995109038484067, 0.9429784454696930052, -4.460028654918597901 ) ) ;
#9583 = ORIENTED_EDGE ( 'NONE', *, *, #37125, .F. ) ;
#9582 = CARTESIAN_POINT ( 'NONE',  ( 10.62864291685173512, 157.9324367681937815, 0.7848347606368001328 ) ) ;
#9584 = DIRECTION ( 'NONE',  ( -0.8745520943968249084, 0.4849315768086533418, -5.271987356194193006E-16 ) ) ;
#9585 = CARTESIAN_POINT ( 'NONE',  ( 3.162278034637682200, -15.50568859125470134, 4.121945908858189789 ) ) ;
#9586 = CARTESIAN_POINT ( 'NONE',  ( -19.59580906854019844, 147.4874203640471535, 1.738765900131762798 ) ) ;
#9587 = CARTESIAN_POINT ( 'NONE',  ( 0.4410767147925211407, 14.17415678908661469, -0.8685042294053136880 ) ) ;
#9588 = CARTESIAN_POINT ( 'NONE',  ( 0.9048393610272945642, 9.142100508531621372, -0.3649321582425499311 ) ) ;
#9589 = ORIENTED_EDGE ( 'NONE', *, *, #32177, .T. ) ;
#9590 = EDGE_LOOP ( 'NONE', ( #6538, #30234 ) ) ;
#9591 = CARTESIAN_POINT ( 'NONE',  ( -4.854186777038641765, 117.7557277303023966, -0.9091791526384296329 ) ) ;
#9592 = CARTESIAN_POINT ( 'NONE',  ( 4.672526732406415029, 120.2198808273567892, 0.4623614190293561799 ) ) ;
#9593 =( NAMED_UNIT ( * ) SI_UNIT ( $, .STERADIAN. ) SOLID_ANGLE_UNIT ( ) );
#9594 = CARTESIAN_POINT ( 'NONE',  ( -9.503290916781066855, 123.5188755717998816, 0.5781397488420940700 ) ) ;
#9595 = CARTESIAN_POINT ( 'NONE',  ( 3.564576864782785570, -14.06793500455072454, 4.479818044377421593 ) ) ;
#9596 = CARTESIAN_POINT ( 'NONE',  ( 14.72636943223149331, 131.2156652454908112, -1.433095336252469654 ) ) ;
#9597 = CARTESIAN_POINT ( 'NONE',  ( -2.460791562519598408, 158.0185616612000956, -1.723846131599015230 ) ) ;
#9598 = CARTESIAN_POINT ( 'NONE',  ( -26.51793118801306548, 72.98537704160715123, 1.269999999999993134 ) ) ;
#9599 = VECTOR ( 'NONE', #713, 1000.000000000000227 ) ;
#9600 = CARTESIAN_POINT ( 'NONE',  ( 8.744610207651122735, 117.8906195244964152, 0.6684397885285150442 ) ) ;
#9601 = CARTESIAN_POINT ( 'NONE',  ( -0.4214665657712599045, 37.86644440679212664, 0.8455140659468449726 ) ) ;
#9602 = CARTESIAN_POINT ( 'NONE',  ( 7.598614292646840518, 122.4062900713904440, -0.04802449110505816604 ) ) ;
#9603 = ORIENTED_EDGE ( 'NONE', *, *, #22178, .T. ) ;
#9604 = CARTESIAN_POINT ( 'NONE',  ( -6.651972016613293606E-14, 104.1064662015457287, 7.011588703784780528E-31 ) ) ;
#9605 = CIRCLE ( 'NONE', #33428, 2.540000000000000480 ) ;
#9606 = CARTESIAN_POINT ( 'NONE',  ( 10.39494437172059094, 56.51500000000000057, 5.094799277214218769 ) ) ;
#9607 = CARTESIAN_POINT ( 'NONE',  ( 5.028190701329536161, 117.3993840585409316, -0.6260521898566507870 ) ) ;
#9608 = CARTESIAN_POINT ( 'NONE',  ( 4.636268038904784561, 155.9604050671876792, 1.079575001969329096 ) ) ;
#9609 = LINE ( 'NONE', #22577, #879 ) ;
#9610 = CARTESIAN_POINT ( 'NONE',  ( 0.3042766021092446760, 116.4832816433156069, -0.08781055504204327011 ) ) ;
#9611 = CARTESIAN_POINT ( 'NONE',  ( -5.434281097240536873, 117.1681999988027911, 0.6838767007579790169 ) ) ;
#9612 = CARTESIAN_POINT ( 'NONE',  ( -5.078986093043186045, 92.04146620154574521, -0.1014902294541237954 ) ) ;
#9613 = CARTESIAN_POINT ( 'NONE',  ( -17.14499999999999957, 71.11999999999999034, 5.714999999999999858 ) ) ;
#9614 = CARTESIAN_POINT ( 'NONE',  ( -4.847303688887219408, 31.57325935411374473, -0.5121714807418957793 ) ) ;
#9615 = EDGE_CURVE ( 'NONE', #23143, #17052, #41527, .T. ) ;
#9616 = CARTESIAN_POINT ( 'NONE',  ( 21.01875934457253692, 148.7375953542188256, 2.355668865594947370 ) ) ;
#9617 = CARTESIAN_POINT ( 'NONE',  ( 1.677595020332960152, 24.74158224480939339, -4.309653081027373211 ) ) ;
#9618 = CARTESIAN_POINT ( 'NONE',  ( -8.384998746481384657, -10.44493509673469767, 0.7792886224267949746 ) ) ;
#9619 = CARTESIAN_POINT ( 'NONE',  ( -8.725233207679389480, 117.9832267607160929, -0.7526383660895783478 ) ) ;
#9620 = CARTESIAN_POINT ( 'NONE',  ( -2.328338358121225582, 124.8000875644994068, -0.05398387088914113896 ) ) ;
#9621 = CARTESIAN_POINT ( 'NONE',  ( -23.21373371908098449, 149.6306211361744829, -0.4638656453230912136 ) ) ;
#9622 = CARTESIAN_POINT ( 'NONE',  ( 1.958559173108875173, 106.7079595946689494, -4.892068575404730169 ) ) ;
#9623 = CARTESIAN_POINT ( 'NONE',  ( 2.359926926834857941, 104.6144662015456817, 4.210384773563669469 ) ) ;
#9624 = AXIS2_PLACEMENT_3D ( 'NONE', #33950, #14748, #20719 ) ;
#9625 = CARTESIAN_POINT ( 'NONE',  ( 3.548611814566905664, 16.26088872207684943, 2.983771105379771971 ) ) ;
#9626 = DIRECTION ( 'NONE',  ( 0.8745520943968249084, -0.4849315768086533418, 5.271987356194193006E-16 ) ) ;
#9627 = CARTESIAN_POINT ( 'NONE',  ( 12.69999999999999929, 11.53894877578616907, 0.000000000000000000 ) ) ;
#9628 = CARTESIAN_POINT ( 'NONE',  ( 2.967701212693483193, -13.54563334627871463, 1.070011838909553425 ) ) ;
#9629 = CARTESIAN_POINT ( 'NONE',  ( 1.979347617175751806, 122.1523088006674840, -0.1944583918105483034 ) ) ;
#9630 = CARTESIAN_POINT ( 'NONE',  ( -9.649066847268132463, 118.2334930433176652, 0.3843608719459137291 ) ) ;
#9631 = ORIENTED_EDGE ( 'NONE', *, *, #17811, .T. ) ;
#9632 = DIRECTION ( 'NONE',  ( -0.7517731442105912709, 0.6594218222380281436, -8.537024980200781389E-16 ) ) ;
#9633 = VERTEX_POINT ( 'NONE', #5754 ) ;
#9634 = CARTESIAN_POINT ( 'NONE',  ( -30.75918919842648336, 69.77432548395512413, 1.269999999999991358 ) ) ;
#9635 = CARTESIAN_POINT ( 'NONE',  ( 2.047221892555406431, -15.65848914036231676, 5.808978358897256555 ) ) ;
#9636 = CARTESIAN_POINT ( 'NONE',  ( -13.37375235405036378, 122.3357896625302459, 1.257830042033918350 ) ) ;
#9637 = CARTESIAN_POINT ( 'NONE',  ( 19.57327063168399306, 152.2820370773569323, -1.161482255138347686 ) ) ;
#9638 = CARTESIAN_POINT ( 'NONE',  ( 3.501419995798253915, -2.955197114699519734, 3.043391175950921568 ) ) ;
#9639 = CARTESIAN_POINT ( 'NONE',  ( -58.35071543880859934, 0.3020958082991723748, -0.9346586068229112421 ) ) ;
#9640 = B_SPLINE_CURVE_WITH_KNOTS ( 'NONE', 3,
 ( #10086, #32259, #3294, #3088, #3723, #38655, #38859, #9874, #9463, #35884, #32465, #16258 ),
 .UNSPECIFIED., .F., .F.,
 ( 4, 1, 1, 1, 1, 1, 1, 1, 1, 4 ),
 ( 0.7354344192538688763, 0.7500000000000001110, 0.7685053377236187311, 0.8015760037631017854, 0.8346466698025848396, 0.8677173358420678939, 0.9007880018815509482, 0.9338586679210340025, 0.9503940009407755296, 0.9543042185119943177 ),
 .UNSPECIFIED. ) ;
#9641 = ORIENTED_EDGE ( 'NONE', *, *, #633, .T. ) ;
#9642 = CARTESIAN_POINT ( 'NONE',  ( -54.09072575249082604, 8.649776409409795974, -3.422340198163621228 ) ) ;
#9643 = CARTESIAN_POINT ( 'NONE',  ( -0.01331772329000604355, 119.9741034315943864, 0.6664733318051297983 ) ) ;
#9644 = CARTESIAN_POINT ( 'NONE',  ( -10.60072409500466861, 154.2769816202975051, 1.465916755537046479 ) ) ;
#9645 = DIRECTION ( 'NONE',  ( -0.7770581983690852956, 0.6294287539884014793, -4.360450048231382406E-16 ) ) ;
#9646 = CARTESIAN_POINT ( 'NONE',  ( 12.07275429247921039, 123.1955650103826798, -1.290935347410189227 ) ) ;
#9647 = CARTESIAN_POINT ( 'NONE',  ( -14.62144676724406089, 123.3142630313093377, -1.799443978378394648 ) ) ;
#9648 = CARTESIAN_POINT ( 'NONE',  ( -58.55221842960730783, 0.5754175076986972615, -0.9757793345693789311 ) ) ;
#9649 = EDGE_LOOP ( 'NONE', ( #39084, #24342, #23298, #9525 ) ) ;
#9650 = CARTESIAN_POINT ( 'NONE',  ( 4.439712258926299171, 118.1647990948395233, -0.4552782637668283394 ) ) ;
#9651 = CARTESIAN_POINT ( 'NONE',  ( 12.22709855250464450, 151.9982576965888654, -0.6666368699087850125 ) ) ;
#9652 = ORIENTED_EDGE ( 'NONE', *, *, #22054, .F. ) ;
#9653 = CARTESIAN_POINT ( 'NONE',  ( 0.009513407573613850629, 119.7614543879625586, -0.4760898169610155994 ) ) ;
#9654 = CARTESIAN_POINT ( 'NONE',  ( 3.824421424077324883, -15.38127155850414773, 2.203493915304267858 ) ) ;
#9655 = EDGE_CURVE ( 'NONE', #10059, #1007, #15209, .T. ) ;
#9656 = DIRECTION ( 'NONE',  ( -0.01997839162482761832, -1.040247600000951803E-18, 0.9998004120163610509 ) ) ;
#9657 = DIRECTION ( 'NONE',  ( 0.8745520943968243532, -0.4849315768086547296, 6.829619984160642269E-16 ) ) ;
#9658 = ADVANCED_FACE ( 'NONE', ( #37475 ), #11699, .T. ) ;
#9659 = CARTESIAN_POINT ( 'NONE',  ( -4.766718869283322668, 117.7281659001820913, 0.9070997928662917209 ) ) ;
#9660 = CARTESIAN_POINT ( 'NONE',  ( 5.087176912069779178, 120.2090573957402455, 0.9271508619376561677 ) ) ;
#9661 = CARTESIAN_POINT ( 'NONE',  ( 6.349999999999963229, 57.14999999999999858, 0.000000000000000000 ) ) ;
#9662 = EDGE_CURVE ( 'NONE', #32297, #10127, #31717, .T. ) ;
#9663 = CARTESIAN_POINT ( 'NONE',  ( 3.211436584971100849, 28.15539441671475274, -3.345526564039049688 ) ) ;
#9664 = CARTESIAN_POINT ( 'NONE',  ( 6.489379754819697865, 121.7611753534313550, 0.2571143975131358617 ) ) ;
#9665 = CARTESIAN_POINT ( 'NONE',  ( -11.66725022231030628, 17.14499999999999957, 5.016499999999999737 ) ) ;
#9666 = AXIS2_PLACEMENT_3D ( 'NONE', #34154, #1781, #21333 ) ;
#9668 = ORIENTED_EDGE ( 'NONE', *, *, #14971, .T. ) ;
#9667 = CARTESIAN_POINT ( 'NONE',  ( -48.90916507497669841, 16.41193755240580288, -3.099911505780766685 ) ) ;
#9669 = CARTESIAN_POINT ( 'NONE',  ( -4.476425760464393555, 71.61790547347303004, 1.270000000000005791 ) ) ;
#9670 = LINE ( 'NONE', #35671, #22014 ) ;
#9671 = CARTESIAN_POINT ( 'NONE',  ( -48.84267179513337709, 18.06759678302662309, 5.143183091231904314 ) ) ;
#9672 = DIRECTION ( 'NONE',  ( -0.03103328369512481019, -0.9876883405951375483, 0.1533253963162051758 ) ) ;
#9673 = CARTESIAN_POINT ( 'NONE',  ( -5.305748947172302721, 88.73331249999998249, 5.247078976224250013 ) ) ;
#9674 = CARTESIAN_POINT ( 'NONE',  ( -17.65389921742009705, 84.42347906515803402, -1.270000000000003348 ) ) ;
#9675 = CARTESIAN_POINT ( 'NONE',  ( -55.24575511360421842, 11.19612964283526324, 0.2458718103055573534 ) ) ;
#9676 = CARTESIAN_POINT ( 'NONE',  ( -57.78858274104275949, 1.044662872677112997, 1.355440516197746303 ) ) ;
#9677 = ADVANCED_FACE ( 'NONE', ( #17874 ), #19718, .T. ) ;
#9678 = CARTESIAN_POINT ( 'NONE',  ( -9.765169485063884380, 118.0373187826741486, 0.07890504670268488896 ) ) ;
#9679 = EDGE_LOOP ( 'NONE', ( #14141, #9486, #6864, #39199 ) ) ;
#9680 = CARTESIAN_POINT ( 'NONE',  ( -54.68578128245503223, 13.03233524004687638, -1.089573673074214656E-14 ) ) ;
#9681 = CARTESIAN_POINT ( 'NONE',  ( -6.020519723803437806, 121.4387767156620015, -0.1661333497277762139 ) ) ;
#9682 = ORIENTED_EDGE ( 'NONE', *, *, #19865, .T. ) ;
#9683 = CARTESIAN_POINT ( 'NONE',  ( 3.034504105865374779, 115.7029491485452581, -1.550851629826452083 ) ) ;
#9684 = CARTESIAN_POINT ( 'NONE',  ( -15.27574012874729981, 148.0141687878753203, -0.5334971086861884926 ) ) ;
#9685 = CARTESIAN_POINT ( 'NONE',  ( 4.517131889307780312, -14.80175198191645336, 4.712020298053779754 ) ) ;
#9686 = CARTESIAN_POINT ( 'NONE',  ( -4.003603038177978135, 117.7793252414215317, 0.6798483224588710572 ) ) ;
#9687 = DIRECTION ( 'NONE',  ( -0.8745520943968249084, 0.4849315768086533418, -5.271987356194193006E-16 ) ) ;
#9688 = CARTESIAN_POINT ( 'NONE',  ( -0.002426349801211070533, 116.5266044092193880, 0.1214244658147705658 ) ) ;
#9689 = CARTESIAN_POINT ( 'NONE',  ( 11.82936742863723723, 152.0434717972437682, 0.3612672141402942239 ) ) ;
#9690 = CARTESIAN_POINT ( 'NONE',  ( -20.05275907367747124, 79.68882802557934042, -1.270000000000003793 ) ) ;
#9691 = CARTESIAN_POINT ( 'NONE',  ( -0.9745549951769645336, 13.24125360461694001, -0.07243667530571006041 ) ) ;
#9692 = CARTESIAN_POINT ( 'NONE',  ( -8.055701656131645905, 158.6724238832827609, -0.2706798611393587684 ) ) ;
#9693 = DIRECTION ( 'NONE',  ( 0.3086833358529555982, -0.9511648638205112416, 1.501066210750423308E-13 ) ) ;
#9694 = FACE_OUTER_BOUND ( 'NONE', #38150, .T. ) ;
#9695 = ORIENTED_EDGE ( 'NONE', *, *, #15927, .F. ) ;
#9696 = CARTESIAN_POINT ( 'NONE',  ( -2.319837389150895213, 116.4337650663298973, 0.2360035357957355751 ) ) ;
#9698 = ADVANCED_FACE ( 'NONE', ( #12123 ), #21272, .T. ) ;
#9697 = ORIENTED_EDGE ( 'NONE', *, *, #39980, .T. ) ;
#9699 = CARTESIAN_POINT ( 'NONE',  ( -58.34883683990797465, -0.2476419964839868537, -0.1803091383267578784 ) ) ;
#9700 = CARTESIAN_POINT ( 'NONE',  ( 6.809904206821519423, 118.2876074772933492, 1.086328812139343070 ) ) ;
#9701 = CARTESIAN_POINT ( 'NONE',  ( 2.301458206243025550, 118.5910164976458532, -0.7067537174111423459 ) ) ;
#9702 = CARTESIAN_POINT ( 'NONE',  ( 0.7350785369229140276, 15.66647056970591301, -8.407117359194836936 ) ) ;
#9703 = CARTESIAN_POINT ( 'NONE',  ( -0.3765078121169122549, 117.5049145548240972, -0.4786851384288721700 ) ) ;
#9704 = CARTESIAN_POINT ( 'NONE',  ( 4.777070507844503489, 117.8483530557036687, -0.7998628223812204174 ) ) ;
#9705 = DIRECTION ( 'NONE',  ( -0.1565721916417968096, -0.9876665170007964401, 0.000000000000000000 ) ) ;
#9706 = EDGE_CURVE ( 'NONE', #5873, #17114, #14282, .T. ) ;
#9707 = AXIS2_PLACEMENT_3D ( 'NONE', #35392, #22162, #19191 ) ;
#9708 = CARTESIAN_POINT ( 'NONE',  ( -7.788912029362665024, 154.6472212274131550, -0.1129171994251847999 ) ) ;
#9709 = ORIENTED_EDGE ( 'NONE', *, *, #17586, .T. ) ;
#9710 = CARTESIAN_POINT ( 'NONE',  ( -0.9451225546581241144, 157.6350123088122359, -1.628263479412583647 ) ) ;
#9711 = CARTESIAN_POINT ( 'NONE',  ( 5.875553665316252783, -14.89341971632543427, 0.3075322240006022056 ) ) ;
#9712 = CARTESIAN_POINT ( 'NONE',  ( 4.787316872900306386, 118.5931160184169073, 0.9404912388413474433 ) ) ;
#9713 = ADVANCED_FACE ( 'NONE', ( #38117 ), #25839, .T. ) ;
#9714 = CARTESIAN_POINT ( 'NONE',  ( -41.88683177698051452, 22.33947639032530219, -1.656270940288501636 ) ) ;
#9715 = VERTEX_POINT ( 'NONE', #31500 ) ;
#9716 = CARTESIAN_POINT ( 'NONE',  ( 15.37772490044519280, 131.3329289045130679, 2.176645470406190608 ) ) ;
#9717 = DIRECTION ( 'NONE',  ( 0.000000000000000000, 1.000000000000000000, 0.000000000000000000 ) ) ;
#9718 = CARTESIAN_POINT ( 'NONE',  ( -30.45812239790965492, 71.16801738242446618, 1.269999999999991358 ) ) ;
#9719 = AXIS2_PLACEMENT_3D ( 'NONE', #20299, #16486, #13928 ) ;
#9720 = CARTESIAN_POINT ( 'NONE',  ( -4.687267571634002650, 120.2198808273567892, 0.2753304537621713011 ) ) ;
#9721 = CARTESIAN_POINT ( 'NONE',  ( 5.686328549477039473, -14.11678386645415628, -6.209864621142330954 ) ) ;
#9722 = CARTESIAN_POINT ( 'NONE',  ( -0.009747742627877935620, 156.3581291470199233, 0.4878169013068173743 ) ) ;
#9723 = CARTESIAN_POINT ( 'NONE',  ( 22.87957784423531749, 146.5373477140321938, -0.6332847025415451192 ) ) ;
#9724 = CARTESIAN_POINT ( 'NONE',  ( -10.28897677580358305, 57.14999999999998437, -4.381499999999999950 ) ) ;
#9725 = CARTESIAN_POINT ( 'NONE',  ( -19.68500000000000227, 71.11999999999999034, 5.016499999999999737 ) ) ;
#9726 = CIRCLE ( 'NONE', #2267, 5.080000000000006288 ) ;
#9727 = B_SPLINE_CURVE_WITH_KNOTS ( 'NONE', 3,
 ( #989, #17147, #32937, #36352 ),
 .UNSPECIFIED., .F., .F.,
 ( 4, 4 ),
 ( 0.7699389564571422762, 1.000000000000000000 ),
 .UNSPECIFIED. ) ;
#9728 = CARTESIAN_POINT ( 'NONE',  ( -22.66443576792692838, 150.6395781703034231, -0.4273611094724394932 ) ) ;
#9729 = ORIENTED_EDGE ( 'NONE', *, *, #3047, .T. ) ;
#9730 = CARTESIAN_POINT ( 'NONE',  ( -6.306168215838764191, 119.9765817188901451, -1.212549642329949995 ) ) ;
#9731 = CARTESIAN_POINT ( 'NONE',  ( -8.270297712355500153, 69.35377921309405735, -1.269999999999995799 ) ) ;
#9732 = CARTESIAN_POINT ( 'NONE',  ( -3.002817136647321306, 156.1079525116674631, -0.5547493173044985015 ) ) ;
#9733 = CARTESIAN_POINT ( 'NONE',  ( 4.310348487322937849, -12.41951052373176090, 1.878555342735434230 ) ) ;
#9734 = CARTESIAN_POINT ( 'NONE',  ( -5.036351857865265735, 117.3993844875897139, 0.5494637324817667201 ) ) ;
#9735 = CARTESIAN_POINT ( 'NONE',  ( 22.98488057257191741, 150.1591296352320910, 0.4592926148156237232 ) ) ;
#9736 = ORIENTED_EDGE ( 'NONE', *, *, #36593, .T. ) ;
#9737 = CARTESIAN_POINT ( 'NONE',  ( 4.617411384770501392, 7.639850289152962048, 0.2838591255797697777 ) ) ;
#9738 = CARTESIAN_POINT ( 'NONE',  ( -4.023493262646688606, 105.1225664206005916, 3.517815851256813175 ) ) ;
#9739 = FACE_OUTER_BOUND ( 'NONE', #32309, .T. ) ;
#9740 = CARTESIAN_POINT ( 'NONE',  ( -3.911441847776591096, 70.75305732235845824, -1.523999999999993804 ) ) ;
#9741 = EDGE_CURVE ( 'NONE', #38260, #12162, #27466, .T. ) ;
#9742 = CARTESIAN_POINT ( 'NONE',  ( 6.996320709379100222, 121.7437260403137884, 0.6222143296915167987 ) ) ;
#9743 = CARTESIAN_POINT ( 'NONE',  ( -4.556395268149300293, 8.773967715207941609, 0.7749943352582737699 ) ) ;
#9744 = CARTESIAN_POINT ( 'NONE',  ( 3.876365344914114441, 117.1932757116604762, 0.6224469224293306402 ) ) ;
#9745 = CARTESIAN_POINT ( 'NONE',  ( -0.05238710762259597004, 113.0327356262574341, 2.621665085262795625 ) ) ;
#9747 = CARTESIAN_POINT ( 'NONE',  ( 21.17963693554076343, 147.9292434580435724, -1.516351520135284625 ) ) ;
#9746 = CARTESIAN_POINT ( 'NONE',  ( 5.322370864742547170, 56.51500000000019952, 5.239063871132564998 ) ) ;
#9748 = TOROIDAL_SURFACE ( 'NONE', #12453, 3.683000000000000718, 0.5080000000000000071 ) ;
#9749 = CARTESIAN_POINT ( 'NONE',  ( 0.4327634382839667393, 5.975216699623357108, -4.620561613140377055 ) ) ;
#9750 = CARTESIAN_POINT ( 'NONE',  ( -21.41027608214069389, 151.3201912522522719, -1.490379992046949820 ) ) ;
#9751 = ORIENTED_EDGE ( 'NONE', *, *, #6848, .T. ) ;
#9752 = CIRCLE ( 'NONE', #30847, 2.540000000000004032 ) ;
#9753 = CARTESIAN_POINT ( 'NONE',  ( -10.50161782422445711, 126.1106773019354819, 0.1489875947030159797 ) ) ;
#9754 = EDGE_CURVE ( 'NONE', #5595, #8452, #12918, .T. ) ;
#9755 = CARTESIAN_POINT ( 'NONE',  ( 4.978007909399718045, -14.21992039213325398, 4.057701602070913793 ) ) ;
#9756 = DIRECTION ( 'NONE',  ( -0.000000000000000000, -0.000000000000000000, -1.000000000000000000 ) ) ;
#9757 = TOROIDAL_SURFACE ( 'NONE', #31522, 14.09699999999999420, 0.6350000000000000089 ) ;
#9758 = ADVANCED_FACE ( 'NONE', ( #2765 ), #15720, .T. ) ;
#9759 = ORIENTED_EDGE ( 'NONE', *, *, #18596, .T. ) ;
#9760 = CARTESIAN_POINT ( 'NONE',  ( 5.837434872614966963, 119.2401804501882197, 1.198870938642750739 ) ) ;
#9761 = FACE_OUTER_BOUND ( 'NONE', #8844, .T. ) ;
#9762 = CARTESIAN_POINT ( 'NONE',  ( -4.476425760464393555, 71.61790547347303004, -1.523999999999994248 ) ) ;
#9763 = CARTESIAN_POINT ( 'NONE',  ( -20.57308965805804846, 132.2049894596293313, 0.6677571715933803276 ) ) ;
#9764 = CARTESIAN_POINT ( 'NONE',  ( 0.9434990333792051542, 116.6346273530297850, -0.1892539897508099256 ) ) ;
#9765 = CARTESIAN_POINT ( 'NONE',  ( -5.941785710907115714, 57.15000000000771507, -5.016499999999997961 ) ) ;
#9766 = AXIS2_PLACEMENT_3D ( 'NONE', #33440, #27454, #1697 ) ;
#9767 = CARTESIAN_POINT ( 'NONE',  ( -5.009703114190266149, 117.5236796697281392, 0.6160668906261116406 ) ) ;
#9768 = CARTESIAN_POINT ( 'NONE',  ( -47.05348687143031583, 24.98710001375500056, 1.566218509541806636 ) ) ;
#9769 = CARTESIAN_POINT ( 'NONE',  ( 1.984180638160394139, -15.05580698533026762, 5.708628072855972846 ) ) ;
#9770 = CARTESIAN_POINT ( 'NONE',  ( -47.35944255389382818, 21.37623662739424191, 4.722871667523163453 ) ) ;
#9771 = LINE ( 'NONE', #35766, #19300 ) ;
#9772 = CARTESIAN_POINT ( 'NONE',  ( -4.622025190417427432, 118.0615168869452134, 0.5436107810192618572 ) ) ;
#9773 = CARTESIAN_POINT ( 'NONE',  ( 5.177913976931196594, 78.94499979771845233, 5.372100000000001430 ) ) ;
#9774 = ORIENTED_EDGE ( 'NONE', *, *, #37346, .T. ) ;
#9775 = FACE_OUTER_BOUND ( 'NONE', #15304, .T. ) ;
#9776 = CARTESIAN_POINT ( 'NONE',  ( 8.421875265154783463, 119.6416590919781697, -1.085143561374857457 ) ) ;
#9777 = CARTESIAN_POINT ( 'NONE',  ( -5.148946675964053199, 115.4673366222922368, -1.510641186666999980 ) ) ;
#9778 = CARTESIAN_POINT ( 'NONE',  ( 4.656206823194031230, 117.8897762713785227, 0.9969127701094048222 ) ) ;
#9779 = CARTESIAN_POINT ( 'NONE',  ( 1.824656174747253168, -15.25388738520313225, 5.420764384989097628 ) ) ;
#9780 = CARTESIAN_POINT ( 'NONE',  ( -7.125042791937310938, 121.7184703992695773, -0.7630849752878293701 ) ) ;
#9781 = CARTESIAN_POINT ( 'NONE',  ( -8.594951744493888768, 74.76616009375631222, -1.269999999999996909 ) ) ;
#9782 = CARTESIAN_POINT ( 'NONE',  ( -7.921807157844599878, 72.80702234259206307, 1.270000000000002682 ) ) ;
#9783 = CARTESIAN_POINT ( 'NONE',  ( 6.519249125050485816, 120.6419738463991536, -0.1350556763279781858 ) ) ;
#9784 = CARTESIAN_POINT ( 'NONE',  ( -14.69551782889057279, 134.6798445586954927, -1.826766161810339018 ) ) ;
#9785 = CARTESIAN_POINT ( 'NONE',  ( 4.808131379915037584, 104.6144662015457527, -0.4149153341867691802 ) ) ;
#9786 = CARTESIAN_POINT ( 'NONE',  ( -0.02156534543299366835, 156.6359106937186709, 1.079218069903262744 ) ) ;
#9787 = CARTESIAN_POINT ( 'NONE',  ( 5.578816284158309990, 56.51499999999997215, -4.418322536902425490 ) ) ;
#9788 = CARTESIAN_POINT ( 'NONE',  ( -11.83487444615315098, 152.0315182889855521, -0.1740310882773943024 ) ) ;
#9789 = CARTESIAN_POINT ( 'NONE',  ( 4.114294302962228755, -10.72644468530807416, -2.136776772127288559 ) ) ;
#9791 = ORIENTED_EDGE ( 'NONE', *, *, #38673, .T. ) ;
#9790 = CARTESIAN_POINT ( 'NONE',  ( 1.374325311229910307, 159.5643428290674990, 0.4556871491110247585 ) ) ;
#9792 = CARTESIAN_POINT ( 'NONE',  ( 5.218897159788115303, 104.6144662015501581, -1.155893325450091380 ) ) ;
#9793 = AXIS2_PLACEMENT_3D ( 'NONE', #35885, #10512, #39073 ) ;
#9794 = CARTESIAN_POINT ( 'NONE',  ( 2.845230715667840027, -15.32736664957809403, 4.381646938852296280 ) ) ;
#9795 = CIRCLE ( 'NONE', #15227, 8.794749999999996959 ) ;
#9796 = CARTESIAN_POINT ( 'NONE',  ( -13.42639911875441605, 154.0568829568526041, 1.747011766586976877 ) ) ;
#9797 = CARTESIAN_POINT ( 'NONE',  ( 0.3889013835376298744, 10.72134676413487142, 0.8939893681288630933 ) ) ;
#9798 = CARTESIAN_POINT ( 'NONE',  ( -8.168866085573604607, 117.6493956690293317, -0.5746791023534235654 ) ) ;
#9799 = CARTESIAN_POINT ( 'NONE',  ( -0.2932310942476468174, 5.691741097161698626, 0.9303163870417268111 ) ) ;
#9800 = VERTEX_POINT ( 'NONE', #6161 ) ;
#9801 = EDGE_LOOP ( 'NONE', ( #26149, #39152 ) ) ;
#9802 = CARTESIAN_POINT ( 'NONE',  ( -47.74911022259793469, 17.86741523025699152, 3.129844374475859947 ) ) ;
#9803 = CARTESIAN_POINT ( 'NONE',  ( 5.714359084451690940, 118.4654530710369329, 0.6612863029850992724 ) ) ;
#9804 = CARTESIAN_POINT ( 'NONE',  ( 34.28999999999999915, 0.000000000000000000, -1.040834085586084257E-14 ) ) ;
#9805 = CARTESIAN_POINT ( 'NONE',  ( -8.389933090069352062, 122.6561726160659731, 0.4454891811124967460 ) ) ;
#9806 = CARTESIAN_POINT ( 'NONE',  ( 3.930318996895993955, -12.97851325427171254, 2.595110522791146401 ) ) ;
#9807 = CARTESIAN_POINT ( 'NONE',  ( 0.8914275061359997476, 157.0053619834820324, -1.381823885352171377 ) ) ;
#9808 = AXIS2_PLACEMENT_3D ( 'NONE', #13444, #26004, #6427 ) ;
#9809 = CARTESIAN_POINT ( 'NONE',  ( -12.94126367519716325, 122.7019651155717384, -1.840448779276435687 ) ) ;
#9810 = FACE_OUTER_BOUND ( 'NONE', #38219, .T. ) ;
#9811 = ADVANCED_FACE ( 'NONE', ( #32134 ), #22309, .T. ) ;
#9812 = CARTESIAN_POINT ( 'NONE',  ( 8.158625645752934474, 120.6838676416457048, 1.398799808874931827 ) ) ;
#9813 = CARTESIAN_POINT ( 'NONE',  ( -3.430556142055666058, 34.24929622306240162, 1.944567991137617247 ) ) ;
#9814 = CARTESIAN_POINT ( 'NONE',  ( 11.25890738108741296, 128.1602342495223468, -0.05278459517149993591 ) ) ;
#9815 = ORIENTED_EDGE ( 'NONE', *, *, #23848, .T. ) ;
#9816 = DIRECTION ( 'NONE',  ( 5.206863593109713661E-17, -1.000000000000000000, 1.077750396879097183E-30 ) ) ;
#9817 = CARTESIAN_POINT ( 'NONE',  ( -14.95453923199683643, 61.75387968257833649, 5.016499999999999737 ) ) ;
#9818 = CARTESIAN_POINT ( 'NONE',  ( -58.82782897837036984, -0.2608788304230558186, 0.04583423360467810820 ) ) ;
#9819 = CARTESIAN_POINT ( 'NONE',  ( 1.650612623617701257E-15, 17.14499999999999957, 0.000000000000000000 ) ) ;
#9820 = CARTESIAN_POINT ( 'NONE',  ( 22.65966732694881358, 150.6414900647796173, 0.2998287813802534285 ) ) ;
#9821 = CARTESIAN_POINT ( 'NONE',  ( -4.844936406558586484, 112.7696648386057632, 2.375766922042533036 ) ) ;
#9822 = DIRECTION ( 'NONE',  ( -0.9998004120163608288, 0.000000000000000000, -0.01997839162482747608 ) ) ;
#9823 = CARTESIAN_POINT ( 'NONE',  ( -6.540217103314379345E-14, 82.64346620154573486, 2.383338306179204368E-29 ) ) ;
#9824 = CARTESIAN_POINT ( 'NONE',  ( -5.176850267262477878, 31.60528704468920580, -0.07969122161898606338 ) ) ;
#9825 = CARTESIAN_POINT ( 'NONE',  ( 1.137402291071409444, 117.9723128000925669, 0.6313431152059614249 ) ) ;
#9826 = CARTESIAN_POINT ( 'NONE',  ( 2.029292378383023898, 15.02103924000656043, -4.168288449772576065 ) ) ;
#9827 = CARTESIAN_POINT ( 'NONE',  ( 1.249529592346430240, 29.00528243095578063, -8.330927077797271707 ) ) ;
#9828 = CARTESIAN_POINT ( 'NONE',  ( 5.510702963104994190, 117.2606150369192477, -0.6137602300856868087 ) ) ;
#9829 = CARTESIAN_POINT ( 'NONE',  ( -1.618304973946187664, 119.5945091202099348, -0.6420790694971422186 ) ) ;
#9830 = FACE_OUTER_BOUND ( 'NONE', #4547, .T. ) ;
#9831 = DIRECTION ( 'NONE',  ( 5.188838149069472160E-16, -1.699382548006136559E-16, -1.000000000000000000 ) ) ;
#9832 = CARTESIAN_POINT ( 'NONE',  ( 1.041310694616567556, 104.6144662015456817, 4.721824807668626889 ) ) ;
#9833 = CARTESIAN_POINT ( 'NONE',  ( 0.4746723515649934888, 24.68197512780947278, 4.609222710213416896 ) ) ;
#9834 = DIRECTION ( 'NONE',  ( -0.01997839162482749689, -1.040247600000944870E-18, 0.9998004120163610509 ) ) ;
#9835 = CARTESIAN_POINT ( 'NONE',  ( -15.47023807670837314, 120.6682698389898434, -0.3091321738930619678 ) ) ;
#9836 = CARTESIAN_POINT ( 'NONE',  ( 2.663950356258127705, -13.19741034273377878, 0.1528337951401303463 ) ) ;
#9837 = CARTESIAN_POINT ( 'NONE',  ( 3.079316153087777508, 123.1875568577169560, -0.05586128712921770156 ) ) ;
#9838 = CARTESIAN_POINT ( 'NONE',  ( -15.09612904044937487, 120.9194639129320734, 0.3833380168901106555 ) ) ;
#9839 = ORIENTED_EDGE ( 'NONE', *, *, #18824, .F. ) ;
#9840 = CARTESIAN_POINT ( 'NONE',  ( 5.177913976931193041, 88.73331249999999670, 5.372100000000000541 ) ) ;
#9841 = ORIENTED_EDGE ( 'NONE', *, *, #2962, .F. ) ;
#9842 = DIRECTION ( 'NONE',  ( 0.1565721916418019999, 0.9876665170007956629, -8.659954811667593930E-17 ) ) ;
#9843 = CARTESIAN_POINT ( 'NONE',  ( 6.046978665186544255, -14.69723126592269224, 0.3844556930898083702 ) ) ;
#9844 = CARTESIAN_POINT ( 'NONE',  ( -18.00466200016603580, 151.7072807693909340, 1.676127293294198850 ) ) ;
#9845 = CARTESIAN_POINT ( 'NONE',  ( 7.282534483022669036, 158.3006260280594404, -1.262407574188499026 ) ) ;
#9846 = CARTESIAN_POINT ( 'NONE',  ( 0.3994026957563919789, 5.465888722076803319, 4.619092260001838923 ) ) ;
#9847 = CARTESIAN_POINT ( 'NONE',  ( -58.77082881926929048, -0.3034670599615398867, -0.1967669022685080149 ) ) ;
#9848 = ORIENTED_EDGE ( 'NONE', *, *, #23204, .T. ) ;
#9849 = CARTESIAN_POINT ( 'NONE',  ( -11.66725022231030984, 17.14499999999999957, -5.016499999999999737 ) ) ;
#9850 = CARTESIAN_POINT ( 'NONE',  ( 0.4207377039450588829, 124.6436471961814050, 0.04080923199211386465 ) ) ;
#9851 = CARTESIAN_POINT ( 'NONE',  ( -16.99563481483670913, 148.6336825499269310, 1.463981761124606207 ) ) ;
#9852 = DIRECTION ( 'NONE',  ( 0.6294287539883844929, 0.7770581983690987293, 0.000000000000000000 ) ) ;
#9853 = CARTESIAN_POINT ( 'NONE',  ( 2.342076541036470783, 157.5529522918930638, -1.611985001046909005 ) ) ;
#9854 = CARTESIAN_POINT ( 'NONE',  ( -13.73566407960812263, 122.1113760975138263, -1.718532046871276808 ) ) ;
#9855 = CARTESIAN_POINT ( 'NONE',  ( -58.10099831372669854, 0.3475205698689753930, -0.9728495803591354907 ) ) ;
#9856 = ORIENTED_EDGE ( 'NONE', *, *, #10274, .T. ) ;
#9857 = CARTESIAN_POINT ( 'NONE',  ( 4.423891049316628354, 118.1653506322867173, -0.4723435439479501396 ) ) ;
#9858 = CARTESIAN_POINT ( 'NONE',  ( 16.08279055836830906, 146.6973543426590254, -0.5313625374031879511 ) ) ;
#9859 = ORIENTED_EDGE ( 'NONE', *, *, #28255, .F. ) ;
#9860 = CARTESIAN_POINT ( 'NONE',  ( -12.73281086834439257, 125.9836878220586556, -1.772748636948828782 ) ) ;
#9861 = CARTESIAN_POINT ( 'NONE',  ( 3.418015357486716699, -15.48303273933827917, 3.654867857709153345 ) ) ;
#9862 = CARTESIAN_POINT ( 'NONE',  ( -4.622786458448389091, 105.1214642455587978, -2.684754972049111732 ) ) ;
#9863 = CARTESIAN_POINT ( 'NONE',  ( -57.89731077922513691, 0.5615449381113218896, -1.034775302914740585E-14 ) ) ;
#9864 = VECTOR ( 'NONE', #28268, 1000.000000000000000 ) ;
#9865 = CARTESIAN_POINT ( 'NONE',  ( -4.773351466264551313, 117.6315869056820418, 0.9547913690014270260 ) ) ;
#9866 = CARTESIAN_POINT ( 'NONE',  ( 17.50754485026800111, 146.9817191466759141, 2.164442782320840752 ) ) ;
#9867 = DIRECTION ( 'NONE',  ( -0.7445787077807538568, -0.6675346791886865860, 0.000000000000000000 ) ) ;
#9868 = CARTESIAN_POINT ( 'NONE',  ( 1.790774717077139089, 25.13178105314743860, 4.274281468382033822 ) ) ;
#9869 = CARTESIAN_POINT ( 'NONE',  ( 15.27574012874717191, 148.0141687878753203, 0.5334971086861887146 ) ) ;
#9870 = CARTESIAN_POINT ( 'NONE',  ( -49.01671973967521012, 18.67808020721676954, -5.174630477995056488 ) ) ;
#9871 = CARTESIAN_POINT ( 'NONE',  ( -48.96835380800505533, 15.76965437727898056, -2.261121166259650650 ) ) ;
#9872 = DIRECTION ( 'NONE',  ( 5.188838149069472160E-16, -1.699382548006136559E-16, -1.000000000000000000 ) ) ;
#9873 = DIRECTION ( 'NONE',  ( 5.188838149069472160E-16, -1.699382548006136559E-16, -1.000000000000000000 ) ) ;
#9874 = CARTESIAN_POINT ( 'NONE',  ( -47.04217617083259029, 23.73857702128102076, 2.948847133965281309 ) ) ;
#9875 = FACE_OUTER_BOUND ( 'NONE', #13763, .T. ) ;
#9876 = CARTESIAN_POINT ( 'NONE',  ( -8.762201071066225921, 117.8145929003731425, -0.5758305771568995590 ) ) ;
#9877 = CARTESIAN_POINT ( 'NONE',  ( -5.664977208693910526, 77.01756250000002524, 5.033228321271210781 ) ) ;
#9878 = CARTESIAN_POINT ( 'NONE',  ( -4.074955089416341991, 118.2429491485453354, 0.1454234154749719787 ) ) ;
#9879 = CARTESIAN_POINT ( 'NONE',  ( -17.14500000000466784, 71.11999999999886768, -1.270000000000000684 ) ) ;
#9880 = CARTESIAN_POINT ( 'NONE',  ( -55.59033409382031721, 8.645621179197947370, 1.431546819705146634 ) ) ;
#9881 = CARTESIAN_POINT ( 'NONE',  ( -55.60486134785667645, 7.243031971518515633, 3.140198620020484110 ) ) ;
#9882 = CARTESIAN_POINT ( 'NONE',  ( -0.3151558924359575409, 116.5752054743899038, 0.1523977429619430557 ) ) ;
#9883 = ORIENTED_EDGE ( 'NONE', *, *, #2992, .T. ) ;
#9884 = CARTESIAN_POINT ( 'NONE',  ( -53.04800011021367112, 17.61732480354184815, -1.091987273408484482E-14 ) ) ;
#9885 = CARTESIAN_POINT ( 'NONE',  ( 6.970729396409415024, 121.9486231262834934, 0.03295389407336209164 ) ) ;
#9886 = ORIENTED_EDGE ( 'NONE', *, *, #4338, .T. ) ;
#9887 = CARTESIAN_POINT ( 'NONE',  ( 3.613157353203237054, 115.7029504961088122, -1.483779985806342294 ) ) ;
#9888 = CARTESIAN_POINT ( 'NONE',  ( -10.42406139656922548, 153.0845720789597522, -0.4157246174923901472 ) ) ;
#9889 = CARTESIAN_POINT ( 'NONE',  ( 5.566531978545880222, -14.14111126781847361, 3.212028819027522797 ) ) ;
#9890 = CARTESIAN_POINT ( 'NONE',  ( -3.062634247293312129, 117.6993298527280984, 0.6308921261198922048 ) ) ;
#9891 = CARTESIAN_POINT ( 'NONE',  ( 5.892673590944617956, 78.88814725119658533, -5.017439957471150791 ) ) ;
#9892 = CARTESIAN_POINT ( 'NONE',  ( 1.404208078696223216, 159.5982469381528972, 0.2156159867753337234 ) ) ;
#9893 = CARTESIAN_POINT ( 'NONE',  ( 5.325826159991753350, 121.3512792334589534, 0.1791233883900909540 ) ) ;
#9894 = DIRECTION ( 'NONE',  ( -0.7258741224889101451, 0.6878275643654844229, -8.537024980200846470E-16 ) ) ;
#9895 = CARTESIAN_POINT ( 'NONE',  ( -0.9163883642843115851, 13.89126970375589032, 0.3362141533434955809 ) ) ;
#9896 = CARTESIAN_POINT ( 'NONE',  ( -23.18927481933092594, 149.6199392087789306, -0.6935230913228406235 ) ) ;
#9897 = CARTESIAN_POINT ( 'NONE',  ( -17.14500000000466784, 71.11999999999886768, 1.269999999999998241 ) ) ;
#9898 = FACE_OUTER_BOUND ( 'NONE', #29952, .T. ) ;
#9899 = ORIENTED_EDGE ( 'NONE', *, *, #23307, .T. ) ;
#9900 = AXIS2_PLACEMENT_3D ( 'NONE', #27812, #40820, #5463 ) ;
#9901 = CARTESIAN_POINT ( 'NONE',  ( -5.566147196004182618, 117.2876211984145698, 0.5856085228032834600 ) ) ;
#9902 = ORIENTED_EDGE ( 'NONE', *, *, #41610, .T. ) ;
#9903 = DIRECTION ( 'NONE',  ( 5.188838149069472160E-16, -1.699382548006136559E-16, -1.000000000000000000 ) ) ;
#9904 = CARTESIAN_POINT ( 'NONE',  ( 21.34910226488267782, 149.1985357531029308, 2.237902092811237864 ) ) ;
#9905 = CARTESIAN_POINT ( 'NONE',  ( 17.46960851010910432, 131.6241255656270255, -1.599527815159631716 ) ) ;
#9906 = CARTESIAN_POINT ( 'NONE',  ( -0.6470182227010313758, 8.987660258844066163, 0.7316552229444387434 ) ) ;
#9907 = CARTESIAN_POINT ( 'NONE',  ( 2.011605530963595623, 11.37297026005182587, 8.215081034461865883 ) ) ;
#9908 = CARTESIAN_POINT ( 'NONE',  ( -5.110479671343788333, 158.7070047875298826, -1.445852496635407380 ) ) ;
#9909 = CARTESIAN_POINT ( 'NONE',  ( 4.833421569118034888, 117.8347370731485597, -0.7197543954735053928 ) ) ;
#9910 = ADVANCED_FACE ( 'NONE', ( #9761 ), #2440, .F. ) ;
#9911 = CARTESIAN_POINT ( 'NONE',  ( -0.1065646865916381608, 105.8844662015456777, 5.332932678536313809 ) ) ;
#9912 = ADVANCED_FACE ( 'NONE', ( #35966 ), #39160, .F. ) ;
#9913 = CARTESIAN_POINT ( 'NONE',  ( 5.165015969722777989, 120.6777149489875569, -0.5489573293230838313 ) ) ;
#9914 = CARTESIAN_POINT ( 'NONE',  ( -8.794423163103219920, 123.6850765633735421, -0.1423839433359066764 ) ) ;
#9915 = ORIENTED_EDGE ( 'NONE', *, *, #12125, .F. ) ;
#9916 = CARTESIAN_POINT ( 'NONE',  ( -15.71196619591404620, 131.3838724160208926, -2.228970979916469197 ) ) ;
#9917 = CARTESIAN_POINT ( 'NONE',  ( 2.810429210790068133, -15.63944505633836712, 5.584101034811558506 ) ) ;
#9918 = APPLICATION_CONTEXT ( 'automotive_design' ) ;
#9919 = CARTESIAN_POINT ( 'NONE',  ( -6.529493367164978770E-14, 72.99146620154573384, -7.899616498973244731E-18 ) ) ;
#9920 = CARTESIAN_POINT ( 'NONE',  ( -47.87216941255763203, 19.82042534259524658, -5.426529464407940928 ) ) ;
#9921 = ORIENTED_EDGE ( 'NONE', *, *, #15276, .T. ) ;
#9922 = B_SPLINE_SURFACE_WITH_KNOTS ( 'NONE', 3, 3, ( 
 ( #36739, #10536, #33337, #26729, #4167, #7562 ),
 ( #20736, #3960, #39946, #30330, #30546, #30131 ),
 ( #760, #23505, #17130, #27143, #33760, #39521 ),
 ( #1385, #36532, #26515, #10740, #23936, #17341 ) ),
 .UNSPECIFIED., .F., .F., .F.,
 ( 4, 4 ),
 ( 4, 2, 4 ),
 ( 0.000000000000000000, 1.000000000000000000 ),
 ( 0.000000000000000000, 0.5000000000000000000, 1.000000000000000000 ),
 .UNSPECIFIED. ) ;
#9923 = CARTESIAN_POINT ( 'NONE',  ( 17.40616913868953475, 140.3598469681121514, 2.385085200778920278 ) ) ;
#9924 = FACE_OUTER_BOUND ( 'NONE', #958, .T. ) ;
#9925 = CARTESIAN_POINT ( 'NONE',  ( -6.439947148575337965E-14, 116.4254662015457313, 1.493913655526859821E-16 ) ) ;
#9926 = CARTESIAN_POINT ( 'NONE',  ( -1.389742127967517504, 109.2701902778323557, 3.915166117862841411 ) ) ;
#9927 = CARTESIAN_POINT ( 'NONE',  ( 0.2611430735369592582, 24.48315862702271417, 8.432237392808469068 ) ) ;
#9928 = CARTESIAN_POINT ( 'NONE',  ( 9.499123264218818363, 124.0643708016488063, 0.7086372128104245771 ) ) ;
#9929 = CIRCLE ( 'NONE', #5212, 0.2539999999999998925 ) ;
#9930 = CARTESIAN_POINT ( 'NONE',  ( 16.46484310285434205, 122.7513851185756693, -0.4780162726406276819 ) ) ;
#9931 = DIRECTION ( 'NONE',  ( -5.188838149069471174E-16, 1.699382548006136313E-16, 1.000000000000000000 ) ) ;
#9932 = CARTESIAN_POINT ( 'NONE',  ( 6.475684456959278634, -13.49251406434824574, 0.1304084665236045215 ) ) ;
#9933 = EDGE_CURVE ( 'NONE', #13136, #18529, #37646, .T. ) ;
#9934 = CARTESIAN_POINT ( 'NONE',  ( -10.83330528665015891, 157.8980211815716928, -0.2164752214609687586 ) ) ;
#9935 = EDGE_LOOP ( 'NONE', ( #7924, #8848, #37061, #15277 ) ) ;
#9936 = CARTESIAN_POINT ( 'NONE',  ( -7.991460488516994864, 121.5207739338980275, -1.170844661440724632 ) ) ;
#9937 = CARTESIAN_POINT ( 'NONE',  ( 4.984401644025001410, -14.86135559163349384, 4.129797103419615922 ) ) ;
#9938 = CARTESIAN_POINT ( 'NONE',  ( -11.46436990449512727, 128.2561452373498980, -0.7395913538610450200 ) ) ;
#9939 = CARTESIAN_POINT ( 'NONE',  ( 2.668130780779813360, -14.68804970414791455, 5.313657848291281738 ) ) ;
#9940 = CARTESIAN_POINT ( 'NONE',  ( -6.564189886853176475E-14, 81.62746620154572952, -5.847435218134868453E-18 ) ) ;
#9941 = CARTESIAN_POINT ( 'NONE',  ( 21.68875320759051917, 132.7412702629105468, 0.4333929054516009183 ) ) ;
#9942 = ORIENTED_EDGE ( 'NONE', *, *, #9157, .T. ) ;
#9943 = CARTESIAN_POINT ( 'NONE',  ( -4.609222696788063622, 3.091975128091568159, 0.4746723485708761459 ) ) ;
#9944 = CARTESIAN_POINT ( 'NONE',  ( 5.287133221413552242, 105.1224873763950143, 0.7811871516068193966 ) ) ;
#9945 = CARTESIAN_POINT ( 'NONE',  ( -4.902043024275339000, 117.4095900847628826, 0.9678312229368277730 ) ) ;
#9946 = CARTESIAN_POINT ( 'NONE',  ( 4.403693129465371392, 110.7916611705323504, 3.072783695400131521 ) ) ;
#9947 = CARTESIAN_POINT ( 'NONE',  ( 6.990161945763603057, 121.8758651151647854, 0.4345305272952283415 ) ) ;
#9948 = CARTESIAN_POINT ( 'NONE',  ( -3.984361711520921556, 7.699456178644025428, -2.362637291489932068 ) ) ;
#9949 = CARTESIAN_POINT ( 'NONE',  ( 11.19826879832059241, 119.1264784044212632, 1.044736191152864313 ) ) ;
#9950 = CARTESIAN_POINT ( 'NONE',  ( -7.213960532363674183, 86.35999999999998522, -1.904999999999999805 ) ) ;
#9952 = CARTESIAN_POINT ( 'NONE',  ( 10.51304382037001162, 120.0128241960130424, -1.064055063733757134 ) ) ;
#9951 = CARTESIAN_POINT ( 'NONE',  ( 2.116451952768004130, 107.0587250333981615, 4.811125309486601331 ) ) ;
#9953 = CARTESIAN_POINT ( 'NONE',  ( 4.623297697159335584, 3.588818502778304609, 0.3943307014320480697 ) ) ;
#9954 = CARTESIAN_POINT ( 'NONE',  ( -21.93197806114495307, 150.5960492154097778, -1.608405794939391509 ) ) ;
#9955 = VECTOR ( 'NONE', #16115, 1000.000000000000114 ) ;
#9956 = ADVANCED_FACE ( 'NONE', ( #32340 ), #37208, .F. ) ;
#9957 = EDGE_LOOP ( 'NONE', ( #35939, #10268, #5428, #18809 ) ) ;
#9958 = VECTOR ( 'NONE', #26969, 1000.000000000000227 ) ;
#9959 = CARTESIAN_POINT ( 'NONE',  ( -15.87385217746184729, 146.2799285973741519, 0.1369075966739885519 ) ) ;
#9960 = CARTESIAN_POINT ( 'NONE',  ( 6.023256536641487635, -13.63339314725699225, 2.031454315062427796 ) ) ;
#9961 = DIRECTION ( 'NONE',  ( 0.9998004120163608288, 0.000000000000000000, 0.01997839162482749342 ) ) ;
#9962 = CARTESIAN_POINT ( 'NONE',  ( -2.894375511602795381, 107.8343606798795093, -4.471999567165577005 ) ) ;
#9963 = EDGE_CURVE ( 'NONE', #30709, #27023, #13378, .T. ) ;
#9964 = VERTEX_POINT ( 'NONE', #41736 ) ;
#9965 = CARTESIAN_POINT ( 'NONE',  ( 15.45413117217001542, 153.1703808545849483, 2.356132421238607222 ) ) ;
#9966 = DIRECTION ( 'NONE',  ( 0.9876665170007969952, -0.1565721916417935344, 5.390917751951444915E-16 ) ) ;
#9967 = CARTESIAN_POINT ( 'NONE',  ( -9.909999474182706436, 76.95545850745379823, -1.269999999999998019 ) ) ;
#9968 = CARTESIAN_POINT ( 'NONE',  ( -14.68046753700562412, 156.0817623197167450, 0.7569547985229808651 ) ) ;
#9969 = CARTESIAN_POINT ( 'NONE',  ( 8.004298179822232129, 158.6817341734954425, -0.1651967042931133389 ) ) ;
#9970 = CARTESIAN_POINT ( 'NONE',  ( -6.059261036834476144, 56.51499999999998636, -5.016499999999990855 ) ) ;
#9971 = AXIS2_PLACEMENT_3D ( 'NONE', #19541, #3169, #41944 ) ;
#9972 = CARTESIAN_POINT ( 'NONE',  ( -48.37037162488499575, 18.71529471574935499, 5.180666589218357210 ) ) ;
#9973 = CARTESIAN_POINT ( 'NONE',  ( -47.22545206610593027, 24.52529105818055655, 1.461865184087808966 ) ) ;
#9974 = CARTESIAN_POINT ( 'NONE',  ( -4.757280042987765967, 117.4019780031357527, -1.206666893366715065 ) ) ;
#9975 = CARTESIAN_POINT ( 'NONE',  ( -50.58884987432006852, 15.93229845861179861, 5.010371253631904942 ) ) ;
#9976 = CARTESIAN_POINT ( 'NONE',  ( -58.82993613934316812, -0.2576853927351192564, 0.02220333243337114723 ) ) ;
#9977 = CARTESIAN_POINT ( 'NONE',  ( -4.731020071145249695, 117.9657514467067472, 0.6165449125908130101 ) ) ;
#9978 = DIRECTION ( 'NONE',  ( -0.5149185422762269093, 0.8572391118119411235, 5.959261578127985974E-15 ) ) ;
#9979 = AXIS2_PLACEMENT_3D ( 'NONE', #18191, #2036, #5663 ) ;
#9980 = ORIENTED_EDGE ( 'NONE', *, *, #21698, .T. ) ;
#9981 = CARTESIAN_POINT ( 'NONE',  ( -1.364642409907909748, 118.7629491485454167, -1.251955028465520980 ) ) ;
#9982 = EDGE_CURVE ( 'NONE', #9488, #8589, #40011, .T. ) ;
#9983 = CARTESIAN_POINT ( 'NONE',  ( -3.548838988669358319, 118.7219257611751857, -0.9358992106884462814 ) ) ;
#9984 = CARTESIAN_POINT ( 'NONE',  ( -5.714359084451818838, 118.4654530710369329, -0.6612863029850992724 ) ) ;
#9985 = CARTESIAN_POINT ( 'NONE',  ( 4.776791126193284498, 117.8777007509519024, 0.8660848876855279377 ) ) ;
#9986 = CARTESIAN_POINT ( 'NONE',  ( -46.69554899239189183, 26.06112269829689865, -0.4657571695567720438 ) ) ;
#9987 = CARTESIAN_POINT ( 'NONE',  ( -16.04436118421920199, 148.0691544347876345, -1.589228464704729005 ) ) ;
#9988 = DIRECTION ( 'NONE',  ( 3.035386659626960118E-16, -0.000000000000000000, 1.000000000000000000 ) ) ;
#9989 = EDGE_CURVE ( 'NONE', #25607, #6738, #13491, .T. ) ;
#9990 = DIRECTION ( 'NONE',  ( 5.188838149069472160E-16, -1.699382548006136559E-16, -1.000000000000000000 ) ) ;
#9991 = CARTESIAN_POINT ( 'NONE',  ( 7.643893061813482603, 124.7210964017841377, 0.1527835634684689414 ) ) ;
#9992 = CARTESIAN_POINT ( 'NONE',  ( -16.79675997928907449, 147.6865045845431723, -1.918872074639297098 ) ) ;
#9993 = DIRECTION ( 'NONE',  ( 0.9336303900108808840, 0.3582377630124027879, -6.739313779395947471E-16 ) ) ;
#9994 = CARTESIAN_POINT ( 'NONE',  ( -0.01341678693510457362, 156.4123495908283985, 0.6714308817992611367 ) ) ;
#9995 = CARTESIAN_POINT ( 'NONE',  ( 7.862390625383989473, 122.3040693739171587, -0.4082539146964299648 ) ) ;
#9996 = CARTESIAN_POINT ( 'NONE',  ( -15.20866760725288103, 143.4108773460236819, -0.2363331269315028793 ) ) ;
#9997 = CARTESIAN_POINT ( 'NONE',  ( 2.551540157903699146, -0.3564265548712530207, -3.854280124997286450 ) ) ;
#9999 = ORIENTED_EDGE ( 'NONE', *, *, #28468, .F. ) ;
#9998 = CARTESIAN_POINT ( 'NONE',  ( 22.36400590086632434, 150.5530013069706285, 1.293239838729947300 ) ) ;
#10000 = CARTESIAN_POINT ( 'NONE',  ( 13.46199999999999797, 12.17394877578616885, 0.000000000000000000 ) ) ;
#10001 = CARTESIAN_POINT ( 'NONE',  ( 3.395721326281507579, -14.88725931823228699, 0.4187095049187871121 ) ) ;
#10002 = CARTESIAN_POINT ( 'NONE',  ( -0.03245814172817904769, 157.7902383798253538, 1.624338139048501883 ) ) ;
#10003 = CARTESIAN_POINT ( 'NONE',  ( 0.8415213475290624912, 13.30065917492326122, -0.4928529130785159751 ) ) ;
#10004 = CARTESIAN_POINT ( 'NONE',  ( -13.28278499026800752, 156.9705208988102640, -0.7618315876160809408 ) ) ;
#10005 = VECTOR ( 'NONE', #12477, 1000.000000000000000 ) ;
#10006 = CARTESIAN_POINT ( 'NONE',  ( 0.8610934044332675397, -11.37225059697985863, 0.4573394443077089533 ) ) ;
#10007 = EDGE_LOOP ( 'NONE', ( #15754, #10890, #18680, #17695 ) ) ;
#10008 = ORIENTED_EDGE ( 'NONE', *, *, #22058, .F. ) ;
#10009 = CARTESIAN_POINT ( 'NONE',  ( -45.15528325240633478, 20.88806775524793125, 3.529375091719462176 ) ) ;
#10010 = EDGE_CURVE ( 'NONE', #5685, #24684, #2526, .T. ) ;
#10011 = CARTESIAN_POINT ( 'NONE',  ( 5.397835693418270964, 119.2618716387835747, 0.5632668535983703650 ) ) ;
#10012 = CARTESIAN_POINT ( 'NONE',  ( -15.71237885704647752, 143.6801599334541208, 0.6671153439278900699 ) ) ;
#10013 = CARTESIAN_POINT ( 'NONE',  ( 2.527534073033691708, -14.76126024938119485, 5.399385249886175409 ) ) ;
#10014 = CARTESIAN_POINT ( 'NONE',  ( 13.68689207195642332, 152.4534842159446271, -1.543072478675916459 ) ) ;
#10015 = VECTOR ( 'NONE', #20543, 1000.000000000000227 ) ;
#10016 = CARTESIAN_POINT ( 'NONE',  ( -6.695514854630728152, 119.3011930948910759, -1.284729283498812435 ) ) ;
#10017 = CARTESIAN_POINT ( 'NONE',  ( -6.555005513994535572E-14, 79.34146620154574236, -6.390659674827382268E-18 ) ) ;
#10018 = CARTESIAN_POINT ( 'NONE',  ( 2.829627719599027369, -13.65247383265987757, 0.5238048331051645690 ) ) ;
#10019 = CARTESIAN_POINT ( 'NONE',  ( -5.860682609351126615, 31.62183355753281333, 2.274222983814665699 ) ) ;
#10020 = CARTESIAN_POINT ( 'NONE',  ( 10.45649748849128713, 153.0728660266736370, -0.08902316335936723279 ) ) ;
#10021 = AXIS2_PLACEMENT_3D ( 'NONE', #4108, #39883, #36471 ) ;
#10022 = ORIENTED_EDGE ( 'NONE', *, *, #10189, .T. ) ;
#10023 = CARTESIAN_POINT ( 'NONE',  ( -12.69999999999999574, 16.51000000000000156, 0.000000000000000000 ) ) ;
#10024 = CARTESIAN_POINT ( 'NONE',  ( 0.4435697013598551841, 106.0197932915369847, 5.281582295280689898 ) ) ;
#10025 = DIRECTION ( 'NONE',  ( -0.8745520943968236871, 0.4849315768086559508, -6.829619984160659032E-16 ) ) ;
#10026 = LINE ( 'NONE', #10449, #16344 ) ;
#10027 = EDGE_CURVE ( 'NONE', #700, #16922, #31850, .T. ) ;
#10028 = CARTESIAN_POINT ( 'NONE',  ( 15.19006826215911587, 156.0999766016731769, 0.2361313609475710340 ) ) ;
#10029 = CARTESIAN_POINT ( 'NONE',  ( -5.498174961348694545, 117.5088849381099436, 0.6086507346144035546 ) ) ;
#10030 = AXIS2_PLACEMENT_3D ( 'NONE', #9434, #12633, #16444 ) ;
#10031 = DIRECTION ( 'NONE',  ( -0.9998004120163609398, 0.000000000000000000, -0.01997839162482749689 ) ) ;
#10032 = DIRECTION ( 'NONE',  ( -1.000000000000000000, -1.092739197465705287E-15, 0.000000000000000000 ) ) ;
#10033 = CARTESIAN_POINT ( 'NONE',  ( -4.187219683869615849, 32.60936066482102547, 1.105729851008191877 ) ) ;
#10034 = CARTESIAN_POINT ( 'NONE',  ( 13.40516742707908726, 121.5866728338796463, 1.646856811522066311 ) ) ;
#10035 = CARTESIAN_POINT ( 'NONE',  ( -4.488006035213030209, 18.49445617864287073, 1.146732334616328286 ) ) ;
#10036 = CARTESIAN_POINT ( 'NONE',  ( -7.485859564062662841, -11.32103332335322499, -3.896386919873200405 ) ) ;
#10037 = CARTESIAN_POINT ( 'NONE',  ( 5.515726608291020128, 117.1379768558993817, -0.5451333893821521670 ) ) ;
#10038 = CARTESIAN_POINT ( 'NONE',  ( -0.7127221660107545542, 117.6736730875354766, -1.182500608623780813 ) ) ;
#10039 = CARTESIAN_POINT ( 'NONE',  ( 20.83467972660109169, 65.95194780259438971, 5.016499999999999737 ) ) ;
#10040 = CARTESIAN_POINT ( 'NONE',  ( -2.864695162364617076, 104.6144662015458096, 3.894373788996692287 ) ) ;
#10041 = CARTESIAN_POINT ( 'NONE',  ( -4.420329592304260480, 21.65838872207745425, -1.398650104627336743 ) ) ;
#10042 = EDGE_CURVE ( 'NONE', #23250, #33175, #29354, .T. ) ;
#10043 = LINE ( 'NONE', #42021, #40946 ) ;
#10044 = DIRECTION ( 'NONE',  ( 0.9876665170007953298, -0.1565721916418034432, 5.390917751951452804E-16 ) ) ;
#10045 = CARTESIAN_POINT ( 'NONE',  ( 2.351750233177451133, -15.05367847713771923, 4.985144330900271648 ) ) ;
#10046 = CARTESIAN_POINT ( 'NONE',  ( 2.822804308802433493, 121.9077826007922312, -0.1826741318641919576 ) ) ;
#10047 = CARTESIAN_POINT ( 'NONE',  ( -0.3352962839985075827, 116.7787044104018861, 0.2500268678974715830 ) ) ;
#10048 = ADVANCED_FACE ( 'NONE', ( #29574 ), #26366, .F. ) ;
#10049 = CARTESIAN_POINT ( 'NONE',  ( 4.976171711130020547, 117.4097491279395626, -0.8839812355984283387 ) ) ;
#10050 = ORIENTED_EDGE ( 'NONE', *, *, #41743, .F. ) ;
#10051 = CARTESIAN_POINT ( 'NONE',  ( 5.008145224984434485, 117.3993836135855418, -0.7758584094373792706 ) ) ;
#10052 = ORIENTED_EDGE ( 'NONE', *, *, #27169, .F. ) ;
#10053 = CARTESIAN_POINT ( 'NONE',  ( -5.274544067074300457, 115.7029491485454002, 0.8135768287290441325 ) ) ;
#10054 = CARTESIAN_POINT ( 'NONE',  ( 3.756887254765235440, -15.74060793811991843, 4.623245420838687281 ) ) ;
#10055 = CARTESIAN_POINT ( 'NONE',  ( -12.27107220260967857, 121.7247091083657153, 1.253333917061305147 ) ) ;
#10056 = CARTESIAN_POINT ( 'NONE',  ( 15.58647730463667536, 154.9569273371780298, -1.293949759430877533 ) ) ;
#10057 = CARTESIAN_POINT ( 'NONE',  ( 4.617411384770501392, 7.639850289152962048, 0.2838591255797697777 ) ) ;
#10058 = CARTESIAN_POINT ( 'NONE',  ( -58.63621593477581229, -0.3005977173826933635, -0.3593407213355099827 ) ) ;
#10059 = VERTEX_POINT ( 'NONE', #23578 ) ;
#10060 = CARTESIAN_POINT ( 'NONE',  ( -4.771056762337200219, 117.4047813638584188, -1.203986021773440385 ) ) ;
#10061 = B_SPLINE_CURVE_WITH_KNOTS ( 'NONE', 3,
 ( #12394, #6013, #25583, #2191, #2402, #18342, #34559, #40947, #28368, #9398, #6218, #31136, #15148, #41158, #24740, #11964, #27940 ),
 .UNSPECIFIED., .F., .F.,
 ( 4, 1, 1, 1, 1, 1, 1, 1, 1, 1, 1, 1, 1, 1, 4 ),
 ( 0.000000000000000000, 0.08300113939718137268, 0.1732806554784933895, 0.2717672377176819087, 0.3752096606209606167, 0.4787223716043260135, 0.5772295444745598747, 0.6668133826162351285, 0.7470991451079272982, 0.7815930070524458317, 0.8169452614683294644, 0.8547689062991584708, 0.8968063284581728745, 0.9447228702782888288, 1.000000000000000000 ),
 .UNSPECIFIED. ) ;
#10062 = CARTESIAN_POINT ( 'NONE',  ( 0.4574053846281739832, 111.1955024190080223, 3.269098021338873838 ) ) ;
#10063 = CARTESIAN_POINT ( 'NONE',  ( -16.86000824444456470, 147.6865045845431723, 1.246329746872388622 ) ) ;
#10064 = CARTESIAN_POINT ( 'NONE',  ( -46.85406979095059654, 20.44882429329730655, 5.016006923199691769 ) ) ;
#10065 = CARTESIAN_POINT ( 'NONE',  ( 2.279834263381187220, 157.4004113605966211, -1.585270110160261536 ) ) ;
#10066 = CARTESIAN_POINT ( 'NONE',  ( -0.4162271216350219571, 118.1045761740670201, -0.5784513839558710346 ) ) ;
#10067 = CARTESIAN_POINT ( 'NONE',  ( -57.97566020452313040, 1.918554019021911916, -1.632400077439718933 ) ) ;
#10068 = VERTEX_POINT ( 'NONE', #10809 ) ;
#10069 = CARTESIAN_POINT ( 'NONE',  ( 4.525059116826507299, 118.1239383869072270, -0.4885259721435726288 ) ) ;
#10070 = CARTESIAN_POINT ( 'NONE',  ( 15.77383231466688152, 147.9505201145231865, -0.6473862450635482491 ) ) ;
#10071 = VERTEX_POINT ( 'NONE', #23791 ) ;
#10072 = CARTESIAN_POINT ( 'NONE',  ( -5.836546232834304959, 120.2771794157441008, -1.045480238269852480 ) ) ;
#10073 = CARTESIAN_POINT ( 'NONE',  ( 3.320832222217961593, -15.07605257934231702, 3.106094183260712516 ) ) ;
#10074 = CARTESIAN_POINT ( 'NONE',  ( 1.734723475976807094E-15, 17.14499999999999957, 0.000000000000000000 ) ) ;
#10075 = AXIS2_PLACEMENT_3D ( 'NONE', #3382, #16349, #25530 ) ;
#10076 = DIRECTION ( 'NONE',  ( -5.188838149069471174E-16, 1.699382548006136313E-16, 1.000000000000000000 ) ) ;
#10077 = CARTESIAN_POINT ( 'NONE',  ( 3.750385610654966229, 4.675867361267946443, -2.714424430587211834 ) ) ;
#10078 = CARTESIAN_POINT ( 'NONE',  ( 17.48541186233164879, 146.4615580561186050, 2.166240883089540770 ) ) ;
#10079 = CARTESIAN_POINT ( 'NONE',  ( -2.633907558715006481, 30.44407049250143871, 0.6696650445282713582 ) ) ;
#10080 = CARTESIAN_POINT ( 'NONE',  ( 3.740357457071568081, -9.854013591530623728, -7.545904704300070875 ) ) ;
#10081 = CARTESIAN_POINT ( 'NONE',  ( 12.96905644698476223, 133.8854804328748571, 0.4775921230882992918 ) ) ;
#10082 = CARTESIAN_POINT ( 'NONE',  ( -3.104076039314392244, 107.6120347158273631, 4.328431646495224605 ) ) ;
#10083 = CARTESIAN_POINT ( 'NONE',  ( -48.35712625370394591, 16.55775765112550602, -2.292466156223463614 ) ) ;
#10084 = DIRECTION ( 'NONE',  ( -0.8745520943968235761, 0.4849315768086558398, -4.268512490100410909E-16 ) ) ;
#10085 = CARTESIAN_POINT ( 'NONE',  ( 21.90559427349721489, 151.4293160993572371, 0.4377259060014726533 ) ) ;
#10086 = CARTESIAN_POINT ( 'NONE',  ( -48.28978369826177186, 19.63653578263565436, 5.206999999995388428 ) ) ;
#10087 = CARTESIAN_POINT ( 'NONE',  ( -7.772068811996249771, 69.25462295839062676, -1.523999999999995580 ) ) ;
#10088 = CARTESIAN_POINT ( 'NONE',  ( -58.32289719230551839, -0.2069853552843642364, -0.1059582036190383214 ) ) ;
#10089 = CARTESIAN_POINT ( 'NONE',  ( -6.059261036834497460, 88.73331249999998249, 5.016499999999999737 ) ) ;
#10090 = ADVANCED_FACE ( 'NONE', ( #14413 ), #35845, .T. ) ;
#10091 = CARTESIAN_POINT ( 'NONE',  ( -15.27962295839633811, 80.49293118800726177, -1.270000000000001350 ) ) ;
#10092 = CARTESIAN_POINT ( 'NONE',  ( -28.42835727709238114, 77.69497285144578314, -1.524000000000007793 ) ) ;
#10093 = CARTESIAN_POINT ( 'NONE',  ( -55.15137202863810728, 10.98262019425784430, 0.5441000652715827224 ) ) ;
#10094 = CARTESIAN_POINT ( 'NONE',  ( -55.65298819915649631, 5.540485941798511504, 2.823722248809245272 ) ) ;
#10095 = CARTESIAN_POINT ( 'NONE',  ( -20.66439279448300326, 152.5811724025633112, -0.09276230403812300851 ) ) ;
#10096 = ORIENTED_EDGE ( 'NONE', *, *, #23687, .F. ) ;
#10097 = CARTESIAN_POINT ( 'NONE',  ( -52.06588384925056801, 19.72955628943436679, -1.090601490622711080E-14 ) ) ;
#10098 = CARTESIAN_POINT ( 'NONE',  ( -6.054156888946658377, 121.4335526797924558, -0.1284449273526937774 ) ) ;
#10099 = AXIS2_PLACEMENT_3D ( 'NONE', #10299, #29475, #23059 ) ;
#10100 = ORIENTED_EDGE ( 'NONE', *, *, #23999, .F. ) ;
#10101 = CARTESIAN_POINT ( 'NONE',  ( -26.51793118801306548, 72.98537704160715123, -1.270000000000006013 ) ) ;
#10102 = CARTESIAN_POINT ( 'NONE',  ( -7.796516423212207059, 154.6345575486818404, -0.2631748570402914211 ) ) ;
#10103 = CARTESIAN_POINT ( 'NONE',  ( 3.833788745076180060, -15.06587152019073272, 5.274579322627055866 ) ) ;
#10104 = CIRCLE ( 'NONE', #615, 0.5080000000000002292 ) ;
#10105 = CARTESIAN_POINT ( 'NONE',  ( -14.84976704640063971, 123.2524255416106342, 1.171266444394656103 ) ) ;
#10106 = CARTESIAN_POINT ( 'NONE',  ( -4.631227783250409402, 22.10816835407601744, -0.05711764529929251599 ) ) ;
#10107 = CARTESIAN_POINT ( 'NONE',  ( 1.396185014843718264, 159.5914066142653098, 0.2870382629871537361 ) ) ;
#10108 = CARTESIAN_POINT ( 'NONE',  ( 1.982318871328906384, -15.65638878249517241, 5.868593396322577149 ) ) ;
#10109 = CARTESIAN_POINT ( 'NONE',  ( -17.14499999999999957, 71.11999999999999034, 1.904999999999989146 ) ) ;
#10110 = CARTESIAN_POINT ( 'NONE',  ( 0.4636875340052978300, -8.988401195314681402, -0.8615772474383697199 ) ) ;
#10111 = CARTESIAN_POINT ( 'NONE',  ( -23.42751387171889021, 146.8275480241000253, -0.6231101672962390259 ) ) ;
#10112 = CARTESIAN_POINT ( 'NONE',  ( -4.825036788391022569, 50.63946620154572997, -0.09641571798141751470 ) ) ;
#10113 = CYLINDRICAL_SURFACE ( 'NONE', #39757, 0.2539999999999997260 ) ;
#10114 = ORIENTED_EDGE ( 'NONE', *, *, #24172, .T. ) ;
#10115 = CARTESIAN_POINT ( 'NONE',  ( -8.793818945878454585, 117.7262650372997399, 0.04269669187023553830 ) ) ;
#10116 = ORIENTED_EDGE ( 'NONE', *, *, #32316, .F. ) ;
#10117 = CARTESIAN_POINT ( 'NONE',  ( -16.98580377952209020, 140.1729163700083518, 1.602912605581681804 ) ) ;
#10118 = DIRECTION ( 'NONE',  ( -0.6559537821943240976, 0.7548010569845284845, -4.686333752532409839E-16 ) ) ;
#10119 = CARTESIAN_POINT ( 'NONE',  ( 19.90801791207593396, 136.1824594150436383, 2.220825683169746156 ) ) ;
#10120 = CARTESIAN_POINT ( 'NONE',  ( 18.83801864273514326, 140.8526363637247982, -1.765582951612574281 ) ) ;
#10121 = CARTESIAN_POINT ( 'NONE',  ( -0.7398639285967090196, 8.776656789086558774, 0.6336005302938405581 ) ) ;
#10122 = CARTESIAN_POINT ( 'NONE',  ( -21.76696383529571577, 149.6930991844618291, -2.018179159957717683 ) ) ;
#10123 = CARTESIAN_POINT ( 'NONE',  ( 4.688774855980650358, 118.0063900739628338, -0.5874540965100417678 ) ) ;
#10124 = DIRECTION ( 'NONE',  ( -0.6294287539884068083, -0.7770581983690809658, -9.357678942267682069E-16 ) ) ;
#10125 = CARTESIAN_POINT ( 'NONE',  ( 10.51090385015211837, 123.6668265419868646, -0.9186085726806036966 ) ) ;
#10126 = CARTESIAN_POINT ( 'NONE',  ( -0.6438746309741667506, 120.9974662015465867, -0.01286614746332133928 ) ) ;
#10127 = VERTEX_POINT ( 'NONE', #4448 ) ;
#10128 = CARTESIAN_POINT ( 'NONE',  ( -7.475014592328212082, 120.3045338523282197, -1.338105361635808510 ) ) ;
#10129 = CARTESIAN_POINT ( 'NONE',  ( 2.047221892555406431, -15.65848914036231676, 5.808978358897256555 ) ) ;
#10130 = CARTESIAN_POINT ( 'NONE',  ( 3.009276887026297587, 50.13146620154573441, -1.210121013456480599 ) ) ;
#10131 = CARTESIAN_POINT ( 'NONE',  ( -47.02779878473986486, 24.11651466984139702, -2.637840241488492943 ) ) ;
#10132 = CARTESIAN_POINT ( 'NONE',  ( 7.823018779267000511, 156.2605297791399437, 2.010767698085225152 ) ) ;
#10133 = CARTESIAN_POINT ( 'NONE',  ( 2.958531772299235918, 50.13146620154573441, 1.329372033065076231 ) ) ;
#10134 = AXIS2_PLACEMENT_3D ( 'NONE', #4561, #5191, #4356 ) ;
#10135 = DIRECTION ( 'NONE',  ( 0.5149185422762211362, -0.8572391118119444542, 0.000000000000000000 ) ) ;
#10136 = CARTESIAN_POINT ( 'NONE',  ( -1.676539183893759777, 107.1743931308027129, 4.723177562573835253 ) ) ;
#10137 = B_SPLINE_CURVE_WITH_KNOTS ( 'NONE', 3,
 ( #7077, #10251, #16426, #23224, #15796, #2837, #29214, #36256, #19414, #13025, #41821, #19616 ),
 .UNSPECIFIED., .F., .F.,
 ( 4, 1, 1, 1, 1, 1, 1, 1, 1, 4 ),
 ( 0.7354344192538665448, 0.7685053377236187311, 0.8015760037631016743, 0.8346466698025848396, 0.8677173358420678939, 0.9007880018815508372, 0.9173233349012923643, 0.9338586679210338914, 0.9503940009407754186, 0.9543042185119922083 ),
 .UNSPECIFIED. ) ;
#10138 = CARTESIAN_POINT ( 'NONE',  ( -7.287282906664737325, 21.23368160547805061, -4.223004820119153457 ) ) ;
#10139 = CARTESIAN_POINT ( 'NONE',  ( 7.977778825752197100, 154.6030710842251494, 0.7700301581992888833 ) ) ;
#10140 = B_SPLINE_CURVE_WITH_KNOTS ( 'NONE', 3,
 ( #5072, #34240, #18023, #15252, #28039, #41048 ),
 .UNSPECIFIED., .F., .F.,
 ( 4, 2, 4 ),
 ( -0.0001503376881350242306, 0.0002168025613753844804, 0.0005839428108857932457 ),
 .UNSPECIFIED. ) ;
#10141 = CARTESIAN_POINT ( 'NONE',  ( 1.008409768533820250, 116.9791385580615781, -0.3449706568517265648 ) ) ;
#10142 = DIRECTION ( 'NONE',  ( 0.000000000000000000, 0.000000000000000000, 1.000000000000000000 ) ) ;
#10143 = CARTESIAN_POINT ( 'NONE',  ( 4.581726285797169673, -15.30239759124965460, -0.5121114015708873035 ) ) ;
#10144 = CARTESIAN_POINT ( 'NONE',  ( -16.17587344042707542, 121.2571949256804089, -0.3060957306870975003 ) ) ;
#10145 = ORIENTED_EDGE ( 'NONE', *, *, #9005, .T. ) ;
#10146 = CARTESIAN_POINT ( 'NONE',  ( -5.059956948048136560, 120.1989321871395049, -0.8615610664638462257 ) ) ;
#10147 = CARTESIAN_POINT ( 'NONE',  ( 3.433723587035138802, -15.33122114496111088, 5.473735664463222683 ) ) ;
#10148 = CARTESIAN_POINT ( 'NONE',  ( -2.970866406646269109, 156.0959049650892041, -0.4589190987796909482 ) ) ;
#10149 = CARTESIAN_POINT ( 'NONE',  ( 1.930977371672661924, -15.05712096081325591, 5.742647184725750087 ) ) ;
#10150 = CARTESIAN_POINT ( 'NONE',  ( -7.538779372106369614, 158.4854300789945398, 0.9926846707982196483 ) ) ;
#10151 = CARTESIAN_POINT ( 'NONE',  ( 6.898502017095807126, 117.1694300671557727, 0.1814136226821931042 ) ) ;
#10152 = ORIENTED_EDGE ( 'NONE', *, *, #3924, .T. ) ;
#10153 = CARTESIAN_POINT ( 'NONE',  ( 4.560362914109654220, -11.68884639558073069, 0.6953251057713033534 ) ) ;
#10154 = CARTESIAN_POINT ( 'NONE',  ( -16.31694223957266843, 121.4173703750124531, -0.3260513381110076714 ) ) ;
#10155 = CARTESIAN_POINT ( 'NONE',  ( 16.87828382557106721, 17.14499999999999957, 0.000000000000000000 ) ) ;
#10156 = CARTESIAN_POINT ( 'NONE',  ( 0.1691645607388194417, 105.7854827236532600, 5.338396616797809635 ) ) ;
#10157 = CARTESIAN_POINT ( 'NONE',  ( 6.991010015000402866, 121.8564574889588528, 0.4677317843132159925 ) ) ;
#10158 = AXIS2_PLACEMENT_3D ( 'NONE', #23127, #36164, #38930 ) ;
#10159 = CARTESIAN_POINT ( 'NONE',  ( 3.750385610654966229, 4.675867361267946443, -2.714424430587211834 ) ) ;
#10160 = CARTESIAN_POINT ( 'NONE',  ( 12.60858107845348997, 120.1953580586475567, 1.309872962259287954 ) ) ;
#10162 = CIRCLE ( 'NONE', #39429, 0.6350000000000014522 ) ;
#10161 = CARTESIAN_POINT ( 'NONE',  ( -0.1036566276974058148, 106.2435128697216413, 5.187401519901555957 ) ) ;
#10164 = CARTESIAN_POINT ( 'NONE',  ( 16.12297089460568955, 125.3625853296581312, -1.240993850804037013 ) ) ;
#10163 = CARTESIAN_POINT ( 'NONE',  ( -28.36525985791271154, 77.02308833105713859, 1.269999999999992468 ) ) ;
#10165 = CARTESIAN_POINT ( 'NONE',  ( -1.246715508051662535, 10.49814879194060069, 4.449005273994115939 ) ) ;
#10166 = CARTESIAN_POINT ( 'NONE',  ( -22.59100494123605074, 149.3758529064199934, -1.630758705999802105 ) ) ;
#10167 = ORIENTED_EDGE ( 'NONE', *, *, #19630, .T. ) ;
#10168 = CARTESIAN_POINT ( 'NONE',  ( -11.82813386268903955, 130.3161362890850512, -0.2363542639706542603 ) ) ;
#10169 = ORIENTED_EDGE ( 'NONE', *, *, #33432, .T. ) ;
#10170 = CARTESIAN_POINT ( 'NONE',  ( -5.918555687551815048, 121.5031286879076902, 0.05579296748036354642 ) ) ;
#10171 = CARTESIAN_POINT ( 'NONE',  ( 5.414172367154487908, -13.81390647261572546, 3.268633212004894872 ) ) ;
#10172 = CARTESIAN_POINT ( 'NONE',  ( -41.62422838180557960, 22.52195256220192832, 1.324149224697090954 ) ) ;
#10173 = CARTESIAN_POINT ( 'NONE',  ( -2.987330068958255147, 108.3452252202424404, -4.269296957098151601 ) ) ;
#10174 = ORIENTED_EDGE ( 'NONE', *, *, #1083, .F. ) ;
#10175 = CARTESIAN_POINT ( 'NONE',  ( 1.027076152783741536, 158.1148137021529578, 1.645667644272182706 ) ) ;
#10176 = CARTESIAN_POINT ( 'NONE',  ( 5.177913976931215245, 56.99702125087947024, 5.372099999999998765 ) ) ;
#10177 = CARTESIAN_POINT ( 'NONE',  ( 8.770618086120967050, 123.6813396614493712, 0.1752578222716852652 ) ) ;
#10178 = CARTESIAN_POINT ( 'NONE',  ( -16.42246607841806849, 155.2191194103077407, 0.6571739840263307597 ) ) ;
#10179 = CARTESIAN_POINT ( 'NONE',  ( 4.543739712435177047, -15.19060223592207137, -0.8445694877862246486 ) ) ;
#10180 = CIRCLE ( 'NONE', #34016, 0.6350000000000001199 ) ;
#10181 = CARTESIAN_POINT ( 'NONE',  ( 13.44960824739621863, 119.6710471929552000, -0.1296808650140443553 ) ) ;
#10182 = CIRCLE ( 'NONE', #28566, 0.5080000000000002292 ) ;
#10183 = CARTESIAN_POINT ( 'NONE',  ( -5.860279866612252420, 56.51500000000000057, -5.019549989587524408 ) ) ;
#10184 = CARTESIAN_POINT ( 'NONE',  ( -49.73866923540565210, 16.61554395881175594, 4.889435247958469510 ) ) ;
#10185 = CARTESIAN_POINT ( 'NONE',  ( -50.57586884603683330, 21.47051451305503988, 0.7809936997224511401 ) ) ;
#10186 = FACE_OUTER_BOUND ( 'NONE', #25932, .T. ) ;
#10187 = CARTESIAN_POINT ( 'NONE',  ( -54.32300027520380326, 9.724537220608771904, 3.743864951777626349 ) ) ;
#10188 = CARTESIAN_POINT ( 'NONE',  ( -58.78603281983694018, -0.2970393704508183519, 0.1722180483736777401 ) ) ;
#10189 = EDGE_CURVE ( 'NONE', #33842, #24193, #18312, .T. ) ;
#10190 = CARTESIAN_POINT ( 'NONE',  ( -4.412045077147967120, 118.1805591891959040, 0.3959213965498911691 ) ) ;
#10191 = CARTESIAN_POINT ( 'NONE',  ( -5.506767014370270275, 78.91949168437545836, -5.113098386149694363 ) ) ;
#10192 = VERTEX_POINT ( 'NONE', #27420 ) ;
#10193 = CARTESIAN_POINT ( 'NONE',  ( -4.336649912933128626, 118.7629491485454309, -1.056103682561591484 ) ) ;
#10194 = CARTESIAN_POINT ( 'NONE',  ( 8.331606247052166125, 120.0850720456318896, -1.118075670235503249 ) ) ;
#10195 = CARTESIAN_POINT ( 'NONE',  ( -5.210105874137158644, 116.2501875120488393, -1.173469071234783501 ) ) ;
#10196 = CARTESIAN_POINT ( 'NONE',  ( 4.433919446672925702, 118.1245909124861129, 0.7354544754953129537 ) ) ;
#10197 = CARTESIAN_POINT ( 'NONE',  ( -9.931348751161777955, 124.0638329749226330, -0.9965119107524912367 ) ) ;
#10198 = DIRECTION ( 'NONE',  ( 0.9891443546370349837, 0.000000000000000000, 0.1469470846586742874 ) ) ;
#10199 = CARTESIAN_POINT ( 'NONE',  ( 0.8479371882405327687, 117.9496053012138077, -1.365999150512961835 ) ) ;
#10200 = CARTESIAN_POINT ( 'NONE',  ( 5.615711437771513381, 117.9270669303711117, -0.5242027053071313114 ) ) ;
#10201 = CARTESIAN_POINT ( 'NONE',  ( -16.66101725429952651, 148.5304741467402323, -2.032660103712368382 ) ) ;
#10202 = EDGE_CURVE ( 'NONE', #26194, #19060, #33900, .T. ) ;
#10203 = CARTESIAN_POINT ( 'NONE',  ( 0.09347673290359038989, 104.6144662015457385, -6.110098594576430564 ) ) ;
#10204 = CARTESIAN_POINT ( 'NONE',  ( -0.004910621514806326471, 156.3161161488371533, 0.2457475809811482670 ) ) ;
#10205 = CARTESIAN_POINT ( 'NONE',  ( 8.262035544818608912, 120.4240392771561119, -1.115000201712876171 ) ) ;
#10206 = CARTESIAN_POINT ( 'NONE',  ( -14.15045567233496016, 138.8477291504528353, -0.2164309031519826565 ) ) ;
#10207 = CARTESIAN_POINT ( 'NONE',  ( -4.187759052228169132, -5.978784877027076838, 2.003160513425938483 ) ) ;
#10208 = CARTESIAN_POINT ( 'NONE',  ( 22.44855437653365726, 150.5824416163731314, 1.170575646458954289 ) ) ;
#10209 = DIRECTION ( 'NONE',  ( -5.188838149069471174E-16, 1.699382548006136313E-16, 1.000000000000000000 ) ) ;
#10210 = CARTESIAN_POINT ( 'NONE',  ( 2.913544029416218262, -15.22775915604775143, 4.213357497968500454 ) ) ;
#10211 = CARTESIAN_POINT ( 'NONE',  ( -7.566762702257322282, 120.1328256275108828, 1.061688055624673943 ) ) ;
#10212 = CARTESIAN_POINT ( 'NONE',  ( 0.7196250225040555781, 4.026961778641204859, -0.6563066166970625837 ) ) ;
#10213 = CARTESIAN_POINT ( 'NONE',  ( -6.903056240602074567, 117.3320596397172721, -0.5256612950045381760 ) ) ;
#10214 = CARTESIAN_POINT ( 'NONE',  ( -0.9385480264228447389, -6.289884363042010484, -0.2871545319985167044 ) ) ;
#10215 = ORIENTED_EDGE ( 'NONE', *, *, #3283, .F. ) ;
#10216 = PRODUCT_DEFINITION ( 'UNKNOWN', '', #37986, #7381 ) ;
#10217 = CARTESIAN_POINT ( 'NONE',  ( -47.20049172920048619, 19.11349993950443249, 3.907078929042784310 ) ) ;
#10218 = CARTESIAN_POINT ( 'NONE',  ( 6.073876170729577417, 119.5347744825833871, 0.5156133147040066200 ) ) ;
#10219 = DIRECTION ( 'NONE',  ( 1.000000000000000000, 0.000000000000000000, 0.000000000000000000 ) ) ;
#10220 = CARTESIAN_POINT ( 'NONE',  ( -16.04013775433294242, 147.3640369757652877, 0.6457813799431219026 ) ) ;
#10221 = ADVANCED_FACE ( 'NONE', ( #14001 ), #24268, .T. ) ;
#10222 = CARTESIAN_POINT ( 'NONE',  ( 2.228616319073483787, -14.90713850702725374, 5.562102343610016320 ) ) ;
#10223 = CARTESIAN_POINT ( 'NONE',  ( 17.47151851664378341, 144.3974720067888313, -1.548345126349529366 ) ) ;
#10224 = CARTESIAN_POINT ( 'NONE',  ( -16.71878049915338948, 131.5287050380659082, -2.312093064668929721 ) ) ;
#10225 = DIRECTION ( 'NONE',  ( 0.7308269722843274696, -0.6825627711659368879, 8.537024980200725183E-16 ) ) ;
#10226 = CARTESIAN_POINT ( 'NONE',  ( 2.351750233177451133, -15.05367847713771923, 4.985144330900271648 ) ) ;
#10227 = CARTESIAN_POINT ( 'NONE',  ( 0.01691503824229025066, 39.20946620154573026, -0.8464976821738524615 ) ) ;
#10228 = EDGE_CURVE ( 'NONE', #21511, #10570, #20379, .T. ) ;
#10229 = CARTESIAN_POINT ( 'NONE',  ( 2.805605324221167596, 120.9854572005495044, -0.04483369291007272689 ) ) ;
#10230 = EDGE_LOOP ( 'NONE', ( #24208, #38414, #30695, #18629 ) ) ;
#10231 = CARTESIAN_POINT ( 'NONE',  ( -9.960492004070040650, 64.81807050032566053, -1.523999999999996025 ) ) ;
#10232 = ADVANCED_FACE ( 'NONE', ( #4235 ), #16984, .F. ) ;
#10233 = DIRECTION ( 'NONE',  ( -0.000000000000000000, -0.000000000000000000, -1.000000000000000000 ) ) ;
#10234 = EDGE_CURVE ( 'NONE', #20064, #8022, #17196, .T. ) ;
#10235 = AXIS2_PLACEMENT_3D ( 'NONE', #13151, #3368, #6554 ) ;
#10236 = CARTESIAN_POINT ( 'NONE',  ( -5.008552712180506461, 117.3993836135855560, 0.7755994290793736257 ) ) ;
#10237 = CARTESIAN_POINT ( 'NONE',  ( 0.001640166039733662951, 159.6041700698465036, -0.08208061555506486473 ) ) ;
#10238 = CARTESIAN_POINT ( 'NONE',  ( -5.416379098809520620, 117.1811293437636721, 0.6832607176795201243 ) ) ;
#10239 = CARTESIAN_POINT ( 'NONE',  ( -0.7907830483637354746, 118.1473448952717860, 0.8952419762006665893 ) ) ;
#10240 = DIRECTION ( 'NONE',  ( -9.627370216492862708E-17, -1.000000000000000000, 0.000000000000000000 ) ) ;
#10241 = CARTESIAN_POINT ( 'NONE',  ( -4.654180141762545908, 32.06930816699426146, 0.6251022194440085666 ) ) ;
#10242 = CARTESIAN_POINT ( 'NONE',  ( 10.35908644403297352, 120.1444133044471556, 1.518303869478637491 ) ) ;
#10243 = CARTESIAN_POINT ( 'NONE',  ( -4.621022795674669226, 27.76579825817536218, 0.1735962381356405959 ) ) ;
#10244 = CARTESIAN_POINT ( 'NONE',  ( 8.391066749008803782, -15.30525627429770097, -0.4359234444501501327 ) ) ;
#10245 = CARTESIAN_POINT ( 'NONE',  ( 8.631715985724209617, 118.5888693174204889, -0.7825621615820586019 ) ) ;
#10246 = CARTESIAN_POINT ( 'NONE',  ( -3.291481622402053109, 124.4927030837263118, -0.08807361928342474777 ) ) ;
#10247 = CARTESIAN_POINT ( 'NONE',  ( 4.970385380909975837, 117.4009584165977600, 0.9889290504008942939 ) ) ;
#10248 = CARTESIAN_POINT ( 'NONE',  ( -10.28897677580358128, 57.14999999999998437, -5.016499999999999737 ) ) ;
#10249 = CARTESIAN_POINT ( 'NONE',  ( 0.8026539263819157943, 105.1230347856897538, 5.284155675286346110 ) ) ;
#10250 = CARTESIAN_POINT ( 'NONE',  ( -0.6244342276652131707, 19.93415720681881353, -4.586363120317934694 ) ) ;
#10251 = CARTESIAN_POINT ( 'NONE',  ( -48.08949201794742123, 19.91830422262442468, -5.194343260851647770 ) ) ;
#10252 = CARTESIAN_POINT ( 'NONE',  ( -16.18905205736058051, 121.2598130428683447, -0.3234957879086920451 ) ) ;
#10253 = CARTESIAN_POINT ( 'NONE',  ( 3.154677723130417277, -14.38507846778283650, 3.622984934187011952 ) ) ;
#10254 = CARTESIAN_POINT ( 'NONE',  ( 2.311559032573872408, 118.7862729053988318, -0.6846880608948527902 ) ) ;
#10255 = CARTESIAN_POINT ( 'NONE',  ( -22.69192130277354025, 142.3612397021088611, 0.6360799666370220429 ) ) ;
#10256 = DIRECTION ( 'NONE',  ( 0.1715592850456333085, -0.1224830539174543292, 0.9775302108976914317 ) ) ;
#10257 = ORIENTED_EDGE ( 'NONE', *, *, #102, .F. ) ;
#10258 = DIRECTION ( 'NONE',  ( 0.3256999990547876367, 0.9454731675810326141, 8.328397965208553695E-18 ) ) ;
#10259 = VERTEX_POINT ( 'NONE', #1250 ) ;
#10260 = CARTESIAN_POINT ( 'NONE',  ( 2.711364258112227255, 37.31625399494021877, -1.095520810760639119 ) ) ;
#10261 = CARTESIAN_POINT ( 'NONE',  ( 2.573200380748495331, -15.70867456196409151, 5.149826986703908815 ) ) ;
#10262 = CARTESIAN_POINT ( 'NONE',  ( -18.89434961005724034, 135.8679125664981484, 1.636908753694952257 ) ) ;
#10263 = VECTOR ( 'NONE', #39835, 1000.000000000000227 ) ;
#10264 = CARTESIAN_POINT ( 'NONE',  ( 21.87558878470073154, 148.2155681941778482, -1.275940291167070306 ) ) ;
#10265 = CARTESIAN_POINT ( 'NONE',  ( -4.476207883417873568, -7.053342675672244155, -1.178223045331058705 ) ) ;
#10266 = CARTESIAN_POINT ( 'NONE',  ( -58.81729092949609594, -0.2729283875645143742, -0.09353142974602446369 ) ) ;
#10267 = EDGE_CURVE ( 'NONE', #33175, #38422, #27212, .T. ) ;
#10268 = ORIENTED_EDGE ( 'NONE', *, *, #8709, .F. ) ;
#10269 = CARTESIAN_POINT ( 'NONE',  ( -4.958175139285456723, 117.4049635120808972, -1.028653955280601773 ) ) ;
#10270 = CARTESIAN_POINT ( 'NONE',  ( 0.3093948633799631920, 109.1907409294041429, 4.022046774707581207 ) ) ;
#10271 = PRODUCT_DEFINITION_SHAPE ( 'NONE', 'NONE',  #24009 ) ;
#10272 = CARTESIAN_POINT ( 'NONE',  ( -7.013665818177523548, 155.6889469082406947, 1.337060831506289293 ) ) ;
#10273 = CARTESIAN_POINT ( 'NONE',  ( -5.486567272856878414E-14, 86.35999999999998522, 0.000000000000000000 ) ) ;
#10274 = EDGE_CURVE ( 'NONE', #17215, #30025, #11021, .T. ) ;
#10275 = CARTESIAN_POINT ( 'NONE',  ( 15.45240368193225322, 131.3329289045130679, -1.560586129702050462 ) ) ;
#10276 = CIRCLE ( 'NONE', #3489, 3.175000000000001155 ) ;
#10277 = CARTESIAN_POINT ( 'NONE',  ( -20.39340916383850200, 150.0074677946399504, -2.333577254436574044 ) ) ;
#10278 = CARTESIAN_POINT ( 'NONE',  ( -57.50953982388014651, 1.662011999372992044, -1.631050346940590812 ) ) ;
#10279 = EDGE_LOOP ( 'NONE', ( #25889, #32003, #13465, #38023 ) ) ;
#10280 = CARTESIAN_POINT ( 'NONE',  ( 4.533610671541467241, 118.1203594940373307, -0.4772282360780506494 ) ) ;
#10281 = CARTESIAN_POINT ( 'NONE',  ( 15.99817776903315547, 146.0164801329953548, -0.4101439804456897265 ) ) ;
#10282 = ORIENTED_EDGE ( 'NONE', *, *, #25832, .T. ) ;
#10283 = CARTESIAN_POINT ( 'NONE',  ( -3.657622835216545631, 156.7231754051992425, -1.598616135119148129 ) ) ;
#10284 = CARTESIAN_POINT ( 'NONE',  ( 2.778183380295619287, -15.08691762314898277, 4.378844564414270835 ) ) ;
#10285 = ADVANCED_FACE ( 'NONE', ( #11225, #4026 ), #4654, .F. ) ;
#10286 = CARTESIAN_POINT ( 'NONE',  ( -2.444554238799683255, 105.1244307588895879, -4.750552072186019714 ) ) ;
#10287 = ADVANCED_FACE ( 'NONE', ( #1454 ), #40840, .T. ) ;
#10288 = CARTESIAN_POINT ( 'NONE',  ( -58.10259267898809554, 0.2821446311938036189, 0.7168088428568702986 ) ) ;
#10289 = CARTESIAN_POINT ( 'NONE',  ( -3.833338661037195561, 9.423677021345861604, 2.587938769098377279 ) ) ;
#10290 = CARTESIAN_POINT ( 'NONE',  ( -0.02615319344480391064, 156.8698190429800832, 1.308812744920978544 ) ) ;
#10291 = CARTESIAN_POINT ( 'NONE',  ( 1.215845237882275276, 34.83336793224903261, 0.05010825926065069075 ) ) ;
#10292 = EDGE_CURVE ( 'NONE', #514, #32447, #26316, .T. ) ;
#10293 = CIRCLE ( 'NONE', #13702, 3.683000000000001162 ) ;
#10294 = CARTESIAN_POINT ( 'NONE',  ( 4.256838582791900194, 16.71066835407712858, 1.825063967593055558 ) ) ;
#10295 = CARTESIAN_POINT ( 'NONE',  ( 2.816370844845887955, 121.0122979933374978, 0.1218616300372573624 ) ) ;
#10296 = CARTESIAN_POINT ( 'NONE',  ( -19.97113776634630611, 79.44829951959813741, 1.269999999999995799 ) ) ;
#10297 = CARTESIAN_POINT ( 'NONE',  ( -50.67046617086457161, 13.01238886216411039, -1.492009926703888656 ) ) ;
#10298 = CARTESIAN_POINT ( 'NONE',  ( 2.184308556171625781, 116.2030918562186912, -0.04283386123071435125 ) ) ;
#10299 = CARTESIAN_POINT ( 'NONE',  ( -36.65473259702432074, 28.27472347546385834, 1.269999999999995577 ) ) ;
#10300 = VECTOR ( 'NONE', #13334, 1000.000000000000000 ) ;
#10301 = DIRECTION ( 'NONE',  ( 5.188838149069472160E-16, -1.699382548006136559E-16, -1.000000000000000000 ) ) ;
#10302 = DIRECTION ( 'NONE',  ( -4.017660918040594346E-17, 1.000000000000000000, 2.376309959284834438E-19 ) ) ;
#10303 = DIRECTION ( 'NONE',  ( -0.8745520943968235761, 0.4849315768086558398, -4.268512490100410909E-16 ) ) ;
#10304 = CARTESIAN_POINT ( 'NONE',  ( -5.475330206976889436, 77.01756250000002524, 5.107412922131463695 ) ) ;
#10305 = CARTESIAN_POINT ( 'NONE',  ( -5.813441077435913762, 56.51499999999999346, 4.384678760708306200 ) ) ;
#10306 = LINE ( 'NONE', #10092, #1506 ) ;
#10307 = CARTESIAN_POINT ( 'NONE',  ( -58.00234944525002589, 2.059104932340308114, 0.8980956459801138214 ) ) ;
#10308 = CARTESIAN_POINT ( 'NONE',  ( -58.24807683554808335, 1.288543178753334573, 1.357556113208942428 ) ) ;
#10309 = CARTESIAN_POINT ( 'NONE',  ( -11.57591774076052893, 118.7825156662901378, 0.1473217720007393150 ) ) ;
#10310 = VERTEX_POINT ( 'NONE', #29984 ) ;
#10311 = CARTESIAN_POINT ( 'NONE',  ( -57.76461416131697746, 2.594137363129217277, -1.330350326707380626 ) ) ;
#10312 = CARTESIAN_POINT ( 'NONE',  ( -6.041016396376916120, 121.4368974476174543, -0.1415500717406000253 ) ) ;
#10313 = EDGE_LOOP ( 'NONE', ( #24145, #3318, #36897, #11171, #18412 ) ) ;
#10314 = CYLINDRICAL_SURFACE ( 'NONE', #5642, 12.69999999999999751 ) ;
#10315 = CARTESIAN_POINT ( 'NONE',  ( -15.52555164710823021, 147.5317938866932366, -0.3613967763117280629 ) ) ;
#10316 = CARTESIAN_POINT ( 'NONE',  ( 3.397480601066255712, -15.04020002808364964, 5.521695076403254632 ) ) ;
#10317 = AXIS2_PLACEMENT_3D ( 'NONE', #3674, #9834, #3462 ) ;
#10318 = CARTESIAN_POINT ( 'NONE',  ( -19.75353020121338332, 136.1149058410947532, 1.478659091479563203 ) ) ;
#10319 = CARTESIAN_POINT ( 'NONE',  ( 3.874746376330849618, 18.20996518813934628, -2.522041008920607563 ) ) ;
#10320 = CARTESIAN_POINT ( 'NONE',  ( 9.724873038621939969, 118.0756159837034716, 0.5523889259422302134 ) ) ;
#10321 = CARTESIAN_POINT ( 'NONE',  ( 1.965399808016191852, -15.70638203882245065, 5.774101002626401247 ) ) ;
#10322 = CARTESIAN_POINT ( 'NONE',  ( -31.84560491834792373, 53.04492649710044816, 1.269999999999993578 ) ) ;
#10323 = CARTESIAN_POINT ( 'NONE',  ( 0.07244829501375356362, -8.348772924205562163, -0.9745465824848156267 ) ) ;
#10324 = CARTESIAN_POINT ( 'NONE',  ( -23.20201897184738371, 149.6253602407241488, -0.6175280007103174373 ) ) ;
#10325 = CARTESIAN_POINT ( 'NONE',  ( 5.871452009091314039, 57.14999999999999858, -5.016499999999999737 ) ) ;
#10326 = CARTESIAN_POINT ( 'NONE',  ( 4.825036788390895559, 50.63946620154572997, 0.09641571798141809757 ) ) ;
#10327 = CARTESIAN_POINT ( 'NONE',  ( -5.554537448396219546, 116.8461671677355156, 0.2570831589019035301 ) ) ;
#10328 = ORIENTED_EDGE ( 'NONE', *, *, #30573, .F. ) ;
#10329 = CARTESIAN_POINT ( 'NONE',  ( -9.634306097686000214, 155.2307989660268959, 1.622952429610069469 ) ) ;
#10330 = CARTESIAN_POINT ( 'NONE',  ( -57.60360693722056169, 1.361403835229456849, -1.300536957989121500 ) ) ;
#10331 = CARTESIAN_POINT ( 'NONE',  ( 20.82642717637620677, 141.6159226613069109, 2.307662509007912810 ) ) ;
#10332 = CARTESIAN_POINT ( 'NONE',  ( 19.68629672748963344, 145.2539617268756729, -1.742627101631719855 ) ) ;
#10333 = CARTESIAN_POINT ( 'NONE',  ( -0.9136164112762927836, -2.447138680932527066, -0.3421040304710446511 ) ) ;
#10334 = AXIS2_PLACEMENT_3D ( 'NONE', #20823, #645, #1059 ) ;
#10335 = CARTESIAN_POINT ( 'NONE',  ( -17.48314440517399504, 153.9260871938423065, -1.866247694559708403 ) ) ;
#10336 = CARTESIAN_POINT ( 'NONE',  ( 4.625020092980742348, 118.0596586542457374, -0.5389086530673455888 ) ) ;
#10337 = AXIS2_PLACEMENT_3D ( 'NONE', #24338, #37138, #30527 ) ;
#10338 = CARTESIAN_POINT ( 'NONE',  ( 5.314256358593297591, 104.6144662015456959, -0.4585142902082095517 ) ) ;
#10339 = CARTESIAN_POINT ( 'NONE',  ( 11.07452758269540105, 153.1537610418535849, -0.9542791616922484677 ) ) ;
#10340 = CARTESIAN_POINT ( 'NONE',  ( -11.85733017202539230, 130.3381101163291760, -0.1934038552275227363 ) ) ;
#10341 = ORIENTED_EDGE ( 'NONE', *, *, #9982, .F. ) ;
#10342 = CARTESIAN_POINT ( 'NONE',  ( -7.432183457866743836, 120.4750020944285609, -1.305203700904508546 ) ) ;
#10343 = CARTESIAN_POINT ( 'NONE',  ( 4.858843758304779215, -15.48047902945742749, 1.209346601706016378 ) ) ;
#10344 = CARTESIAN_POINT ( 'NONE',  ( -5.274544067074300457, 115.7029491485454002, 0.8135768287290441325 ) ) ;
#10345 = CARTESIAN_POINT ( 'NONE',  ( -4.547563907768285674, 118.0745712654054387, -0.7853206451047147763 ) ) ;
#10346 = EDGE_CURVE ( 'NONE', #23040, #24227, #38580, .T. ) ;
#10347 = CARTESIAN_POINT ( 'NONE',  ( -56.71132732703541990, 3.319205314284062958, -2.191228219141365230 ) ) ;
#10348 = DIRECTION ( 'NONE',  ( -0.8745520943968126959, 0.4849315768086755463, -5.691349986800565628E-16 ) ) ;
#10349 = CARTESIAN_POINT ( 'NONE',  ( 11.01240597710799030, 122.5598569164413334, 1.651065454484659023 ) ) ;
#10350 = CARTESIAN_POINT ( 'NONE',  ( -30.01829664378881901, 60.43850663962886216, -1.270000000000005569 ) ) ;
#10351 = CARTESIAN_POINT ( 'NONE',  ( 22.76738278397251136, 137.3906169244638136, 0.4549464913834383450 ) ) ;
#10352 = CARTESIAN_POINT ( 'NONE',  ( 0.8142577860443056537, 14.98675861574836077, 8.418590528086960845 ) ) ;
#10353 = CARTESIAN_POINT ( 'NONE',  ( 2.729962743038877981, 120.7841308545065431, 0.3244322735474265973 ) ) ;
#10354 = CARTESIAN_POINT ( 'NONE',  ( 6.900334503690523036, 117.6856483911789581, -0.5402308543058538248 ) ) ;
#10355 = CARTESIAN_POINT ( 'NONE',  ( -41.62422838180499696, 22.52195256220245057, -1.324149224696933747 ) ) ;
#10356 = ORIENTED_EDGE ( 'NONE', *, *, #21004, .T. ) ;
#10357 = CARTESIAN_POINT ( 'NONE',  ( 0.4613487476409313670, 118.7629491485454025, 1.278559828376704344 ) ) ;
#10358 = CIRCLE ( 'NONE', #20532, 13.46199999999999619 ) ;
#10359 = UNCERTAINTY_MEASURE_WITH_UNIT (LENGTH_MEASURE( 1.000000000000000082E-05 ), #40102, 'distance_accuracy_value', 'NONE');
#10360 = CARTESIAN_POINT ( 'NONE',  ( -16.86121613381897433, 155.2078297922403465, -0.3138802613840050437 ) ) ;
#10361 = VERTEX_POINT ( 'NONE', #27835 ) ;
#10362 = CARTESIAN_POINT ( 'NONE',  ( 8.047001766538286915, 121.4495122670571590, -0.8773712736992811401 ) ) ;
#10363 = CARTESIAN_POINT ( 'NONE',  ( -47.26619606798129070, 24.98193397792426751, -1.785901896324533222 ) ) ;
#10364 = CARTESIAN_POINT ( 'NONE',  ( -9.304959842724306540, 124.0984330410602183, -0.5077435198050487264 ) ) ;
#10365 = CARTESIAN_POINT ( 'NONE',  ( 3.969679720280225421, -13.58737529183706627, 3.751183842293267290 ) ) ;
#10366 = CARTESIAN_POINT ( 'NONE',  ( -18.64118049546060263, 128.6297099747515347, 0.9949054493987050662 ) ) ;
#10367 = DIRECTION ( 'NONE',  ( -6.353134868986659519E-16, 1.000000000000000000, 0.000000000000000000 ) ) ;
#10368 = CARTESIAN_POINT ( 'NONE',  ( 5.748481425938850364, 159.1178304044242964, 0.1659167284945115006 ) ) ;
#10369 = ORIENTED_EDGE ( 'NONE', *, *, #19041, .T. ) ;
#10370 = CARTESIAN_POINT ( 'NONE',  ( 1.360477052538118681, -3.804838552850991817, 4.419457122809256511 ) ) ;
#10371 = CARTESIAN_POINT ( 'NONE',  ( -17.31377588638430964, 122.7721875394316555, -0.3459704467065360944 ) ) ;
#10372 = PLANE ( 'NONE',  #1769 ) ;
#10373 = AXIS2_PLACEMENT_3D ( 'NONE', #6018, #8993, #25588 ) ;
#10374 = CARTESIAN_POINT ( 'NONE',  ( 4.652282364505444967, 111.7580701808239070, 2.677127711625311157 ) ) ;
#10375 = CARTESIAN_POINT ( 'NONE',  ( 4.647043587409348753, 118.8389947276285881, 1.076879562718962235 ) ) ;
#10376 =( BOUNDED_CURVE ( )  B_SPLINE_CURVE ( 3, ( #9932, #16097, #29745, #29103, #10143, #35724, #42122 ),
 .UNSPECIFIED., .F., .T. ) 
 B_SPLINE_CURVE_WITH_KNOTS ( ( 4, 3, 4 ),
 ( 0.7498838476046071344, 1.000185576741208449, 1.000187438830518083 ),
 .UNSPECIFIED. ) 
 CURVE ( )  GEOMETRIC_REPRESENTATION_ITEM ( )  RATIONAL_B_SPLINE_CURVE ( ( 0.5000007283237750677, 0.4995979372591234369, 0.6662643611511984698, 1.000000000000000000, 0.9999975172142537838, 0.9999950344377539491, 0.9999925516705003847 ) ) 
 REPRESENTATION_ITEM ( '' )  );
#10377 = CARTESIAN_POINT ( 'NONE',  ( -1.319288878716189828, -8.717950886928733212, 4.428293336331323715 ) ) ;
#10378 = CARTESIAN_POINT ( 'NONE',  ( 14.37796933089559381, 121.0470547900126519, 1.299527359048518793 ) ) ;
#10379 = CARTESIAN_POINT ( 'NONE',  ( -57.02215525307828159, 2.672977372696112575, -2.026151568886790599 ) ) ;
#10381 = CARTESIAN_POINT ( 'NONE',  ( 11.80709641148037470, 120.8928578745602209, -1.148978701482599840 ) ) ;
#10380 = DIRECTION ( 'NONE',  ( -0.8745520943968243532, 0.4849315768086547296, -5.361993529360573944E-16 ) ) ;
#10382 = CARTESIAN_POINT ( 'NONE',  ( -1.959332070151295291, -8.942847522256865744, 4.198131957625402144 ) ) ;
#10383 = CARTESIAN_POINT ( 'NONE',  ( -22.83601474261773134, 146.5373477140321938, -1.546791039490589270 ) ) ;
#10384 = ORIENTED_EDGE ( 'NONE', *, *, #21447, .T. ) ;
#10385 = CARTESIAN_POINT ( 'NONE',  ( -7.938918103923473524, 154.5997988942315260, 0.3378123388718582421 ) ) ;
#10386 = CARTESIAN_POINT ( 'NONE',  ( 4.377062889037126148, -14.98224217357194199, 4.840108967533193862 ) ) ;
#10387 = DIRECTION ( 'NONE',  ( 0.01997839162482749689, 1.040247600000945640E-18, -0.9998004120163610509 ) ) ;
#10388 = VECTOR ( 'NONE', #36781, 1000.000000000000114 ) ;
#10389 = CARTESIAN_POINT ( 'NONE',  ( -1.300523255896344654, 106.1067062490390640, -5.175614940688300081 ) ) ;
#10390 = ORIENTED_EDGE ( 'NONE', *, *, #6379, .T. ) ;
#10391 = CARTESIAN_POINT ( 'NONE',  ( 12.62197313556516320, 122.7135068550949200, 1.834144044656287109 ) ) ;
#10392 = DIRECTION ( 'NONE',  ( -0.1469470846586743706, -9.335746474409589170E-17, -0.9891443546370348727 ) ) ;
#10393 = LINE ( 'NONE', #37221, #6906 ) ;
#10394 = CIRCLE ( 'NONE', #40373, 0.5080000000000000071 ) ;
#10395 = CARTESIAN_POINT ( 'NONE',  ( -15.27126642897852982, 121.5932973536894934, 0.6323128539531664982 ) ) ;
#10396 = CARTESIAN_POINT ( 'NONE',  ( -6.300109353874518980, 26.68925120273002705, -5.586516568188822696 ) ) ;
#10397 = CARTESIAN_POINT ( 'NONE',  ( 1.752245784495049863, 156.4219299504922844, 0.9069267871912084500 ) ) ;
#10398 = AXIS2_PLACEMENT_3D ( 'NONE', #4869, #32613, #4242 ) ;
#10399 = CARTESIAN_POINT ( 'NONE',  ( 2.843964318557650639, 116.7549172960530939, -0.2381273168889445624 ) ) ;
#10400 = CARTESIAN_POINT ( 'NONE',  ( -46.77033296427473630, 25.82163574504403059, 1.429790282917978939 ) ) ;
#10401 = CARTESIAN_POINT ( 'NONE',  ( -48.75318004186330967, 22.89261100037833785, 1.301163434177643241 ) ) ;
#10402 = DIRECTION ( 'NONE',  ( -0.1715592850456333363, 0.1224830539174543431, 0.9775302108976914317 ) ) ;
#10403 = CARTESIAN_POINT ( 'NONE',  ( -54.34142964503966056, 9.837102586603037935, 3.694930414371496052 ) ) ;
#10404 = CARTESIAN_POINT ( 'NONE',  ( -58.63886446992002988, -0.3042812601921741078, 0.3526691660533222694 ) ) ;
#10405 = CARTESIAN_POINT ( 'NONE',  ( -4.466856387348673962, 118.1267949675633417, 0.5517216040399967047 ) ) ;
#10406 = CARTESIAN_POINT ( 'NONE',  ( -5.586884702347497011, 110.9644662015457328, -0.1116392523995361624 ) ) ;
#10407 = ORIENTED_EDGE ( 'NONE', *, *, #3748, .T. ) ;
#10408 = CARTESIAN_POINT ( 'NONE',  ( -44.36446822842629700, 21.81554158013422651, 2.896954608336737014 ) ) ;
#10409 = CARTESIAN_POINT ( 'NONE',  ( -8.285659017902016643, 120.0588997814717089, -1.449894828885264664 ) ) ;
#10410 = CARTESIAN_POINT ( 'NONE',  ( -4.351830713015083951, 111.2795884869231173, -3.127581853150075197 ) ) ;
#10411 = VECTOR ( 'NONE', #38924, 1000.000000000000000 ) ;
#10412 = CARTESIAN_POINT ( 'NONE',  ( 4.522265204868332944, 118.1110255742863586, 0.6889464356651477939 ) ) ;
#10413 = CARTESIAN_POINT ( 'NONE',  ( -10.75107117262888501, 153.0872561326487187, -1.097343645257591538 ) ) ;
#10414 = AXIS2_PLACEMENT_3D ( 'NONE', #32006, #37982, #12207 ) ;
#10415 = CARTESIAN_POINT ( 'NONE',  ( -0.8958938016497142165, 115.7029491485453150, -1.751256854871092949 ) ) ;
#10416 = CARTESIAN_POINT ( 'NONE',  ( -5.924740142096584172, 65.21691166894066782, 1.270000000000006013 ) ) ;
#10417 = CARTESIAN_POINT ( 'NONE',  ( 0.1058213901577000071, 105.9761915687834772, -5.295735085524063024 ) ) ;
#10418 = CARTESIAN_POINT ( 'NONE',  ( -10.31823449898719147, 154.1877054190025262, -1.778048316349531088 ) ) ;
#10419 = CARTESIAN_POINT ( 'NONE',  ( -5.332935397695335311, 104.6144662015457385, -0.1065647409268299373 ) ) ;
#10420 = CARTESIAN_POINT ( 'NONE',  ( -0.009748065369249884343, 159.5507987164374981, 0.4878330526048098581 ) ) ;
#10421 = CARTESIAN_POINT ( 'NONE',  ( 8.413874481325049004, 119.6811429777993681, -1.089663159344693488 ) ) ;
#10422 = CARTESIAN_POINT ( 'NONE',  ( -11.83435633982874435, 152.0434770505088977, -0.1115628666874381447 ) ) ;
#10423 = EDGE_CURVE ( 'NONE', #915, #10519, #6577, .T. ) ;
#10424 = CARTESIAN_POINT ( 'NONE',  ( -3.178183004559932190, -7.902942162671289239, -3.366045245292264010 ) ) ;
#10425 = CARTESIAN_POINT ( 'NONE',  ( 14.80341400616306657, 120.8492938200443092, 1.052940121379140725 ) ) ;
#10426 = CARTESIAN_POINT ( 'NONE',  ( -14.60888863026623952, 79.54114996201613508, 1.269999999999998019 ) ) ;
#10427 = CARTESIAN_POINT ( 'NONE',  ( 3.154745640343158630, -14.88448557395780014, 3.454683184413806174 ) ) ;
#10428 = CARTESIAN_POINT ( 'NONE',  ( -18.37903003504447952, 149.1773161885088825, 1.724610598947830420 ) ) ;
#10429 = CARTESIAN_POINT ( 'NONE',  ( -0.5179912613141952615, -13.03896268189918217, -0.8249499322734266116 ) ) ;
#10430 = CARTESIAN_POINT ( 'NONE',  ( -14.49621620279169676, 120.3567457872619997, -0.7930654045677064667 ) ) ;
#10431 = VECTOR ( 'NONE', #635, 1000.000000000000000 ) ;
#10432 = CARTESIAN_POINT ( 'NONE',  ( -0.6011478996571989475, -4.452122406214784611, 0.7678286701737500053 ) ) ;
#10433 = ORIENTED_EDGE ( 'NONE', *, *, #36513, .F. ) ;
#10434 = CARTESIAN_POINT ( 'NONE',  ( -47.44699234454015624, 15.94620872345377904, 0.4021177788561363098 ) ) ;
#10435 = CARTESIAN_POINT ( 'NONE',  ( 3.094730188726686482, 108.9521120498200730, 4.030551393973051510 ) ) ;
#10436 = CARTESIAN_POINT ( 'NONE',  ( -1.703787162446291914, 156.3322054215483092, 0.5946588160098703613 ) ) ;
#10437 = CARTESIAN_POINT ( 'NONE',  ( 2.381342306750187099, -14.83133394530772264, 5.477793184119461145 ) ) ;
#10438 = CARTESIAN_POINT ( 'NONE',  ( 11.67916898317097818, 124.4569610989641859, -1.132436424213030035 ) ) ;
#10439 = CARTESIAN_POINT ( 'NONE',  ( -18.97962326299262159, 149.2349160008635351, -2.496544457321505650 ) ) ;
#10440 = DIRECTION ( 'NONE',  ( -1.000000000000000000, 1.365923996832131856E-16, 0.000000000000000000 ) ) ;
#10441 = EDGE_CURVE ( 'NONE', #1883, #11997, #34036, .T. ) ;
#10442 = CARTESIAN_POINT ( 'NONE',  ( 1.860714312465608478, -15.17550571231866741, 5.451645902226371021 ) ) ;
#10443 = DIRECTION ( 'NONE',  ( 0.8745520943968243532, -0.4849315768086547296, 6.829619984160642269E-16 ) ) ;
#10444 = CARTESIAN_POINT ( 'NONE',  ( 7.051595240896772587, 122.0586610246435129, 0.007850877590933884320 ) ) ;
#10445 = ORIENTED_EDGE ( 'NONE', *, *, #18832, .F. ) ;
#10446 = CARTESIAN_POINT ( 'NONE',  ( -3.764831887694549462, 109.1680670511255897, 3.784283605914390503 ) ) ;
#10447 = CARTESIAN_POINT ( 'NONE',  ( 3.527324519276021420, 50.63946620154572997, -1.707870599815379586 ) ) ;
#10448 = AXIS2_PLACEMENT_3D ( 'NONE', #28013, #2480, #28230 ) ;
#10449 = CARTESIAN_POINT ( 'NONE',  ( -3.745035802202505265E-14, 57.78499999999999659, -1.904999999999999805 ) ) ;
#10450 = AXIS2_PLACEMENT_3D ( 'NONE', #23996, #40222, #33612 ) ;
#10451 = CARTESIAN_POINT ( 'NONE',  ( 8.070121050663628282, 158.6666700270975525, 0.1062422583151904215 ) ) ;
#10452 = CARTESIAN_POINT ( 'NONE',  ( -6.342742252400029201, 120.0627515544778134, 0.2010047130458860465 ) ) ;
#10453 = AXIS2_PLACEMENT_3D ( 'NONE', #5964, #34932, #18923 ) ;
#10454 = CARTESIAN_POINT ( 'NONE',  ( 1.726544654667829137, -15.62332984182715556, 5.743678577341975178 ) ) ;
#10455 = CARTESIAN_POINT ( 'NONE',  ( -5.314278422745059238, 105.1224610256965235, 0.4583187270701644667 ) ) ;
#10456 = CARTESIAN_POINT ( 'NONE',  ( 0.9570772947141352738, 38.77965003586765391, -1.217401628196721042 ) ) ;
#10457 = CARTESIAN_POINT ( 'NONE',  ( 20.64857576366712522, 148.2641884961211076, 2.442776014760721814 ) ) ;
#10458 = CARTESIAN_POINT ( 'NONE',  ( 3.287934792154566299, 21.71798121574904172, 3.254339964430349230 ) ) ;
#10459 = CARTESIAN_POINT ( 'NONE',  ( -5.330747076954383878, 11.08732641057851964, -6.519097198751918398 ) ) ;
#10460 = CARTESIAN_POINT ( 'NONE',  ( 2.459102646145539417, 117.4060512218794230, -0.6259389031298756567 ) ) ;
#10461 = CARTESIAN_POINT ( 'NONE',  ( -0.3557171951619191863, 107.2171362991012842, -4.792661424475801901 ) ) ;
#10462 = AXIS2_PLACEMENT_3D ( 'NONE', #35346, #38960, #6793 ) ;
#10463 = CARTESIAN_POINT ( 'NONE',  ( -5.800481910058950419, 78.89561208401060810, 5.028344476440693711 ) ) ;
#10464 = DIRECTION ( 'NONE',  ( 4.017660918040594346E-17, -1.000000000000000000, -2.376309959284834438E-19 ) ) ;
#10465 = CARTESIAN_POINT ( 'NONE',  ( -0.001862839608620314551, 124.0591982226671490, 0.09322411149287226917 ) ) ;
#10466 = CARTESIAN_POINT ( 'NONE',  ( -1.932895124392534303, 20.38400505531995321, -4.219463811995566083 ) ) ;
#10467 = CYLINDRICAL_SURFACE ( 'NONE', #40107, 0.6350000000000014522 ) ;
#10468 = DIRECTION ( 'NONE',  ( -5.188838149069471174E-16, 1.699382548006136313E-16, 1.000000000000000000 ) ) ;
#10469 = CARTESIAN_POINT ( 'NONE',  ( 3.254806331274714637, -13.89383896039994504, 2.504907480430248246 ) ) ;
#10470 = EDGE_CURVE ( 'NONE', #35682, #18326, #37847, .T. ) ;
#10471 = CARTESIAN_POINT ( 'NONE',  ( 3.106711772599447308, 110.6400929099055332, -3.287732168264224430 ) ) ;
#10472 = CARTESIAN_POINT ( 'NONE',  ( -20.34281169216131246, 152.5255278361454145, 0.5339126128458231424 ) ) ;
#10473 = CARTESIAN_POINT ( 'NONE',  ( 4.801216665950859941, 117.4032681888241143, -1.015537427444714202 ) ) ;
#10474 = DIRECTION ( 'NONE',  ( -0.8745520943968235761, 0.4849315768086558398, -5.691349986800547879E-16 ) ) ;
#10475 = ORIENTED_EDGE ( 'NONE', *, *, #5011, .F. ) ;
#10476 = DIRECTION ( 'NONE',  ( 0.9998501190848636533, 0.01731298258487296016, -2.441448296158449905E-15 ) ) ;
#10477 = CARTESIAN_POINT ( 'NONE',  ( 5.320894714828252603, -15.22957080661538320, -0.4730099507937148284 ) ) ;
#10478 = CARTESIAN_POINT ( 'NONE',  ( -8.970048054448252373, 157.0267672960688969, 1.675204009492540669 ) ) ;
#10479 = CARTESIAN_POINT ( 'NONE',  ( 12.31483450803178314, 120.4651188882986759, -0.9715887866197354672 ) ) ;
#10480 = CARTESIAN_POINT ( 'NONE',  ( 4.611808778022512989, -11.57686662695173929, 0.3579861242195471194 ) ) ;
#10481 = CARTESIAN_POINT ( 'NONE',  ( -58.64197075571546947, -0.3086314946795363223, -0.3446796491146816854 ) ) ;
#10482 = EDGE_LOOP ( 'NONE', ( #23465, #21341, #19368, #8292 ) ) ;
#10483 = DIRECTION ( 'NONE',  ( -0.4849315768086534528, -0.8745520943968249084, -1.030032898892974818E-16 ) ) ;
#10484 = CARTESIAN_POINT ( 'NONE',  ( 1.846946891755073983, 121.3688471916803451, 0.3635544463458706965 ) ) ;
#10485 = SURFACE_STYLE_FILL_AREA ( #30494 ) ;
#10486 = CARTESIAN_POINT ( 'NONE',  ( -11.50974670170856129, 153.2879862121713757, 1.252373795633383802 ) ) ;
#10487 = CARTESIAN_POINT ( 'NONE',  ( 2.684992056639614599, 118.0925652926021598, 0.9597114035846702196 ) ) ;
#10488 = CARTESIAN_POINT ( 'NONE',  ( 18.42722449710328902, 147.3262642721504960, -1.661950199828387875 ) ) ;
#10489 = CARTESIAN_POINT ( 'NONE',  ( -5.841774105247432125, 118.7305451321402501, -1.158284778981343521 ) ) ;
#10490 = LINE ( 'NONE', #20479, #16780 ) ;
#10491 = CIRCLE ( 'NONE', #41799, 0.5080000000000002292 ) ;
#10492 = ORIENTED_EDGE ( 'NONE', *, *, #37489, .T. ) ;
#10493 = CARTESIAN_POINT ( 'NONE',  ( 4.535015814824959079, 118.1196967487753113, -0.4753252364964687393 ) ) ;
#10494 = CARTESIAN_POINT ( 'NONE',  ( 12.39727431377423272, 130.6617397222824479, -0.4182072254281058998 ) ) ;
#10495 = ORIENTED_EDGE ( 'NONE', *, *, #356, .T. ) ;
#10496 = CARTESIAN_POINT ( 'NONE',  ( 3.406014632911877893, -14.97454077108105430, 2.395711393442250259 ) ) ;
#10497 = CARTESIAN_POINT ( 'NONE',  ( -14.42383115828894447, 69.61113539875873357, 1.524000000000000243 ) ) ;
#10498 = CARTESIAN_POINT ( 'NONE',  ( -48.98643424071138952, 17.83616253325477174, 5.099923142907145213 ) ) ;
#10499 = EDGE_CURVE ( 'NONE', #32297, #33608, #4656, .T. ) ;
#10500 = CARTESIAN_POINT ( 'NONE',  ( -0.5165578309945342284, 6.287656885725535716, -4.620190224396742984 ) ) ;
#10501 = CARTESIAN_POINT ( 'NONE',  ( 17.05487166051791448, 147.7912591418244403, 2.046378512860588028 ) ) ;
#10502 = CARTESIAN_POINT ( 'NONE',  ( -2.297029980818328987, 30.88344267599554271, 1.420920951733973814 ) ) ;
#10503 = AXIS2_PLACEMENT_3D ( 'NONE', #2983, #25340, #3186 ) ;
#10504 = CARTESIAN_POINT ( 'NONE',  ( 2.229080734463354307, 9.364070591990056869, -4.050418370856919914 ) ) ;
#10505 = CARTESIAN_POINT ( 'NONE',  ( 7.564868681920670745, 122.4257779438054285, 0.2276018551017724989 ) ) ;
#10506 = CARTESIAN_POINT ( 'NONE',  ( -0.1064799869812408512, 105.7853621660184444, 5.332934571178566507 ) ) ;
#10507 = EDGE_CURVE ( 'NONE', #30484, #15671, #12016, .T. ) ;
#10508 = CARTESIAN_POINT ( 'NONE',  ( -51.86985193027736329, 10.34936321858908492, -9.208787596046330052E-15 ) ) ;
#10509 = CARTESIAN_POINT ( 'NONE',  ( 8.791514164305905155, 117.7407919306599524, -0.07643277369106631081 ) ) ;
#10510 = CARTESIAN_POINT ( 'NONE',  ( -24.32950799593924884, 77.42192949967211746, -1.270000000000005569 ) ) ;
#10511 = CARTESIAN_POINT ( 'NONE',  ( -46.91105319604628932, 25.30766295409365441, -1.767504291099697866 ) ) ;
#10512 = DIRECTION ( 'NONE',  ( 5.188838149069472160E-16, -1.699382548006136559E-16, -1.000000000000000000 ) ) ;
#10513 = CARTESIAN_POINT ( 'NONE',  ( -29.37490963521362275, 66.57792725179282911, -1.524000000000867994 ) ) ;
#10514 = CARTESIAN_POINT ( 'NONE',  ( -6.059261036834474368, 53.58606250000000415, 5.016499999999999737 ) ) ;
#10515 = CARTESIAN_POINT ( 'NONE',  ( -46.87324200585490530, 25.14909121271579195, 1.861784591013474266 ) ) ;
#10516 = CARTESIAN_POINT ( 'NONE',  ( -58.03112897257378933, 1.932186039288422030, 1.137512825365907254 ) ) ;
#10517 = CARTESIAN_POINT ( 'NONE',  ( -55.60508136934060275, 7.116827924314645060, 3.170888472016278214 ) ) ;
#10518 = CARTESIAN_POINT ( 'NONE',  ( -18.55749356256747262, 125.2038358216989735, -0.01254332324266062976 ) ) ;
#10519 = VERTEX_POINT ( 'NONE', #28472 ) ;
#10520 = CARTESIAN_POINT ( 'NONE',  ( -56.91719228404756592, 5.442273006173628858, -0.3640331681397807606 ) ) ;
#10521 = CARTESIAN_POINT ( 'NONE',  ( -6.971431743821577598, 121.9475450123567839, -0.2149471541011502840 ) ) ;
#10522 = ADVANCED_FACE ( 'NONE', ( #11645 ), #22888, .T. ) ;
#10523 = ORIENTED_EDGE ( 'NONE', *, *, #41005, .T. ) ;
#10524 = PLANE ( 'NONE',  #15822 ) ;
#10525 = CARTESIAN_POINT ( 'NONE',  ( -2.887663853482277165, 156.0927491134738716, -0.09102753749515611614 ) ) ;
#10526 = CARTESIAN_POINT ( 'NONE',  ( 5.913917015499376539, -14.05268412609835060, 2.470677959447274308 ) ) ;
#10527 = CARTESIAN_POINT ( 'NONE',  ( -5.882407806703863429, 118.3130479344264501, 0.8400364453129069986 ) ) ;
#10528 = CARTESIAN_POINT ( 'NONE',  ( 4.537321141924904211, 26.63107350737006840, 0.8823464973398146283 ) ) ;
#10529 = CARTESIAN_POINT ( 'NONE',  ( 22.58226468115093866, 150.6256779753201158, 0.9011697351191821914 ) ) ;
#10530 = EDGE_CURVE ( 'NONE', #27874, #25310, #5926, .T. ) ;
#10531 = CARTESIAN_POINT ( 'NONE',  ( 15.71988674539023734, 146.8976217521451133, 0.5151081277902610500 ) ) ;
#10532 = CARTESIAN_POINT ( 'NONE',  ( 4.537321141924904211, 26.63107350737006840, 0.8823464973398146283 ) ) ;
#10533 = CARTESIAN_POINT ( 'NONE',  ( 0.3060232888392590556, -2.951246395405549450, 0.9280917289473271659 ) ) ;
#10534 = CARTESIAN_POINT ( 'NONE',  ( -22.51303867192119057, 150.7865899205276321, -0.6781733187083917036 ) ) ;
#10535 = CARTESIAN_POINT ( 'NONE',  ( 6.059261036834394432, 71.63300248836196715, 5.016499999999999737 ) ) ;
#10536 = CARTESIAN_POINT ( 'NONE',  ( 4.962522518486619738, 117.4026900519639440, 1.030022258927823398 ) ) ;
#10537 = ORIENTED_EDGE ( 'NONE', *, *, #40728, .F. ) ;
#10538 = CARTESIAN_POINT ( 'NONE',  ( -5.558216936808848097, 116.7820928991152556, 0.1694093166678532214 ) ) ;
#10539 = CARTESIAN_POINT ( 'NONE',  ( -1.377724515701776120, 119.5584937100158243, 0.5648184346096531971 ) ) ;
#10540 = CARTESIAN_POINT ( 'NONE',  ( -58.16081875750722219, 0.1563330388574495078, -0.6246648654044505422 ) ) ;
#10541 = CARTESIAN_POINT ( 'NONE',  ( 1.123502178401303064, 117.8708904510121016, 0.6147983682407556216 ) ) ;
#10542 = CARTESIAN_POINT ( 'NONE',  ( 11.87140890173645857, 122.0047285378078357, -1.287708742280476493 ) ) ;
#10543 = CARTESIAN_POINT ( 'NONE',  ( -0.3089908097382615959, -9.589635095254870123, 0.9269408180416041088 ) ) ;
#10544 = CARTESIAN_POINT ( 'NONE',  ( -4.901975893987194688, 117.8999350694477926, -0.9234475893805552671 ) ) ;
#10545 = CARTESIAN_POINT ( 'NONE',  ( 4.661932672826285540, 118.0285282382062206, -0.5802744411614334519 ) ) ;
#10546 = CARTESIAN_POINT ( 'NONE',  ( -48.82738941085167284, 18.57305038084609095, -5.399437279161923620 ) ) ;
#10547 = CARTESIAN_POINT ( 'NONE',  ( 5.344295804397718008, 104.6144662015764482, -0.1103522168260312741 ) ) ;
#10548 = CARTESIAN_POINT ( 'NONE',  ( 3.236331573563320241, 156.2293907256693331, -0.8668920366435199920 ) ) ;
#10549 = ADVANCED_FACE ( 'NONE', ( #24418 ), #492, .T. ) ;
#10550 = CARTESIAN_POINT ( 'NONE',  ( -15.76285804746354380, 145.9067145067653541, -0.3149794173055767699 ) ) ;
#10551 = ORIENTED_EDGE ( 'NONE', *, *, #9754, .T. ) ;
#10552 = CARTESIAN_POINT ( 'NONE',  ( -18.42282194684162278, 148.3462492009778373, -2.436111078577046118 ) ) ;
#10553 = CARTESIAN_POINT ( 'NONE',  ( 5.204094786718133747, -15.42339607600888485, 1.288180339967581967 ) ) ;
#10554 = CARTESIAN_POINT ( 'NONE',  ( -4.623307638546573450, 118.0214715435377997, -0.8250825005389410549 ) ) ;
#10555 = CARTESIAN_POINT ( 'NONE',  ( -49.72660956849071567, 16.83360665160238412, -5.072308565479707099 ) ) ;
#10556 = CARTESIAN_POINT ( 'NONE',  ( 4.146107882323581961, 118.2391775594914520, 0.3988131543976252691 ) ) ;
#10557 = CARTESIAN_POINT ( 'NONE',  ( 3.340139884075139509, 119.4525916976722897, 0.8552862985148332875 ) ) ;
#10558 = CARTESIAN_POINT ( 'NONE',  ( -5.095652749712312080, 31.83908346630384756, 0.3959475160674750249 ) ) ;
#10559 = CARTESIAN_POINT ( 'NONE',  ( 0.8865878252961926220, 116.4323782974132513, 0.004867729696705778465 ) ) ;
#10560 = CARTESIAN_POINT ( 'NONE',  ( -6.244303144875123834, 11.31477948022340208, -5.679040650537692692 ) ) ;
#10561 = CARTESIAN_POINT ( 'NONE',  ( 15.93611381433498941, 145.8030804522035737, 1.048911189365803853 ) ) ;
#10562 = EDGE_CURVE ( 'NONE', #12982, #1192, #39242, .T. ) ;
#10563 = CARTESIAN_POINT ( 'NONE',  ( 14.59306090326458261, 120.9595740141730289, -0.6228583445698288035 ) ) ;
#10564 = CARTESIAN_POINT ( 'NONE',  ( -7.772068811996249771, 69.25462295839062676, 1.524000000000003796 ) ) ;
#10565 = CARTESIAN_POINT ( 'NONE',  ( 4.401043740403896010, 115.6909491485452435, 1.538549278747252114 ) ) ;
#10566 = CARTESIAN_POINT ( 'NONE',  ( -22.66420477949326795, 150.6410255081855212, -0.3761569768119877311 ) ) ;
#10567 = AXIS2_PLACEMENT_3D ( 'NONE', #2997, #41971, #9372 ) ;
#10568 = ORIENTED_EDGE ( 'NONE', *, *, #15865, .F. ) ;
#10569 = CARTESIAN_POINT ( 'NONE',  ( -5.496727918792607248, 120.7378957778092570, -0.7277922162673816642 ) ) ;
#10570 = VERTEX_POINT ( 'NONE', #5281 ) ;
#10571 = DIRECTION ( 'NONE',  ( -5.206863593109713661E-17, 1.000000000000000000, -1.077750396879097183E-30 ) ) ;
#10572 = CARTESIAN_POINT ( 'NONE',  ( -1.571702145576721721, 120.8584627942791627, -0.1987642453017052502 ) ) ;
#10573 = CARTESIAN_POINT ( 'NONE',  ( 4.422138279315844578, -13.30579995099732926, 3.341551838899307736 ) ) ;
#10574 = CARTESIAN_POINT ( 'NONE',  ( -22.37379725164922561, 146.3189071340513294, 1.009121573351525525 ) ) ;
#10575 = DIRECTION ( 'NONE',  ( -0.9807655518882848478, 0.1951894777626808908, -8.537024980200819846E-16 ) ) ;
#10576 = CARTESIAN_POINT ( 'NONE',  ( 15.18737561846505102, 156.0999766016731769, 0.3708822620858234775 ) ) ;
#10577 = EDGE_CURVE ( 'NONE', #26127, #14331, #2621, .T. ) ;
#10578 = ORIENTED_EDGE ( 'NONE', *, *, #1891, .T. ) ;
#10579 = CARTESIAN_POINT ( 'NONE',  ( -1.251853189678833411, -4.679435864505671283, 4.458631606201990394 ) ) ;
#10580 = CARTESIAN_POINT ( 'NONE',  ( -18.63504953328976299, 154.1157618415863624, -0.3723726386282264489 ) ) ;
#10581 = CARTESIAN_POINT ( 'NONE',  ( -18.88948446928058900, 80.17638627449419175, 1.269999999999995799 ) ) ;
#10582 = FACE_OUTER_BOUND ( 'NONE', #7787, .T. ) ;
#10583 = CARTESIAN_POINT ( 'NONE',  ( -5.358236209449569465, 119.5150064772791012, 0.8961528214930735148 ) ) ;
#10584 = CARTESIAN_POINT ( 'NONE',  ( -1.290833045837797455, 0.8901568857254957834, 4.466177308409287505 ) ) ;
#10585 = CARTESIAN_POINT ( 'NONE',  ( 5.840790351889470600, 117.5931221156369730, 0.8184019802203833516 ) ) ;
#10586 = CARTESIAN_POINT ( 'NONE',  ( -58.76944392236582360, -0.3049061203676955989, -0.2000781065760083854 ) ) ;
#10588 = CARTESIAN_POINT ( 'NONE',  ( 13.62782584980143952, 121.9345505566020194, -1.161422094953211470 ) ) ;
#10587 = CARTESIAN_POINT ( 'NONE',  ( -5.861642722916909243, 64.54502714855203749, -1.269999999999993801 ) ) ;
#10589 = CARTESIAN_POINT ( 'NONE',  ( 4.471266627501615076, -5.469457446779734333, -1.220754042301255948 ) ) ;
#10590 = CARTESIAN_POINT ( 'NONE',  ( -22.48407052889642799, 149.9757045183965261, -1.524144198737067635 ) ) ;
#10591 = VERTEX_POINT ( 'NONE', #28258 ) ;
#10592 = CARTESIAN_POINT ( 'NONE',  ( -8.684730043605732419, 123.3259068333282755, 0.1300027459630656579 ) ) ;
#10593 = CARTESIAN_POINT ( 'NONE',  ( 6.473144302699227026, -13.19137087452153168, 0.2309683151692971392 ) ) ;
#10594 = DIRECTION ( 'NONE',  ( -5.188838149069471174E-16, 1.699382548006136313E-16, 1.000000000000000000 ) ) ;
#10595 = CARTESIAN_POINT ( 'NONE',  ( 1.734723475976807094E-15, 17.14499999999999957, 0.000000000000000000 ) ) ;
#10597 = ORIENTED_EDGE ( 'NONE', *, *, #6446, .T. ) ;
#10596 = AXIS2_PLACEMENT_3D ( 'NONE', #34273, #11670, #14648 ) ;
#10598 = CARTESIAN_POINT ( 'NONE',  ( 12.21694169560761800, 122.3148578561100948, 1.796258641216138541 ) ) ;
#10599 = DIRECTION ( 'NONE',  ( -5.188838149069471174E-16, 1.699382548006136313E-16, 1.000000000000000000 ) ) ;
#10600 = DIRECTION ( 'NONE',  ( 6.353134868986659519E-16, -1.000000000000000000, 0.000000000000000000 ) ) ;
#10601 = CARTESIAN_POINT ( 'NONE',  ( -5.484805557156832378, 159.0107326448372191, 0.7391455978106867830 ) ) ;
#10602 = CARTESIAN_POINT ( 'NONE',  ( 5.585279946883024316, 5.098922668322787288, -6.300588543511215001 ) ) ;
#10603 = CARTESIAN_POINT ( 'NONE',  ( -0.006077178772757848950, 120.4695998130595598, 0.3041268764237433087 ) ) ;
#10604 = DIRECTION ( 'NONE',  ( -0.9998004120163609398, 0.000000000000000000, -0.01997839162482749342 ) ) ;
#10605 = CARTESIAN_POINT ( 'NONE',  ( 0.9702981664978360676, 116.7682604261274264, -0.2585377725347692834 ) ) ;
#10606 = CARTESIAN_POINT ( 'NONE',  ( 4.646169936107913401, 117.9325745699973282, -0.7782960047779410306 ) ) ;
#10607 = CARTESIAN_POINT ( 'NONE',  ( -57.61251194202308312, 1.342215824410947222, 1.291938351770520077 ) ) ;
#10608 = CARTESIAN_POINT ( 'NONE',  ( -48.74997074597248314, 21.16799237019927205, 3.036721307642054946 ) ) ;
#10609 = CARTESIAN_POINT ( 'NONE',  ( 2.959734542844846938, 107.4070365762694479, -4.429236197848620549 ) ) ;
#10610 = CARTESIAN_POINT ( 'NONE',  ( -49.72660956849071567, 16.83360665160238412, 5.072308565479690223 ) ) ;
#10611 = CARTESIAN_POINT ( 'NONE',  ( -58.19146433326328349, 0.6478084378821518108, 1.146157376894137325 ) ) ;
#10612 = CARTESIAN_POINT ( 'NONE',  ( -4.439880037416177316, 118.1648146445724876, 0.4551947970507644325 ) ) ;
#10613 = CARTESIAN_POINT ( 'NONE',  ( 1.814579162714248461, 106.5840813593849248, -4.953779699249533763 ) ) ;
#10614 = B_SPLINE_SURFACE_WITH_KNOTS ( 'NONE', 3, 3, ( 
 ( #5716, #18672, #22276, #21434, #12084, #18884, #28691, #25072, #15685, #34670, #21646, #1881, #31679, #2729, #2307, #5500, #35301, #27848, #22072, #34462, #18244, #15267, #2091, #41278, #15055, #41064, #41491, #11875, #8682, #35099, #25286, #38077, #12297, #38290, #5922, #41700, #12508, #25498, #38498, #6129, #19303, #9934, #35938, #32308, #376, #3782, #23114 ),
 ( #19511, #22483, #41912, #22695, #35512, #29321, #3138, #32520, #16100, #16743, #6967, #3351, #16318, #29105, #29747, #6750, #165, #10144, #19938, #42123, #25702, #35726, #26549, #12919, #6333, #587, #38707, #2933, #25910, #32956, #38917, #19093, #19719, #9728, #6537, #13134, #13559, #26126, #10360, #36367, #36150, #39555, #15895, #23331, #39339, #32738, #9516 ),
 ( #32101, #39127, #22904, #3571, #28897, #16532, #29541, #13343, #12712, #26332, #33367, #30363, #30578, #39981, #40394, #4199, #7805, #16952, #20342, #1417, #17163, #20766, #4827, #4619, #11396, #33997, #14374, #40596, #26763, #30162, #13766, #13965, #17574, #10566, #1002, #27384, #7184, #20553, #7383, #10983, #11188, #26970, #10772, #36774, #17779, #14171, #23753 ),
 ( #7591, #24173, #33583, #33791, #29951, #4415, #37183, #17372, #8005, #30778, #20976, #24382, #1627, #14582, #20143, #39772, #1212, #23545, #27175, #27587, #36566, #40189, #33166, #3993, #23966, #36985, #791, #5240, #8628, #35052, #34833, #21806, #8843, #25020, #14793, #12460, #37388, #12245, #9058, #21178, #31839, #15636, #34206, #28434, #8206, #21591, #34620 ),
 ( #5447, #28641, #17991, #2256, #5034, #38241, #1829, #38022, #31196, #5667, #22023, #24589, #41652, #28220, #18407, #2039, #28003, #37803, #40804, #30988, #41012, #11605, #31414, #37596, #15218, #34406, #5872, #25238, #41226, #12029, #18195, #18835, #18624, #31629, #41440, #2679, #8422, #27796, #11820, #21381, #15004, #24809, #2469, #15431, #9268, #32264, #13294 ),
 ( #13080, #41866, #12870, #19463, #19885, #3094, #16690, #536, #328, #6915, #22226, #32900, #3520, #26071, #2884, #3732, #22853, #26280, #16481, #6702, #29486, #29695, #35892, #25454, #22432, #6487, #35255, #116, #16266, #38451, #19042, #32472, #39289, #23068, #6079, #36101, #10095, #32047, #15847, #29269, #28853, #12664, #25654, #19671, #38661, #39080, #9469 ),
 ( #35462, #9882, #6284, #19255, #32685, #16054, #38866, #29057, #42076, #25859, #9678, #22642, #35678, #3302, #20506, #39718, #36723, #36937, #4150, #4570, #10518, #14125, #23277, #26712, #7757, #23489, #27126, #11145, #10932, #17735, #40351, #20722, #4785, #33113, #36515, #20090, #20293, #23921, #16903, #7335, #33746, #13510, #29905, #33321, #17113, #30114, #26916 ),
 ( #40140, #17529, #1160, #3943, #30736, #26499, #30530, #27339, #39503, #7962, #33954, #10309, #1370, #36313, #39930, #10723, #954, #743, #23703, #7133, #13718, #33534, #13922, #14327, #7545, #24132, #4366, #37141, #20930, #17326, #30315, #34579, #40969, #8375, #34366, #1996, #4989, #24341, #5199, #17947, #11773, #1789, #14959, #40762, #41396, #31586, #27960 ),
 ( #27551, #34787, #21133, #34163, #24764, #14751, #37762, #30949, #27752, #18362, #11559, #24544, #21761, #37977, #37551, #21340, #11355, #18153, #40557, #5621, #25192, #8586, #21549, #31157, #5406, #31368, #2211, #24978, #28390, #18577, #5829, #15170, #37345, #8165, #38196, #28176, #41181, #11984, #8802, #2424, #15385, #12201, #9012, #21977, #35009, #18784, #1584 ),
 ( #14542, #10047, #28809, #12823, #15593, #6443, #22597, #23019, #25409, #25810, #19620, #29436, #13249, #275, #35841, #38411, #12417, #35629, #36048, #6656, #9222, #61, #16430, #3254, #26233, #42025, #3468, #38819, #22180, #6862, #16214, #39237, #35210, #6037, #22804, #13031, #18998, #35412, #32633, #31796, #2634, #28598, #12619, #41607, #32002, #2841, #15800 ),
 ( #41825, #19418, #38615, #26021, #29008, #39030, #25606, #22388, #9420, #6240, #9630, #32424, #19210, #32218, #3051, #9838, #29219, #16009, #13879, #7712, #20250, #14080, #13668, #696, #32848, #30068, #27083, #39667, #3680, #23874, #20460, #26873, #26449, #36894, #10677, #30271, #10472, #36261, #905, #4318, #29858, #7081, #23440, #40091, #4105, #20045, #33276 ),
 ( #33063, #39880, #16642, #3894, #7500, #16858, #23659, #10886, #36679, #20674, #33698, #33489, #19835, #23228, #26660, #36469, #7288, #17282, #17065, #1113, #29650, #488, #13461, #39452, #10255, #25734, #29137, #13381, #13170, #196, #29358, #3384, #35335, #32990, #15723, #32773, #29576, #41739, #10178, #36186, #12543, #6782, #28727, #42154, #12950, #19336, #22311 ),
 ( #38533, #22728, #25532, #16567, #6163, #16351, #9549, #26160, #412, #2968, #19974, #6573, #25942, #22520, #6366, #16133, #19132, #9348, #32342, #32136, #38950, #15932, #9763, #12747, #26368, #3603, #35758, #19542, #38741, #39376, #32550, #39162, #19751, #23147, #28928, #41946, #3171, #7005, #35550, #9968, #22940, #35969, #29784, #10601, #33829, #13801, #3817 ),
 ( #33407, #40018, #40436, #23581, #37223, #21015, #20803, #27423, #16986, #17408, #1456, #1253, #8042, #30614, #27214, #16781, #23367, #26799, #10395, #36603, #14208, #7217, #39808, #40229, #623, #20177, #29986, #7423, #20381, #17200, #14416, #11024, #30404, #24005, #33621, #36400, #13592, #26581, #4657, #17613, #39591, #11227, #24213, #33202, #37025, #4028, #30198 ),
 ( #826, #1038, #4238, #14003, #10811, #27009, #23793, #36814, #4450, #7633, #7840, #20591, #36374, #16539, #20562, #20776, #20351, #13349, #383, #40198, #26770, #16749, #29754, #16958, #29957, #10574, #33375, #23975, #3789, #33591, #36784, #39989, #7601, #33800, #26979, #36993, #13565, #39780, #26339, #4207, #7390, #7814, #10150, #23553, #4424, #14181, #10994 ),
 ( #23120, #39345, #17171, #29549, #17382, #36156, #10781, #1221, #30170, #27184, #36574, #30372, #1011, #6973, #19944, #13975, #32964, #593, #26555, #39561, #23761, #10366, #20149, #23337, #7191, #33172, #4000, #797, #13773, #18416, #38032, #8852, #18204, #27805, #14384, #34416, #11405, #15013, #40605, #27392, #28012, #15229, #20985, #37605, #1838, #24392, #37397 ),
 ( #14802, #4836, #17789, #5044, #17999, #40813, #21390, #12038, #34006, #8638, #24818, #41021, #37813, #21816, #11831, #25029, #1637, #11614, #30587, #5249, #8432, #4628, #40403, #24599, #34629, #2265, #28229, #41235, #21601, #11197, #24183, #31205, #17583, #5456, #37192, #31423, #1426, #2048, #8014, #30787, #14591, #27596, #8214, #21187, #34215, #30997, #28443 ),
 ( #3102, #41449, #38460, #25868, #9890, #9686, #39088, #15645, #22652, #6495, #26080, #34842, #6293, #15856, #2479, #22441, #41661, #16063, #32056, #29065, #31848, #25464, #16275, #9067, #12674, #25663, #9278, #35264, #18634, #42085, #2894, #25247, #35470, #5676, #28863, #19473, #22236, #6088, #31638, #38670, #32480, #19051, #41875, #15440, #12254, #38874, #38250 ),
 ( #5882, #9477, #22033, #35061, #19264, #18844, #2688, #12879, #35686, #28650, #12469, #32272, #3309, #29279, #124, #13088, #16913, #20098, #17334, #1169, #19679, #13931, #22863, #7141, #33122, #26507, #29495, #36323, #14133, #3530, #29913, #6711, #23713, #336, #23497, #16698, #32695, #4159, #33542, #39297, #13727, #3951, #29703, #13519, #23286, #26289, #16489 ),
 ( #752, #23076, #26720, #19894, #20514, #10731, #39728, #10527, #32909, #4374, #36524, #7343, #26926, #36731, #36110, #13302, #39512, #30325, #6924, #10105, #27135, #3740, #544, #10318, #7554, #20303, #35900, #33329, #17122, #30122, #962, #40148, #39939, #2220, #28183, #27969, #34585, #7766, #5414, #31164, #40770, #30540, #18369, #8383, #11781, #24348, #11153 ),
 ( #30743, #24140, #40565, #37769, #17955, #37148, #34170, #34373, #1592, #2005, #7970, #11568, #20730, #20938, #5206, #33963, #24553, #8593, #21347, #15179, #21557, #18161, #10941, #1378, #4792, #17538, #17743, #14967, #14336, #14549, #40978, #23930, #27346, #27558, #11363, #37355, #8173, #31376, #24771, #37558, #36945, #33754, #40358, #4580, #21141, #4997, #30956 ),
 ( #1796, #14759, #27759, #41614, #24986, #9426, #9229, #31594, #28816, #32430, #22187, #25817, #2641, #31804, #11991, #32008, #12829, #28604, #15601, #3261, #37985, #32226, #18586, #2431, #12424, #12210, #25416, #28398, #15392, #15808, #41403, #25199, #19216, #35419, #38204, #9021, #8810, #21984, #21768, #3058, #22604, #35217, #38417, #35017, #2848, #6043, #38825 ),
 ( #16015, #16221, #41831, #34795, #5628, #35636, #19005, #5837, #18791, #12625, #25613, #38623, #22396, #6450, #6247, #29014, #42034, #9636, #19424, #41188, #39675, #7507, #26239, #10262, #13038, #3902, #20052, #20466, #22811, #23235, #17072, #26879, #10684, #39887, #33283, #35849, #9844, #33071, #33495, #4112, #6663, #10478, #13886, #705, #23665, #39461, #912 ),
 ( #4325, #13676, #36685, #19626, #32641, #20256, #23447, #3474, #32856, #30075, #29227, #68, #26028, #10055, #39037, #16436, #29443, #282, #26667, #36270, #13255, #16865, #36056, #36475, #26457, #7295, #39246, #19842, #6869, #23026, #496, #3688, #16649, #29656, #13468, #29865, #7090, #34540, #17289, #34331, #31118, #1119, #11731, #37724, #14088, #8332, #30278 ),
 ( #20888, #23880, #30692, #8548, #40097, #24298, #27089, #18113, #36899, #17906, #11105, #10893, #40721, #27919, #33706, #8121, #14497, #24094, #7922, #17693, #20682, #7718, #33912, #4527, #27511, #17491, #1542, #14288, #14915, #5159, #40519, #11311, #27297, #40925, #34119, #37304, #21302, #1955, #30487, #1330, #4740, #24720, #40312, #37104, #21507, #21095, #4946 ),
 ( #30910, #1748, #14707, #27712, #11516, #24501, #37506, #15757, #32170, #18955, #3006, #15554, #19166, #28556, #28129, #25768, #31961, #15965, #41139, #11945, #38567, #28762, #24936, #8966, #9380, #22555, #22344, #9586, #28346, #35367, #28963, #38775, #5366, #2800, #41564, #15126, #35165, #12157, #41776, #2594, #12576, #2381, #38153, #41979, #21719, #25360, #38365 ),
 ( #31323, #25563, #12372, #37934, #5992, #18321, #9179, #12778, #21934, #6197, #2167, #8757, #34743, #5574, #18532, #31537, #15341, #41355, #25150, #34963, #5786, #18741, #31751, #22136, #39194, #19, #6816, #13834, #16168, #444, #19371, #36430, #12985, #36216, #29391, #3206, #16815, #4063, #9796, #26403, #32805, #231, #26190, #36004, #38986, #29173, #10002 ),
 ( #35795, #19786, #32586, #33235, #23399, #3636, #16601, #3419, #17023, #10211, #29609, #26615, #7249, #6607, #25978, #22974, #861, #19578, #22762, #30021, #16386, #32377, #13208, #20208, #13414, #35585, #23181, #39408, #7037, #20005, #26832, #33022, #39839, #10636, #10428, #6402, #3851, #29817, #13624, #656, #39622, #31066, #21049, #24454, #37057, #23829, #27459 ),
 ( #36848, #11057, #8282, #30649, #7667, #4691, #4901, #14241, #14657, #20625, #24249, #33444, #33655, #17856, #4480, #37257, #21252, #34075, #27870, #34282, #30857, #14867, #1069, #17440, #30230, #30437, #1702, #27041, #1283, #27661, #23615, #40050, #27248, #40263, #24042, #7875, #5111, #40672, #8075, #20838, #11464, #37458, #40879, #36636, #18063, #17647, #4271 ),
 ( #1904, #33862, #7458, #1492, #14449, #20416, #10843, #40472, #11263, #17234, #14037, #37675, #22091, #21880, #2114, #41512, #3541, #34906, #38517, #15289, #2329, #24666, #2543, #25517, #41301, #28294, #16502, #8498, #2751, #31271, #15077, #12105, #24885, #25094, #41088, #28077, #28504, #11896, #37882, #31914, #5945, #8705, #21668, #21455, #34692, #34485, #15707 ),
 ( #12319, #5522, #5317, #35118, #22297, #18479, #15504, #8914, #31484, #38099, #5738, #18691, #18268, #31701, #25306, #38310, #9130, #18904, #28711, #9334, #41721, #12526, #35322, #6722, #19690, #32707, #29509, #11679, #30333, #13531, #6936, #16924, #7776, #556, #16711, #40158, #19907, #26301, #7152, #1180, #10329, #348, #30134, #29714, #29924, #36535, #36955 ),
 ( #13940, #27146, #10539, #14143, #23508, #23088, #20739, #26938, #10950, #36122, #32922, #33554, #10743, #3753, #3963, #4386, #17548, #17344, #4589, #23938, #33764, #13315, #39949, #7354, #10117, #973, #20111, #23724, #39740, #36742, #39525, #33133, #39310, #26518, #20313, #33340, #762, #13738, #23299, #7564, #4170, #36336, #20524, #26732, #17132, #15189, #34179 ),
 ( #21355, #2228, #17964, #5005, #34803, #14344, #21565, #7978, #20946, #30964, #1600, #1805, #17750, #33971, #5215, #4799, #30750, #8602, #24780, #14557, #27564, #40367, #11370, #27354, #34593, #12001, #24562, #27768, #40573, #34381, #40779, #28192, #8181, #30549, #5422, #5637, #18169, #11162, #24147, #24994, #11576, #24357, #37361, #14766, #37566, #8393, #31172 ),
 ( #18377, #31386, #11789, #41198, #1388, #40986, #8818, #21149, #2013, #37156, #14976, #27977, #21777, #37778, #37994, #6459, #16229, #78, #29235, #22611, #12218, #41411, #22404, #39045, #35644, #38212, #29024, #3270, #32234, #13046, #28825, #32439, #41839, #25208, #9851, #3066, #26036, #9029, #21994, #9644, #42042, #35025, #22197, #19433, #35858, #22821, #18594 ),
 ( #5846, #12838, #31603, #16024, #2441, #12635, #15402, #25621, #18801, #28406, #25825, #31812, #2648, #15608, #28613, #38834, #41622, #35226, #12431, #25424, #38425, #9238, #6051, #19013, #32018, #2856, #15817, #38632, #9435, #35429, #6254, #19224, #17080, #3911, #918, #3697, #39469, #30284, #23034, #26675, #39683, #10272, #7098, #32649, #30080, #16873, #39256 ),
 ( #36065, #32865, #26464, #16657, #20059, #4330, #4120, #33290, #20263, #36483, #26247, #23888, #6671, #23670, #20474, #3486, #1126, #27094, #16445, #39894, #19634, #33080, #29873, #23243, #13263, #712, #40103, #29451, #13685, #290, #7513, #10063, #7304, #505, #6880, #13893, #17295, #19851, #10486, #23456, #13477, #36277, #26885, #29663, #10691, #36689, #33500 ),
 ( #14095, #10898, #34549, #24729, #37311, #8127, #33918, #5374, #11525, #4953, #27927, #37732, #7928, #1336, #11318, #2176, #37109, #11112, #18329, #14294, #20689, #1550, #8556, #4747, #36905, #24508, #24101, #24306, #30917, #15135, #33714, #40934, #7723, #21102, #34126, #40526, #27305, #17912, #28138, #17497, #1756, #4535, #21515, #40320, #37515, #30700, #30495 ),
 ( #20896, #27718, #14715, #14504, #27519, #40727, #17700, #8340, #21308, #34338, #5166, #18121, #31126, #1963, #31331, #41146, #14925, #11742, #11952, #22564, #41783, #35174, #15972, #12786, #38161, #31544, #41573, #32386, #25160, #41362, #35593, #2390, #8768, #31759, #25776, #34971, #24943, #12583, #12165, #12382, #18963, #19382, #2602, #16179, #29, #41988, #6410 ),
 ( #3015, #25572, #15349, #3217, #22351, #38784, #38373, #8975, #28773, #28970, #15561, #21942, #25369, #9594, #31970, #5794, #6001, #6205, #28564, #29182, #18751, #38576, #34751, #9187, #19176, #22143, #9388, #37943, #35376, #21728, #5584, #32182, #18541, #28354, #2807, #15768, #19795, #23407, #16394, #22985, #7256, #12993, #29400, #39204, #32815, #36012, #26413 ),
 ( #39631, #26622, #664, #32596, #30237, #25987, #30029, #26840, #38996, #7465, #3645, #9805, #3859, #39848, #453, #29618, #17243, #22773, #4071, #3429, #240, #13425, #26200, #39417, #13217, #10012, #29825, #6826, #16610, #33242, #20216, #10220, #23190, #35804, #36224, #6618, #17031, #36643, #7046, #20012, #33031, #16823, #13632, #10643, #10436, #19586, #869 ),
 ( #36438, #13842, #23624, #20425, #33452, #4280, #1291, #14456, #40271, #40885, #31072, #1500, #27468, #11066, #11687, #17863, #11272, #34289, #1912, #14248, #7675, #17654, #8504, #27256, #17447, #24673, #20634, #27050, #7883, #14874, #24050, #1077, #30863, #30446, #30655, #37263, #37682, #20845, #34492, #18276, #18071, #21462, #40057, #5323, #21259, #1709, #33663 ),
 ( #4488, #5118, #11471, #37065, #4700, #27876, #14046, #10850, #23837, #33870, #36858, #40478, #24255, #8082, #14664, #21055, #34081, #27668, #4908, #24460, #40679, #37465, #8289, #21886, #12735, #5528, #9137, #22096, #34914, #31708, #15083, #41727, #41519, #21675, #18910, #22510, #12325, #15921, #5745, #31921, #8713, #6358, #31277, #6153, #2957, #28084, #25725 ),
 ( #22302, #2120, #15510, #28511, #18697, #37888, #2549, #9539, #11902, #38318, #41095, #32126, #34699, #2756, #25102, #24891, #12532, #41936, #18485, #35124, #25313, #38105, #5950, #15713, #31491, #2336, #28716, #15295, #25521, #28301, #38522, #41307, #28919, #19119, #9338, #35326, #12112, #38732, #35538, #8921, #10385, #7208, #32542, #25933, #35960, #26789, #19535 ),
 ( #38942, #3163, #26150, #20168, #29347, #19328, #6995, #35749, #6774, #13372, #13791, #39153, #10592, #36594, #36392, #816, #16125, #39800, #39580, #19964, #9753, #23572, #16770, #33191, #32762, #3375, #23138, #23357, #9959, #16342, #19742, #4020, #26359, #188, #402, #612, #22930, #16977, #13161, #32982, #29128, #3595, #13584, #16558, #3807, #29976, #29775 ),
 ( #26572, #32333, #22721, #29568, #6564, #39366, #42148, #10170, #36176, #12942, #7411, #23783, #33609, #27205, #17399, #20794, #5066, #4856, #34030, #21006, #40628, #24621, #24411, #11636, #30394, #37418, #21209, #40834, #20373, #17812, #30606, #17190, #37215, #14198, #30809, #4647, #1658, #4441, #40218, #31018, #36805, #27413, #40424, #11015, #7831, #33396, #14613 ),
 ( #27617, #4229, #7623, #1243, #23994, #37013, #33819, #18020, #11425, #8237, #34235, #8034, #26999, #30188, #1030, #1861, #14823, #13994, #27826, #40009, #10801, #20582, #17603, #1446, #14405, #11219, #24203, #8871, #15876, #18224, #2498, #21412, #38478, #2069, #38270, #31442, #5274, #18864, #6108, #11853, #28463, #34863, #2285, #28249, #38052, #41043, #31225 ),
 ( #5694, #37835, #21834, #34648, #35283, #25483, #18654, #31659, #5476, #19072, #12276, #15462, #28670, #9297, #8662, #15034, #12061, #2915, #21622, #24840, #32078, #28034, #34439, #15248, #22259, #18436, #37629, #25266, #41254, #25048, #41468, #28883, #9086, #41895, #12693, #12488, #8454, #22052, #35081, #15664, #5902, #31868, #2708, #41681, #26529, #39109, #25888 ),
 ( #3331, #13324, #3121, #771, #25685, #566, #39534, #9497, #20120, #3973, #22461, #16721, #38690, #9914, #22884, #29302, #32292, #35922, #16934, #6313, #32719, #35492, #10340, #16081, #26312, #19492, #19286, #6949, #36347, #42106, #16512, #6732, #32503, #16300, #26104, #29086, #12900, #146, #38895, #19700, #9708, #3553, #22673, #23311, #13540, #29518, #358 ),
 ( #39320, #10126, #29724, #7161, #35708, #6517, #13112, #33145, #23098, #36131, #29933, #19917, #32932, #3762, #2184, #23734, #13748, #1396, #30145, #1191, #7786, #8775, #33564, #5592, #31552, #31339, #37951, #10550, #21735, #33977, #14352, #33350, #34758, #11170, #15142, #27154, #13950, #17556, #18335, #4397, #26948, #14151, #41152, #20747, #39960, #36965, #37163 ) ),
 .UNSPECIFIED., .F., .F., .F.,
 ( 4, 1, 1, 1, 1, 1, 1, 1, 1, 1, 1, 1, 1, 1, 1, 1, 1, 1, 1, 1, 1, 1, 1, 1, 1, 1, 1, 1, 1, 1, 1, 1, 1, 1, 1, 1, 1, 1, 1, 1, 1, 1, 1, 1, 1, 1, 4 ),
 ( 4, 1, 1, 1, 1, 1, 1, 1, 1, 1, 1, 1, 2, 1, 1, 1, 2, 1, 1, 1, 1, 1, 2, 1, 1, 1, 1, 1, 1, 1, 2, 1, 1, 1, 1, 1, 1, 1, 1, 1, 4 ),
 ( 0.000000000000000000, 0.007812500000000000000, 0.01562500000000000000, 0.02343750000000000000, 0.03125000000000000000, 0.04687500000000000000, 0.06250000000000000000, 0.07812500000000000000, 0.09375000000000000000, 0.1093750000000000000, 0.1250000000000000000, 0.1406250000000000000, 0.1562500000000000000, 0.1875000000000000000, 0.2187500000000000000, 0.2500000000000000000, 0.2812500000000000000, 0.3125000000000000000, 0.3281250000000000000, 0.3437500000000000000, 0.3750000000000000000, 0.4062500000000000000, 0.4375000000000000000, 0.4687500000000000000, 0.5000000000000000000, 0.5312500000000000000, 0.5625000000000000000, 0.5937500000000000000, 0.6250000000000000000, 0.6562500000000000000, 0.6718750000000000000, 0.6875000000000000000, 0.7187500000000000000, 0.7500000000000000000, 0.7812500000000000000, 0.8125000000000000000, 0.8437500000000000000, 0.8750000000000000000, 0.8906250000000000000, 0.9062500000000000000, 0.9218750000000000000, 0.9375000000000000000, 0.9531250000000000000, 0.9687500000000000000, 0.9765625000000000000, 0.9843750000000000000, 1.000000000000000000 ),
 ( 0.000000000000000000, 0.01539374999999999945, 0.03078749999999999890, 0.04618125000000002089, 0.06157499999999999779, 0.07696875000000003020, 0.09236250000000004179, 0.1077562499999999979, 0.1231499999999999956, 0.1431375000000000008, 0.1631250000000000200, 0.1831125000000000114, 0.2031000000000000028, 0.2063375000000000070, 0.2095750000000000113, 0.2128125000000000155, 0.2160500000000000198, 0.2667375000000000163, 0.3174250000000000682, 0.3681125000000000647, 0.4188000000000000611, 0.5201750000000000540, 0.6215500000000000469, 0.6266374999999999584, 0.6317250000000000920, 0.6368124999999997815, 0.6418999999999999151, 0.6469874999999999376, 0.6520749999999999602, 0.6571624999999999828, 0.6622500000000000053, 0.7044687500000000879, 0.7466875000000001705, 0.7889062500000000311, 0.8010555555555555207, 0.8311249999999998916, 0.8733437499999998632, 0.9155625000000000568, 0.9403166666666666895, 0.9577812500000000284, 1.000000000000000000 ),
 .UNSPECIFIED. ) ;
#10615 = ORIENTED_EDGE ( 'NONE', *, *, #32998, .F. ) ;
#10616 = CARTESIAN_POINT ( 'NONE',  ( -41.05189575270516400, 23.09451173561986081, 1.523999999999992472 ) ) ;
#10617 = CARTESIAN_POINT ( 'NONE',  ( 8.354336569859343697, 119.9739600045604675, -1.115347381135292970 ) ) ;
#10618 = CARTESIAN_POINT ( 'NONE',  ( -2.490049542275868166, 107.2224589468338536, -4.730309301830580182 ) ) ;
#10619 = CARTESIAN_POINT ( 'NONE',  ( 4.554505725324297316, 118.0858391265290805, 0.7375152256654264882 ) ) ;
#10620 = CARTESIAN_POINT ( 'NONE',  ( -16.25331603292288563, 145.9442052555630767, -1.443193537303810059 ) ) ;
#10621 = CARTESIAN_POINT ( 'NONE',  ( -1.187503523883304712, 115.7029482321909200, -1.742292230791464336 ) ) ;
#10622 = CARTESIAN_POINT ( 'NONE',  ( 0.7493318530476299477, 117.9496056092839069, -1.372937156641410361 ) ) ;
#10623 = AXIS2_PLACEMENT_3D ( 'NONE', #30431, #23175, #30224 ) ;
#10624 = DIRECTION ( 'NONE',  ( -0.9998004120163608288, 0.000000000000000000, -0.01997839162482749342 ) ) ;
#10625 = CARTESIAN_POINT ( 'NONE',  ( -10.02184412846599315, 123.2077283916686525, -1.294377628214502751 ) ) ;
#10626 = DIRECTION ( 'NONE',  ( -0.9336303900108815501, -0.3582377630124009560, -4.235673982319039874E-16 ) ) ;
#10627 = CARTESIAN_POINT ( 'NONE',  ( -47.20932677516402975, 20.06242161047454076, 5.120036295479145849 ) ) ;
#10628 = AXIS2_PLACEMENT_3D ( 'NONE', #37178, #41004, #11810 ) ;
#10629 = CARTESIAN_POINT ( 'NONE',  ( 8.325883379001766116, 120.1130057568717433, -1.118334525995474227 ) ) ;
#10630 = CARTESIAN_POINT ( 'NONE',  ( -8.882710456238886110, 123.9526509987454261, -0.04472055067538689005 ) ) ;
#10631 = CIRCLE ( 'NONE', #23537, 0.2539999999999998925 ) ;
#10632 = CARTESIAN_POINT ( 'NONE',  ( -17.14500000000466784, 71.11999999999886768, 1.269999999999998241 ) ) ;
#10633 = CARTESIAN_POINT ( 'NONE',  ( 22.70904429024572835, 149.7444054411783441, 1.421740456058896207 ) ) ;
#10634 = DIRECTION ( 'NONE',  ( -5.188838149069471174E-16, 1.699382548006136313E-16, 1.000000000000000000 ) ) ;
#10635 = CARTESIAN_POINT ( 'NONE',  ( 2.816406720412386822, -15.24816796146632925, 4.372395393210481984 ) ) ;
#10636 = CARTESIAN_POINT ( 'NONE',  ( -18.50101540898971919, 149.0103496150362901, 1.723905467370217437 ) ) ;
#10637 = CARTESIAN_POINT ( 'NONE',  ( -0.9160044981361634697, -1.370538221358817310, 0.3309596765904046500 ) ) ;
#10638 = CARTESIAN_POINT ( 'NONE',  ( -7.949750681159734711, 158.6775731370129279, -0.5882489250746234521 ) ) ;
#10639 = CARTESIAN_POINT ( 'NONE',  ( -0.9749442489646007459, 26.91501818708639249, 0.01812370653153724809 ) ) ;
#10640 = ORIENTED_EDGE ( 'NONE', *, *, #38131, .F. ) ;
#10641 = CARTESIAN_POINT ( 'NONE',  ( -53.75865956017525349, 9.373754164828760338, 3.697140908559925165 ) ) ;
#10642 = CARTESIAN_POINT ( 'NONE',  ( 5.744069310734388090, 120.3160329940760818, 0.4351690567359403072 ) ) ;
#10643 = CARTESIAN_POINT ( 'NONE',  ( -3.102522256439491422, 156.1450793681712241, 0.6153187215006974409 ) ) ;
#10644 = CARTESIAN_POINT ( 'NONE',  ( 3.520038346949750707, -14.46602075298747359, 5.128058278438484052 ) ) ;
#10645 = CARTESIAN_POINT ( 'NONE',  ( 17.77977776825574452, 147.3864036964934598, -1.530147356706996309 ) ) ;
#10646 = ORIENTED_EDGE ( 'NONE', *, *, #36018, .T. ) ;
#10647 = CARTESIAN_POINT ( 'NONE',  ( -19.28990034181461510, 145.1342744731992127, -2.527759927608660195 ) ) ;
#10648 = CARTESIAN_POINT ( 'NONE',  ( 4.835342064185105926, 104.6144662015457527, -0.09903605035092130637 ) ) ;
#10649 = CARTESIAN_POINT ( 'NONE',  ( 2.995043271588619493, -14.66878921821561299, 4.005342282345994320 ) ) ;
#10650 = CARTESIAN_POINT ( 'NONE',  ( -4.874430425846600023, 117.4785343618161875, -1.135543576852563463 ) ) ;
#10651 = CARTESIAN_POINT ( 'NONE',  ( 9.140193528981123805, 153.9061766533773152, -0.01708403265280362612 ) ) ;
#10652 = VERTEX_POINT ( 'NONE', #28042 ) ;
#10653 = CARTESIAN_POINT ( 'NONE',  ( -5.219734918942418034, 114.8006916078311690, 1.211930405771829866 ) ) ;
#10654 = CARTESIAN_POINT ( 'NONE',  ( 4.549352062591466073, 112.0094687158549789, 2.856336935586818448 ) ) ;
#10655 = PLANE ( 'NONE',  #32041 ) ;
#10656 = CARTESIAN_POINT ( 'NONE',  ( -4.974001918040873882, 117.3966124607983659, -0.9751453929904890794 ) ) ;
#10657 = AXIS2_PLACEMENT_3D ( 'NONE', #5444, #5237, #18404 ) ;
#10658 = CARTESIAN_POINT ( 'NONE',  ( 15.85175717768486514, 121.0146182718019645, 0.1572851932169303801 ) ) ;
#10659 = CARTESIAN_POINT ( 'NONE',  ( -6.555005513994535572E-14, 79.34146620154574236, -6.390659674827382268E-18 ) ) ;
#10660 = CARTESIAN_POINT ( 'NONE',  ( 2.108464161424454364, -15.40773383333050894, 5.967785631577029903 ) ) ;
#10661 = FACE_OUTER_BOUND ( 'NONE', #36667, .T. ) ;
#10662 = CARTESIAN_POINT ( 'NONE',  ( -17.14500000000466784, 71.11999999999886768, -1.270000000000000684 ) ) ;
#10663 = CARTESIAN_POINT ( 'NONE',  ( 4.785842063580148853, 158.3075559295907055, 1.719165798332183082 ) ) ;
#10664 = ORIENTED_EDGE ( 'NONE', *, *, #10228, .F. ) ;
#10665 = CARTESIAN_POINT ( 'NONE',  ( -1.660137282266059611, 14.53371390510571004, 8.268994913937449454 ) ) ;
#10666 = CARTESIAN_POINT ( 'NONE',  ( -2.311280081344418313, 117.1825730503849456, -0.6599811042350863799 ) ) ;
#10667 = CARTESIAN_POINT ( 'NONE',  ( -2.416298757281930776, 119.8248006784163380, -0.5703471319689767949 ) ) ;
#10668 = LINE ( 'NONE', #4097, #34745 ) ;
#10669 = DIRECTION ( 'NONE',  ( 0.01997839162482749689, 1.040247600000945640E-18, -0.9998004120163610509 ) ) ;
#10670 = CARTESIAN_POINT ( 'NONE',  ( -5.018108817528237786, 104.6144662015435358, 1.816817646635351613 ) ) ;
#10671 = AXIS2_PLACEMENT_3D ( 'NONE', #28360, #14932, #25167 ) ;
#10672 = CARTESIAN_POINT ( 'NONE',  ( -4.399545650080316506, 2.442302885307133131, -1.471791394725967095 ) ) ;
#10673 = CARTESIAN_POINT ( 'NONE',  ( -5.451267667241070720E-14, 85.80437499999999318, 0.000000000000000000 ) ) ;
#10674 = CARTESIAN_POINT ( 'NONE',  ( -4.848171622920200541, 115.6909491485453003, 1.282745750490223324 ) ) ;
#10675 = CARTESIAN_POINT ( 'NONE',  ( 3.347306494706169477, -13.94864326390300668, 3.303819676456750898 ) ) ;
#10676 = CARTESIAN_POINT ( 'NONE',  ( 3.181806805318111220, 118.0279923103727242, -0.7725587567394767152 ) ) ;
#10677 = CARTESIAN_POINT ( 'NONE',  ( -22.18008199021001303, 150.6715983490228723, 0.5179974990882320052 ) ) ;
#10678 = CYLINDRICAL_SURFACE ( 'NONE', #40105, 2.539999999999999591 ) ;
#10679 = DIRECTION ( 'NONE',  ( 5.188838149069472160E-16, -1.699382548006136559E-16, -1.000000000000000000 ) ) ;
#10680 = AXIS2_PLACEMENT_3D ( 'NONE', #2922, #35291, #38487 ) ;
#10681 = VERTEX_POINT ( 'NONE', #25057 ) ;
#10682 = CARTESIAN_POINT ( 'NONE',  ( -4.382135906878160903, 104.6144662015457811, -2.048376150530189843 ) ) ;
#10683 = CARTESIAN_POINT ( 'NONE',  ( 4.856922264871083250, -15.58127974107270575, 2.741789226191331252 ) ) ;
#10684 = CARTESIAN_POINT ( 'NONE',  ( -20.06821085608268618, 149.3093937917295762, 1.664735353294634290 ) ) ;
#10685 = CARTESIAN_POINT ( 'NONE',  ( -0.2095918955067871126, -8.989892990265463624, -4.636818132431064221 ) ) ;
#10686 = ORIENTED_EDGE ( 'NONE', *, *, #8089, .T. ) ;
#10687 = DIRECTION ( 'NONE',  ( -0.9998004120163608288, 1.039227405372657318E-20, -0.01997839162482760098 ) ) ;
#10688 = CIRCLE ( 'NONE', #33818, 9.048749999999998295 ) ;
#10689 = CARTESIAN_POINT ( 'NONE',  ( 0.3459730346047664717, 118.1497763966932695, 1.075889458897477891 ) ) ;
#10690 =( LENGTH_UNIT ( ) NAMED_UNIT ( * ) SI_UNIT ( .MILLI., .METRE. ) );
#10691 = CARTESIAN_POINT ( 'NONE',  ( -1.906664127224672489, 156.5995568990359175, 1.114948187579593242 ) ) ;
#10692 = CARTESIAN_POINT ( 'NONE',  ( -47.36402082484878662, 19.94680553081675356, 5.177108632069717942 ) ) ;
#10693 = CARTESIAN_POINT ( 'NONE',  ( 18.32188643113664739, 147.9371514012413229, -1.660510838394361866 ) ) ;
#10694 = CARTESIAN_POINT ( 'NONE',  ( -12.41171712301742502, 121.5863879130357503, -1.717582910027388499 ) ) ;
#10695 = DIRECTION ( 'NONE',  ( -0.7284927773988482125, -0.6850534820564830873, 0.000000000000000000 ) ) ;
#10696 = ORIENTED_EDGE ( 'NONE', *, *, #39789, .F. ) ;
#10697 = CARTESIAN_POINT ( 'NONE',  ( 4.118366482596429456, 118.2429491485453354, -0.1862083956823271380 ) ) ;
#10698 = CARTESIAN_POINT ( 'NONE',  ( 4.393282770141039961, 155.8497297829079571, -0.4427821657071675521 ) ) ;
#10699 = ORIENTED_EDGE ( 'NONE', *, *, #41321, .F. ) ;
#10700 = CARTESIAN_POINT ( 'NONE',  ( 2.368424984008928202, -15.31393412036581658, 4.927583237414308037 ) ) ;
#10701 = CARTESIAN_POINT ( 'NONE',  ( -5.008552712180506461, 117.3993836135855560, 0.7755994290793736257 ) ) ;
#10702 = AXIS2_PLACEMENT_3D ( 'NONE', #40966, #12199, #31366 ) ;
#10703 = CARTESIAN_POINT ( 'NONE',  ( -58.36992421181236068, -0.2917964073288620286, -5.103743859794852046E-13 ) ) ;
#10704 = CARTESIAN_POINT ( 'NONE',  ( -4.468841950160419962, 8.124252568732815760, -1.173904233648782158 ) ) ;
#10705 = CARTESIAN_POINT ( 'NONE',  ( -0.008308630153283404207, 120.0570981805881559, 0.4157978282972239481 ) ) ;
#10706 = CARTESIAN_POINT ( 'NONE',  ( 0.3073029101277962583, 33.80961766112287847, 0.5411155679567926091 ) ) ;
#10707 = B_SPLINE_CURVE_WITH_KNOTS ( 'NONE', 3,
 ( #29023, #3695, #42041, #16872, #289, #38631, #32864, #32438, #35857, #12837, #3484, #13476 ),
 .UNSPECIFIED., .F., .F.,
 ( 4, 2, 2, 2, 2, 4 ),
 ( 0.000000000000000000, 0.1320156187279750426, 0.1980234280919625778, 0.2640312374559500852, 0.3918846486443439692, 0.3959276339151724944 ),
 .UNSPECIFIED. ) ;
#10708 = CARTESIAN_POINT ( 'NONE',  ( 0.7007450612751181529, 9.901275517365906609, -4.597291952374415125 ) ) ;
#10709 = CARTESIAN_POINT ( 'NONE',  ( 15.52555164710810232, 147.5317938866932366, 0.3613967763117282850 ) ) ;
#10710 = DIRECTION ( 'NONE',  ( 1.011795553208986377E-16, 1.000000000000000000, -0.000000000000000000 ) ) ;
#10711 = TOROIDAL_SURFACE ( 'NONE', #40650, 8.794749999999998735, 0.2540000000000000036 ) ;
#10712 = CARTESIAN_POINT ( 'NONE',  ( -54.07635852566403400, 7.689673991023174615, -1.154061576158815550 ) ) ;
#10713 = CARTESIAN_POINT ( 'NONE',  ( -5.550348810799227373, 116.7477450504428731, -0.3527803593980367580 ) ) ;
#10714 = CARTESIAN_POINT ( 'NONE',  ( -17.32429653712378936, 61.56493206124108042, -1.269999999999999130 ) ) ;
#10715 = DIRECTION ( 'NONE',  ( 0.01731298258488772612, -0.9998501190848633202, 1.788962107505314604E-16 ) ) ;
#10716 = CARTESIAN_POINT ( 'NONE',  ( -32.57812072184745489, 51.47121137486388420, -1.270000000000005569 ) ) ;
#10717 = CARTESIAN_POINT ( 'NONE',  ( 5.540715274600516160, 6.338079305180906786, 6.343128766557815545 ) ) ;
#10718 = CARTESIAN_POINT ( 'NONE',  ( -46.38316532014830074, 26.05065462784526176, 1.523999999999997357 ) ) ;
#10719 = FACE_OUTER_BOUND ( 'NONE', #33667, .T. ) ;
#10720 = CARTESIAN_POINT ( 'NONE',  ( -58.05887703936295452, 1.806656698574160558, 1.362798277128383972 ) ) ;
#10721 = EDGE_CURVE ( 'NONE', #21991, #6038, #25640, .T. ) ;
#10722 = LINE ( 'NONE', #11144, #24024 ) ;
#10723 = CARTESIAN_POINT ( 'NONE',  ( -15.39314341005352738, 120.8297411738997624, 0.1127201291141931849 ) ) ;
#10724 = VERTEX_POINT ( 'NONE', #14830 ) ;
#10725 = CARTESIAN_POINT ( 'NONE',  ( -55.80532936045926107, 9.325833942460080905, -1.087685647686953452E-14 ) ) ;
#10726 = CARTESIAN_POINT ( 'NONE',  ( 7.800415316508575003, 122.5706186015670767, -0.04211976961263740743 ) ) ;
#10727 = ORIENTED_EDGE ( 'NONE', *, *, #19352, .F. ) ;
#10728 = DIRECTION ( 'NONE',  ( 0.01997839162482749689, 1.040247600000944870E-18, -0.9998004120163610509 ) ) ;
#10729 = CARTESIAN_POINT ( 'NONE',  ( -15.64085066085090681, 147.2198192248932571, -0.3637928714071056446 ) ) ;
#10730 = CARTESIAN_POINT ( 'NONE',  ( 3.233725904218312408, -15.30436843596319463, 5.598328752637605099 ) ) ;
#10731 = CARTESIAN_POINT ( 'NONE',  ( -4.041216738203083914, 118.0179939250997023, 0.7376333572805303662 ) ) ;
#10732 = CARTESIAN_POINT ( 'NONE',  ( -4.050807963365556930, 30.95410787014092335, -2.229501126309402448 ) ) ;
#10733 = CARTESIAN_POINT ( 'NONE',  ( 23.12711913739482839, 149.5941399179437781, 0.9155080916133792046 ) ) ;
#10734 = CARTESIAN_POINT ( 'NONE',  ( -8.473844426907703564, 67.77203500197072117, 1.524000000000003574 ) ) ;
#10735 = CARTESIAN_POINT ( 'NONE',  ( 4.377640660406503237, 26.40621510375495973, 1.544744264128281364 ) ) ;
#10736 = CARTESIAN_POINT ( 'NONE',  ( -0.06867543354984582959, -8.127513596672324425, -0.9731866935420671050 ) ) ;
#10737 = CARTESIAN_POINT ( 'NONE',  ( -22.64163882069516376, 150.6401102206664291, -0.6810593374908544551 ) ) ;
#10738 = CARTESIAN_POINT ( 'NONE',  ( -15.71196903609989981, 80.05455644220629097, 1.269999999999997575 ) ) ;
#10739 = EDGE_CURVE ( 'NONE', #14389, #11424, #16282, .T. ) ;
#10740 = CARTESIAN_POINT ( 'NONE',  ( 4.862091962581056137, 117.4116108956684030, 1.165648838277617338 ) ) ;
#10741 = ORIENTED_EDGE ( 'NONE', *, *, #29867, .F. ) ;
#10742 = CARTESIAN_POINT ( 'NONE',  ( -5.551342799028650354, 116.9755805007568483, 0.3845323937588601138 ) ) ;
#10743 = CARTESIAN_POINT ( 'NONE',  ( -10.18365381109015821, 122.2967958330617648, 1.106735498401915985 ) ) ;
#10744 = CARTESIAN_POINT ( 'NONE',  ( -57.61623536216810493, 1.334194615165582576, -1.288300599212580888 ) ) ;
#10745 = CARTESIAN_POINT ( 'NONE',  ( 7.877908914988192457, 118.7344292658239340, 1.218006232967851377 ) ) ;
#10746 = CARTESIAN_POINT ( 'NONE',  ( 12.77186547895197499, 122.8260676081006153, -1.334005200199291252 ) ) ;
#10747 = CARTESIAN_POINT ( 'NONE',  ( -0.7316449863892299232, -12.60219034754442902, -0.6469547163463490458 ) ) ;
#10748 = CARTESIAN_POINT ( 'NONE',  ( -20.80232463633032225, 150.1670661137953289, -2.219268881695795059 ) ) ;
#10749 = CARTESIAN_POINT ( 'NONE',  ( -44.96292901393739072, 21.56701576681934540, -3.486870777078513228 ) ) ;
#10750 = CARTESIAN_POINT ( 'NONE',  ( 4.835304301806635507, 104.6144662015456959, -0.09947441844414706136 ) ) ;
#10751 = CARTESIAN_POINT ( 'NONE',  ( 13.14213916796041559, 130.8944540161131442, -0.9043360416341283958 ) ) ;
#10752 = CARTESIAN_POINT ( 'NONE',  ( 7.836112336079962049, 122.3275008022818326, 0.6979122178994436876 ) ) ;
#10753 = ORIENTED_EDGE ( 'NONE', *, *, #39902, .F. ) ;
#10754 = CARTESIAN_POINT ( 'NONE',  ( -17.85978967527205441, 148.7876888829155746, -2.377023446492704473 ) ) ;
#10755 = CARTESIAN_POINT ( 'NONE',  ( 3.150932678494966055, -15.78083729861913476, 4.935700751529307873 ) ) ;
#10756 = DIRECTION ( 'NONE',  ( 0.8745520943968235761, -0.4849315768086558398, 0.000000000000000000 ) ) ;
#10757 = CARTESIAN_POINT ( 'NONE',  ( -4.680464983510406185, 117.9617385798577942, -0.8792464480512792724 ) ) ;
#10758 = EDGE_CURVE ( 'NONE', #13951, #22153, #41478, .T. ) ;
#10759 = CARTESIAN_POINT ( 'NONE',  ( -53.45432727069204759, 10.77832982246877691, -4.078803160923793136 ) ) ;
#10760 = CARTESIAN_POINT ( 'NONE',  ( 4.065926199369043204, 118.2429491485453497, 0.3080910687088499467 ) ) ;
#10761 = CARTESIAN_POINT ( 'NONE',  ( 11.51381720411931830, 123.3156264706956478, 1.674137098916062660 ) ) ;
#10762 = DIRECTION ( 'NONE',  ( -5.463695987328526437E-16, -1.000000000000000000, -1.672774450599033775E-31 ) ) ;
#10763 = EDGE_CURVE ( 'NONE', #22953, #14753, #31763, .T. ) ;
#10764 = CARTESIAN_POINT ( 'NONE',  ( 15.72215902125767606, 120.8394623874526275, 0.2972128523334376382 ) ) ;
#10765 = AXIS2_PLACEMENT_3D ( 'NONE', #13216, #6204, #10219 ) ;
#10766 = EDGE_CURVE ( 'NONE', #6407, #1559, #18144, .T. ) ;
#10767 = CARTESIAN_POINT ( 'NONE',  ( 6.775881838314501415, 16.25650946394821617, 5.045332117489572887 ) ) ;
#10768 = CARTESIAN_POINT ( 'NONE',  ( 0.6211475606395560067, 120.8480686026657196, 0.1701230225530363793 ) ) ;
#10769 = CARTESIAN_POINT ( 'NONE',  ( 3.136615966272614742, 159.3365417412370562, -0.7296721229192899560 ) ) ;
#10770 = CARTESIAN_POINT ( 'NONE',  ( -17.09258512000246100, 84.17916046765628835, 1.523999999999996469 ) ) ;
#10771 = FACE_OUTER_BOUND ( 'NONE', #35325, .T. ) ;
#10772 = CARTESIAN_POINT ( 'NONE',  ( -8.070121050663757956, 158.6666700270975525, -0.1062422583151902272 ) ) ;
#10773 = ORIENTED_EDGE ( 'NONE', *, *, #25441, .F. ) ;
#10774 = CARTESIAN_POINT ( 'NONE',  ( -46.60530155212499892, 26.17382724835484709, -0.6632222222222314834 ) ) ;
#10775 = CARTESIAN_POINT ( 'NONE',  ( 5.711181965518192349, 121.0140050728914076, -0.3875387523984055727 ) ) ;
#10776 = CARTESIAN_POINT ( 'NONE',  ( 6.475569851349685990, -13.49999789469196365, 0.1848929821133123153 ) ) ;
#10777 = DIRECTION ( 'NONE',  ( 5.188838149069472160E-16, -1.699382548006136559E-16, -1.000000000000000000 ) ) ;
#10778 = CARTESIAN_POINT ( 'NONE',  ( -0.6563489144271578146, 156.3175253132196190, -0.2722359314208550041 ) ) ;
#10779 = CARTESIAN_POINT ( 'NONE',  ( 2.009495809369673314, -15.14277677434763802, 5.899592854099822148 ) ) ;
#10780 = VECTOR ( 'NONE', #26225, 1000.000000000000000 ) ;
#10781 = CARTESIAN_POINT ( 'NONE',  ( -4.901524533163420294, 117.5843641943970681, 0.6192240155325965389 ) ) ;
#10782 = CARTESIAN_POINT ( 'NONE',  ( -41.08173151913482002, 23.06272320883524785, 1.524000000019140932 ) ) ;
#10783 = CARTESIAN_POINT ( 'NONE',  ( 22.53260066761437486, 150.7862151120626777, 0.5269028172337441029 ) ) ;
#10784 = ORIENTED_EDGE ( 'NONE', *, *, #36085, .F. ) ;
#10785 = CARTESIAN_POINT ( 'NONE',  ( 3.745621265272091716, -10.50169880513956322, -2.708184146228840294 ) ) ;
#10786 = CARTESIAN_POINT ( 'NONE',  ( -22.66341594453909281, 150.6395781703034231, -0.4783972420343528542 ) ) ;
#10787 = MANIFOLD_SOLID_BREP ( 'Stock-MAS-162-1', #2672 ) ;
#10788 = DIRECTION ( 'NONE',  ( -5.188838149069472160E-16, 1.699382548006136559E-16, 1.000000000000000000 ) ) ;
#10789 = CYLINDRICAL_SURFACE ( 'NONE', #17666, 1.270000000000000240 ) ;
#10790 = ORIENTED_EDGE ( 'NONE', *, *, #12808, .F. ) ;
#10791 = CARTESIAN_POINT ( 'NONE',  ( 6.543339688405037435, 119.8646354556796894, 1.246904736843251982 ) ) ;
#10792 = CARTESIAN_POINT ( 'NONE',  ( 3.235533175430977515, 2.501875212487111977, 3.308963532380430284 ) ) ;
#10793 = CARTESIAN_POINT ( 'NONE',  ( 19.75679031132823127, 152.3633698111425758, 1.804147069793666347 ) ) ;
#10794 = CARTESIAN_POINT ( 'NONE',  ( -55.40724689661794855, 6.067898552060245088, -3.000206617153963418 ) ) ;
#10796 = CARTESIAN_POINT ( 'NONE',  ( 5.883429839103449410, 118.5625182843610617, -0.8957466683066145352 ) ) ;
#10795 = CARTESIAN_POINT ( 'NONE',  ( 5.941785710906973605, 57.15000000000325997, 5.016500000000000625 ) ) ;
#10797 = CARTESIAN_POINT ( 'NONE',  ( 4.571311019248293306, -6.119132638730012452, 0.7325351754658009362 ) ) ;
#10798 = CARTESIAN_POINT ( 'NONE',  ( -10.35357550766360646, 157.8614378686282862, -1.168524991271691515 ) ) ;
#10799 = ORIENTED_EDGE ( 'NONE', *, *, #28499, .F. ) ;
#10800 = EDGE_CURVE ( 'NONE', #24363, #15693, #21541, .T. ) ;
#10801 = CARTESIAN_POINT ( 'NONE',  ( -10.33307603652750828, 126.0505730134521230, -0.02860894079130314391 ) ) ;
#10803 = CARTESIAN_POINT ( 'NONE',  ( 6.002709446384779213, -13.95775275001606630, 2.224537231649871494 ) ) ;
#10802 = CIRCLE ( 'NONE', #41413, 9.048749999999998295 ) ;
#10804 = CIRCLE ( 'NONE', #11465, 6.349999999999999645 ) ;
#10805 = CARTESIAN_POINT ( 'NONE',  ( -6.604303299200508256E-14, 94.83546620154572793, -1.207165459215201580E-19 ) ) ;
#10806 = CARTESIAN_POINT ( 'NONE',  ( -0.08181223041124258133, 118.1651005001092045, -0.8941161664445478330 ) ) ;
#10807 = EDGE_LOOP ( 'NONE', ( #32374, #9668 ) ) ;
#10808 = CARTESIAN_POINT ( 'NONE',  ( 11.41083474541176024, 122.2847249198043471, 1.726555165334429987 ) ) ;
#10809 = CARTESIAN_POINT ( 'NONE',  ( -29.89586364642803318, 71.55302121702176521, -1.524000000000007571 ) ) ;
#10810 = CARTESIAN_POINT ( 'NONE',  ( -30.02342128825639023, 69.55262966049605211, -1.270000000000007123 ) ) ;
#10811 = CARTESIAN_POINT ( 'NONE',  ( -2.968319594835739483, 117.2422168882539211, 0.4889809032577733250 ) ) ;
#10812 = EDGE_CURVE ( 'NONE', #14129, #35669, #32457, .T. ) ;
#10813 = CARTESIAN_POINT ( 'NONE',  ( 2.407351327831447119, 1.847773219181642057, 8.093752867084216263 ) ) ;
#10814 = CARTESIAN_POINT ( 'NONE',  ( 11.38067935084455762, 126.1532465342912985, 1.245950066931533096 ) ) ;
#10815 = CARTESIAN_POINT ( 'NONE',  ( -3.682264917456323783, 82.13546620154573930, -0.07358041635423923088 ) ) ;
#10816 = CARTESIAN_POINT ( 'NONE',  ( 15.74805233916999292, 121.4292885696920621, -0.3002298764450369584 ) ) ;
#10817 = CARTESIAN_POINT ( 'NONE',  ( -16.46263872254443683, 83.91929436251373886, 1.269999999999996687 ) ) ;
#10818 = CARTESIAN_POINT ( 'NONE',  ( -53.56064905838539403, 9.687610447046496986, 3.641404713838447105 ) ) ;
#10819 = CARTESIAN_POINT ( 'NONE',  ( -49.15418727280429323, 24.05022843951647715, -9.137385882761073034E-15 ) ) ;
#10820 = CARTESIAN_POINT ( 'NONE',  ( -50.29507671575587580, 15.72791930032350827, 4.796563717952097683 ) ) ;
#10821 = CARTESIAN_POINT ( 'NONE',  ( -58.65389498535380852, -0.3158197163193834367, 0.3266806156710039266 ) ) ;
#10822 = CARTESIAN_POINT ( 'NONE',  ( -4.447578949651058267, 118.1635636769329665, 0.4463883187089059401 ) ) ;
#10823 = DIRECTION ( 'NONE',  ( -5.188838149069472160E-16, 1.699382548006136559E-16, 1.000000000000000000 ) ) ;
#10824 = EDGE_LOOP ( 'NONE', ( #17908, #40243, #6262, #19009 ) ) ;
#10825 = CARTESIAN_POINT ( 'NONE',  ( -45.82931853585290582, 22.14969803457954356, 3.600065900675641029 ) ) ;
#10826 = AXIS2_PLACEMENT_3D ( 'NONE', #30070, #41656, #33277 ) ;
#10827 = CARTESIAN_POINT ( 'NONE',  ( -6.079163865392237298, 119.4949355251708454, -1.258858988448749106 ) ) ;
#10828 = TOROIDAL_SURFACE ( 'NONE', #42142, 15.36699999999999555, 0.6350000000000000089 ) ;
#10829 = CARTESIAN_POINT ( 'NONE',  ( -7.639005212201317896, 124.2918010433613745, -0.1615048153450349133 ) ) ;
#10830 = CARTESIAN_POINT ( 'NONE',  ( 4.468651703854161994, 118.1302808690484625, 0.7051366077090519546 ) ) ;
#10831 = CARTESIAN_POINT ( 'NONE',  ( -6.262986112992452448, 155.3815620563194955, -0.9009107504210206452 ) ) ;
#10832 = CYLINDRICAL_SURFACE ( 'NONE', #15176, 5.588000000000006295 ) ;
#10833 = CARTESIAN_POINT ( 'NONE',  ( 3.202712377253894793, 117.9496042817458914, -1.175034297761716529 ) ) ;
#10834 = CARTESIAN_POINT ( 'NONE',  ( -10.14627733936766241, 123.6566696788710686, -1.220144418243291007 ) ) ;
#10835 = DIRECTION ( 'NONE',  ( -0.8745520943968245753, 0.4849315768086539524, -5.691349986800526185E-16 ) ) ;
#10836 = CARTESIAN_POINT ( 'NONE',  ( -46.53702275532343435, 20.69065974945542763, 4.840627275220680481 ) ) ;
#10837 = CARTESIAN_POINT ( 'NONE',  ( -25.80936006922821591, 73.72935646344811289, 1.269999999999992468 ) ) ;
#10838 = CARTESIAN_POINT ( 'NONE',  ( -7.534622205921475135, 122.4254553736845281, -0.03076868180150949678 ) ) ;
#10839 = DIRECTION ( 'NONE',  ( -0.8745520943968250194, 0.4849315768086532863, -5.361993529360574930E-16 ) ) ;
#10840 = CARTESIAN_POINT ( 'NONE',  ( 1.349732659537954405, 159.5224216140176168, 0.6194554754934781249 ) ) ;
#10841 = CYLINDRICAL_SURFACE ( 'NONE', #19739, 13.46199999999999619 ) ;
#10842 = CARTESIAN_POINT ( 'NONE',  ( 3.189131052002434963, -14.84934909478852205, 3.295817422932660890 ) ) ;
#10843 = CARTESIAN_POINT ( 'NONE',  ( -5.080524353911874513, 119.7208665877771665, 0.8394179162009565154 ) ) ;
#10844 = CARTESIAN_POINT ( 'NONE',  ( -0.02964290590182637811, -9.142985105544495283, 0.9735349185509928338 ) ) ;
#10845 = CARTESIAN_POINT ( 'NONE',  ( -5.618954885709059432, 159.1014311945586712, -0.6070295849213356298 ) ) ;
#10846 = CARTESIAN_POINT ( 'NONE',  ( -0.8651787172165069650, -5.103258934911358402, 0.4504873164067982327 ) ) ;
#10847 = EDGE_LOOP ( 'NONE', ( #28065, #40856, #9196, #9902 ) ) ;
#10848 = CARTESIAN_POINT ( 'NONE',  ( -49.86808358410245745, 14.13890166617936472, 1.547476669397152671 ) ) ;
#10849 = CARTESIAN_POINT ( 'NONE',  ( 3.418449710216091564, 108.6681208952157078, 4.126741282752677265 ) ) ;
#10850 = CARTESIAN_POINT ( 'NONE',  ( -5.897637645108146032, 121.3687970875902806, 0.2476274089428441572 ) ) ;
#10851 = CARTESIAN_POINT ( 'NONE',  ( 3.029556690758328674, -14.73736909467317169, 5.484434072839230012 ) ) ;
#10852 = CARTESIAN_POINT ( 'NONE',  ( 13.22964523056185193, 152.2904283036577908, -1.375236710735037837 ) ) ;
#10853 = ORIENTED_EDGE ( 'NONE', *, *, #21990, .F. ) ;
#10854 = CARTESIAN_POINT ( 'NONE',  ( -6.656653968794013387, 119.6463993818898359, -1.283952750486249572 ) ) ;
#10855 = CARTESIAN_POINT ( 'NONE',  ( -4.808149584360944750, 104.6144662015457243, 0.4147572885131461939 ) ) ;
#10856 = CARTESIAN_POINT ( 'NONE',  ( 2.932272473696061255, -14.72556872895393276, 4.151486945341092749 ) ) ;
#10857 = CYLINDRICAL_SURFACE ( 'NONE', #14979, 0.2540000000000015024 ) ;
#10858 = CARTESIAN_POINT ( 'NONE',  ( 9.295404511957237048, 124.2653519604415067, 0.02360630055292711402 ) ) ;
#10859 = AXIS2_PLACEMENT_3D ( 'NONE', #18341, #22155, #2401 ) ;
#10860 = ORIENTED_EDGE ( 'NONE', *, *, #26102, .F. ) ;
#10861 = CARTESIAN_POINT ( 'NONE',  ( -3.443790112798272407, 108.1634672882648118, 4.064613902700619619 ) ) ;
#10863 = EDGE_CURVE ( 'NONE', #1745, #38547, #7989, .T. ) ;
#10862 = DIRECTION ( 'NONE',  ( 0.9998004120163609398, 4.016384292689130894E-17, 0.01997839162482749689 ) ) ;
#10864 = AXIS2_PLACEMENT_3D ( 'NONE', #35313, #6141, #28494 ) ;
#10865 = DIRECTION ( 'NONE',  ( 1.000000000000000000, -9.627370216492862708E-17, 0.000000000000000000 ) ) ;
#10866 = EDGE_CURVE ( 'NONE', #26975, #41779, #14084, .T. ) ;
#10867 = FACE_OUTER_BOUND ( 'NONE', #35013, .T. ) ;
#10868 = CARTESIAN_POINT ( 'NONE',  ( 22.65077213736919859, 150.6401102206664291, 0.2239908233986879216 ) ) ;
#10869 = DIRECTION ( 'NONE',  ( 0.3582377630124009560, -0.9336303900108815501, 3.445432962228709470E-16 ) ) ;
#10870 = CARTESIAN_POINT ( 'NONE',  ( 1.944882249840667710, -15.28710494480188586, 6.001156021306252697 ) ) ;
#10871 = CARTESIAN_POINT ( 'NONE',  ( 12.21488373879589062, 55.24500000000000455, 5.016499999999999737 ) ) ;
#10872 = CARTESIAN_POINT ( 'NONE',  ( 3.009276887026297143, 39.20946620154573026, -1.210121013456480599 ) ) ;
#10873 = CARTESIAN_POINT ( 'NONE',  ( 20.67294874948561656, 147.9587796579421308, 2.444796510662507583 ) ) ;
#10874 = ORIENTED_EDGE ( 'NONE', *, *, #34502, .F. ) ;
#10875 = CARTESIAN_POINT ( 'NONE',  ( -3.240848860066210868, 23.83156553091082230, 7.781828003744739597 ) ) ;
#10876 = CARTESIAN_POINT ( 'NONE',  ( 8.690636420055867006, 118.2864455517542552, -0.6276685427593149402 ) ) ;
#10877 = CARTESIAN_POINT ( 'NONE',  ( -5.572611807913307125, 123.3023672762779910, -0.1864456790743028447 ) ) ;
#10879 = CARTESIAN_POINT ( 'NONE',  ( -5.974493989214139766, 78.88147413144915276, 5.016500000000001513 ) ) ;
#10878 = B_SPLINE_CURVE_WITH_KNOTS ( 'NONE', 3,
 ( #24972, #24536, #17727, #41390, #11553, #8796, #34361, #4983, #18571, #37971, #18147, #14744, #21754, #27953, #1991, #14953, #11349 ),
 .UNSPECIFIED., .F., .F.,
 ( 4, 1, 1, 1, 1, 1, 1, 1, 1, 1, 1, 1, 1, 1, 4 ),
 ( 0.000000000000000000, 0.08300113939718137268, 0.1732806554784933895, 0.2717672377176819087, 0.3752096606209606167, 0.4787223716043260135, 0.5772295444745598747, 0.6668133826162351285, 0.7470991451079272982, 0.7815930070524458317, 0.8169452614683294644, 0.8547689062991584708, 0.8968063284581728745, 0.9447228702782888288, 1.000000000000000000 ),
 .UNSPECIFIED. ) ;
#10880 = FACE_OUTER_BOUND ( 'NONE', #30927, .T. ) ;
#10881 = CARTESIAN_POINT ( 'NONE',  ( -4.722986921911269675, 104.6144662015457811, 1.042082363010505164 ) ) ;
#10882 = CARTESIAN_POINT ( 'NONE',  ( 3.345514242732226418, 6.565394131763864216, 3.211428121085859733 ) ) ;
#10883 = DIRECTION ( 'NONE',  ( 1.000000000000000000, 0.000000000000000000, 0.000000000000000000 ) ) ;
#10884 = CARTESIAN_POINT ( 'NONE',  ( 3.136003201302111076, -14.34114629734795088, 4.029177829137042366 ) ) ;
#10885 = CARTESIAN_POINT ( 'NONE',  ( 2.458941639547435720, 111.1666841684333633, -3.140650435616773262 ) ) ;
#10886 = CARTESIAN_POINT ( 'NONE',  ( -5.853624122459167189, 117.3024554866451865, 0.4121555180536240481 ) ) ;
#10887 = VECTOR ( 'NONE', #8723, 1000.000000000000000 ) ;
#10888 = CARTESIAN_POINT ( 'NONE',  ( -4.462110519195587877, 27.89918626506305444, 0.8161882792947469101 ) ) ;
#10889 = CARTESIAN_POINT ( 'NONE',  ( -3.630816577625875226E-14, 57.14999999999999147, 0.000000000000000000 ) ) ;
#10890 = ORIENTED_EDGE ( 'NONE', *, *, #31808, .T. ) ;
#10891 = CYLINDRICAL_SURFACE ( 'NONE', #216, 0.2540000000000005032 ) ;
#10892 = CARTESIAN_POINT ( 'NONE',  ( 4.827739681024636909, -15.50696398224166117, 1.464145260785405522 ) ) ;
#10893 = CARTESIAN_POINT ( 'NONE',  ( -10.04363327864691158, 120.6268241347409855, 1.191437567882422943 ) ) ;
#10894 = CARTESIAN_POINT ( 'NONE',  ( 0.1724166890850278577, 29.87817833284422875, -0.9617850639438362270 ) ) ;
#10895 = ORIENTED_EDGE ( 'NONE', *, *, #6446, .F. ) ;
#10896 = CARTESIAN_POINT ( 'NONE',  ( -3.932819197772146946, 27.98301002373793978, 0.4898618918306564263 ) ) ;
#10897 = CARTESIAN_POINT ( 'NONE',  ( 0.03413713131413576019, 107.6766875080336376, 4.617405654744151988 ) ) ;
#10898 = CARTESIAN_POINT ( 'NONE',  ( -0.5800011805208045157, 120.2131932824006526, 0.3882866552237520530 ) ) ;
#10899 = CARTESIAN_POINT ( 'NONE',  ( -4.934731464961845226, 117.4065818953012155, -1.087731638897137643 ) ) ;
#10900 = CARTESIAN_POINT ( 'NONE',  ( 15.78846850359692411, 131.3838724160208926, -1.599517327752104201 ) ) ;
#10901 = CARTESIAN_POINT ( 'NONE',  ( -18.19503446209947128, 151.8090458617612057, -2.356823057848427716 ) ) ;
#10902 = DIRECTION ( 'NONE',  ( 5.188838149069472160E-16, -1.699382548006136559E-16, -1.000000000000000000 ) ) ;
#10903 = AXIS2_PLACEMENT_3D ( 'NONE', #36480, #23668, #16870 ) ;
#10904 = CARTESIAN_POINT ( 'NONE',  ( 4.297048582020653207, 118.2143428055317855, -0.3468108124363870060 ) ) ;
#10905 = CARTESIAN_POINT ( 'NONE',  ( 1.566048506583572308, 120.7946061759640486, -0.1772761409975699420 ) ) ;
#10906 = ORIENTED_EDGE ( 'NONE', *, *, #36900, .T. ) ;
#10907 = CARTESIAN_POINT ( 'NONE',  ( 2.245555723253176872, -15.32365336378345511, 5.046800657416122604 ) ) ;
#10908 = AXIS2_PLACEMENT_3D ( 'NONE', #39481, #39697, #33092 ) ;
#10909 = CARTESIAN_POINT ( 'NONE',  ( 11.62920297224776611, 55.59919541885983563, -5.016499999999893156 ) ) ;
#10910 = CARTESIAN_POINT ( 'NONE',  ( -58.36222274556690337, -0.2757005147488722496, 0.1096927518865258300 ) ) ;
#10911 = EDGE_CURVE ( 'NONE', #30952, #1883, #16309, .T. ) ;
#10912 = CARTESIAN_POINT ( 'NONE',  ( -4.168830513765062307, 9.198770455692846681, 1.997586429550192166 ) ) ;
#10913 = CARTESIAN_POINT ( 'NONE',  ( 10.28893712963043328, 123.4707319107414492, 1.320145760562476900 ) ) ;
#10914 = CARTESIAN_POINT ( 'NONE',  ( -2.184147097501310419, 31.48929697360260249, 1.237019084378400580 ) ) ;
#10915 = CARTESIAN_POINT ( 'NONE',  ( -7.618479139564731106, 124.7215218652630710, -0.1522353441811856445 ) ) ;
#10916 = VECTOR ( 'NONE', #36355, 1000.000000000000114 ) ;
#10917 = CARTESIAN_POINT ( 'NONE',  ( 1.893578447776079754, 19.08455809737888487, -4.224370802633358402 ) ) ;
#10918 = CARTESIAN_POINT ( 'NONE',  ( 7.787205264484002853, 154.6472212274131550, 0.1983306932048341242 ) ) ;
#10919 = DIRECTION ( 'NONE',  ( 0.9469626219732538708, 0.3213437296502617002, 6.686393187109395313E-16 ) ) ;
#10920 = CARTESIAN_POINT ( 'NONE',  ( -56.42856387642236626, 3.193865871111118082, -0.1553879740656047281 ) ) ;
#10921 = CARTESIAN_POINT ( 'NONE',  ( 5.561512006252619322, 116.7374906030325263, -0.1055575561059139272 ) ) ;
#10922 = DIRECTION ( 'NONE',  ( -0.8745520943968240202, 0.4849315768086553402, -5.361993529360572958E-16 ) ) ;
#10923 = CARTESIAN_POINT ( 'NONE',  ( 10.92199999999999704, 57.78500000000000369, 5.016499999999999737 ) ) ;
#10924 = CARTESIAN_POINT ( 'NONE',  ( 1.975136073220359556, -15.70315947173593685, 5.621751108460161461 ) ) ;
#10925 = CARTESIAN_POINT ( 'NONE',  ( -29.18709815851897815, 67.04824513550720155, -1.524000000000006461 ) ) ;
#10926 = AXIS2_PLACEMENT_3D ( 'NONE', #36123, #16503, #13102 ) ;
#10927 = CARTESIAN_POINT ( 'NONE',  ( -3.339872139798120809, 10.66371166075841437, -7.743087711851694088 ) ) ;
#10928 = CARTESIAN_POINT ( 'NONE',  ( -4.737240446979679831, 56.51499999999999346, 4.914900000000012703 ) ) ;
#10929 = DIRECTION ( 'NONE',  ( 1.011795553208986377E-16, 1.000000000000000000, -0.000000000000000000 ) ) ;
#10930 = CARTESIAN_POINT ( 'NONE',  ( -58.10740272659374739, 1.828491270143103975, 0.5949618876680204949 ) ) ;
#10931 = DIRECTION ( 'NONE',  ( -5.188838149069471174E-16, 1.699382548006136313E-16, 1.000000000000000000 ) ) ;
#10932 = CARTESIAN_POINT ( 'NONE',  ( -23.22010346901286937, 149.3105122542552863, -0.009921264925044727401 ) ) ;
#10933 = VERTEX_POINT ( 'NONE', #12285 ) ;
#10934 = CARTESIAN_POINT ( 'NONE',  ( -58.19197273006702886, 1.486408586729007109, -1.232490673556632332 ) ) ;
#10935 = DIRECTION ( 'NONE',  ( -0.000000000000000000, -1.000000000000000000, -0.000000000000000000 ) ) ;
#10936 = VERTEX_POINT ( 'NONE', #12703 ) ;
#10937 = CARTESIAN_POINT ( 'NONE',  ( -47.60342124590309254, 19.66962190513607212, -5.193532021806997356 ) ) ;
#10939 = CARTESIAN_POINT ( 'NONE',  ( -5.659482139215807714E-14, 120.9974662015457341, 3.101038099172001777E-16 ) ) ;
#10938 = AXIS2_PLACEMENT_3D ( 'NONE', #31718, #21475, #8931 ) ;
#10940 = CARTESIAN_POINT ( 'NONE',  ( 4.375071722208805802, -15.20633266255931559, 4.762636924185132514 ) ) ;
#10941 = CARTESIAN_POINT ( 'NONE',  ( -18.41670328667959566, 131.7683309214445728, 1.453117541724253670 ) ) ;
#10942 = CARTESIAN_POINT ( 'NONE',  ( 13.43369120214907397, 119.6710471929552000, 0.6668731667128946494 ) ) ;
#10943 = CARTESIAN_POINT ( 'NONE',  ( 9.086436585086531181, 153.9805727688486456, 0.3555968032218797537 ) ) ;
#10944 = DIRECTION ( 'NONE',  ( 5.188838149069472160E-16, -1.699382548006136559E-16, -1.000000000000000000 ) ) ;
#10945 = CARTESIAN_POINT ( 'NONE',  ( -22.79149376799281868, 150.3987591554885626, -0.7843734907460312433 ) ) ;
#10946 = CARTESIAN_POINT ( 'NONE',  ( -52.88939467130921912, 11.33278677544117841, -4.135169601362077785 ) ) ;
#10947 = DIRECTION ( 'NONE',  ( -0.8745520943968236871, 0.4849315768086558953, -5.361993529360571971E-16 ) ) ;
#10948 = VERTEX_POINT ( 'NONE', #38697 ) ;
#10949 = CARTESIAN_POINT ( 'NONE',  ( -8.758561883465446840, 117.9281413055073529, 0.3499703560493910848 ) ) ;
#10950 = CARTESIAN_POINT ( 'NONE',  ( -6.615874392072807808, 120.4115791468657903, 0.8913422009562911308 ) ) ;
#10951 = CARTESIAN_POINT ( 'NONE',  ( -58.19487492224605774, 0.08271841185791539708, -0.5637723373511558389 ) ) ;
#10952 = EDGE_CURVE ( 'NONE', #4427, #29032, #31786, .T. ) ;
#10953 = CARTESIAN_POINT ( 'NONE',  ( 7.655434399951916546, 119.7866739149480253, -1.082013720931114698 ) ) ;
#10954 = CARTESIAN_POINT ( 'NONE',  ( 0.4928529169951482158, -8.289340824275994279, 0.8415213476199340237 ) ) ;
#10955 = CARTESIAN_POINT ( 'NONE',  ( -0.3865025759031381902, 117.6538564835029206, -0.5089310662413599751 ) ) ;
#10956 = CARTESIAN_POINT ( 'NONE',  ( -46.30033180095409051, 21.65562830348028456, -4.292083522273610008 ) ) ;
#10957 = CARTESIAN_POINT ( 'NONE',  ( 4.076263842838947049, 104.6144662015456817, 2.604289233408977111 ) ) ;
#10958 = EDGE_CURVE ( 'NONE', #29270, #8806, #32064, .T. ) ;
#10959 = CARTESIAN_POINT ( 'NONE',  ( 16.09504119906499753, 148.0691544347876345, -0.9470067175600010989 ) ) ;
#10960 = CARTESIAN_POINT ( 'NONE',  ( 7.784012320830338005, 122.6313477005580665, 0.1555430910899518460 ) ) ;
#10961 = ORIENTED_EDGE ( 'NONE', *, *, #24547, .T. ) ;
#10962 = CARTESIAN_POINT ( 'NONE',  ( -9.373281424700515174, 121.4347015428822374, -1.498606428831740889 ) ) ;
#10963 = CARTESIAN_POINT ( 'NONE',  ( 2.830806653267172734, -15.77471167405206032, 5.191726263073638492 ) ) ;
#10964 = DIRECTION ( 'NONE',  ( -6.353134868986659519E-16, 1.000000000000000000, 0.000000000000000000 ) ) ;
#10965 = CARTESIAN_POINT ( 'NONE',  ( -4.407290876230779197, 118.1655354096973554, -0.6431967494569043042 ) ) ;
#10966 = CIRCLE ( 'NONE', #12337, 0.5080000000000002292 ) ;
#10967 = ADVANCED_FACE ( 'NONE', ( #9924 ), #13428, .T. ) ;
#10968 = CARTESIAN_POINT ( 'NONE',  ( -50.36516092884956208, 15.79195539882771726, -4.916963016749614113 ) ) ;
#10969 = CARTESIAN_POINT ( 'NONE',  ( 4.065926199369043204, 118.2429491485453354, 0.3080910687088499467 ) ) ;
#10970 = B_SPLINE_SURFACE_WITH_KNOTS ( 'NONE', 3, 3, ( 
 ( #15978, #28975, #41995, #32391, #3223, #16184, #29188, #38168, #34, #25992, #39001, #35809, #2396, #15355, #41368, #8981, #33036, #3864, #29623, #30243, #7261, #669, #23630, #20431, #3649, #39210, #7051, #40064, #32820, #6831, #1084, #10018, #16400, #39421, #33459 ),
 ( #20221, #19802, #20018, #26629, #27056, #10226, #23845, #7681, #7472, #14052, #29405, #10856, #10649, #33248, #22990, #36866, #30035, #4286, #16829, #16616, #36443, #36650, #23196, #459, #29831, #17250, #39636, #13432, #13637, #13847, #36230, #32602, #26418, #4077, #245 ),
 ( #875, #10442, #26846, #23413, #17036, #3435, #39853, #13223, #26206, #36016, #11277, #33670, #24466, #8087, #40278, #14670, #8510, #21060, #14879, #14462, #1507, #4494, #30870, #27881, #40483, #27474, #21469, #17454, #5125, #14253, #11071, #24261, #37268, #20850, #40890 ),
 ( #18076, #34295, #37470, #31079, #34499, #8297, #20640, #34086, #1714, #1297, #11477, #40685, #30453, #7888, #27674, #37688, #27262, #24055, #37070, #33877, #4915, #17869, #11694, #4706, #17659, #21266, #30660, #1918, #24680, #38375, #2604, #34973, #9189, #5796, #37734 ),
 ( #11744, #24731, #22145, #28567, #8558, #21731, #35176, #35378, #6003, #22353, #41148, #18965, #31972, #9390, #18123, #31761, #41364, #27929, #18752, #24945, #41575, #15351, #12384, #15137, #8771, #41785, #34551, #38163, #8977, #34753, #18543, #1965, #25371, #28356, #21518 ),
 ( #31128, #5376, #2178, #37946, #28140, #31546, #15770, #15563, #2809, #28775, #12585, #18331, #14929, #40936, #25574, #38578, #31334, #11954, #5587, #2392, #12167, #25163, #21944, #32597, #9806, #12787, #19587, #26624, #28971, #13218, #32184, #7047, #25777, #6827, #30 ),
 ( #3860, #25988, #6207, #10222, #10437, #10013, #3017, #15974, #29826, #16395, #6411, #19383, #6619, #9595, #16180, #454, #19178, #22565, #32387, #38997, #29183, #3430, #16824, #3646, #32816, #19796, #36013, #38785, #23408, #41990, #23191, #20013, #35594, #665, #39632 ),
 ( #3218, #12994, #26414, #13426, #22774, #35805, #29401, #241, #26201, #39418, #13633, #39205, #22986, #16611, #29619, #36225, #33032, #14047, #36439, #40479, #40680, #40272, #33243, #20217, #17864, #4489, #36644, #7466, #36859, #7676, #30447, #11067, #1710, #23625, #11273 ),
 ( #34082, #24051, #17448, #27469, #24256, #20426, #871, #10851, #14665, #33453, #10644, #4909, #13843, #4072, #1078, #37264, #4281, #7257, #37066, #17245, #23838, #1292, #30864, #27051, #27669, #11472, #26841, #14457, #20846, #7884, #8083, #33871, #39849, #17032, #4701 ),
 ( #30238, #17655, #21056, #40058, #20635, #33665, #30030, #14249, #27257, #30656, #1501, #15084, #15511, #8505, #25103, #34290, #37683, #18698, #21463, #38106, #22097, #21887, #28717, #9138, #5746, #15714, #1913, #5324, #31073, #31278, #34916, #35125, #31492, #34493, #5529 ),
 ( #41728, #8922, #18486, #5119, #12113, #2122, #31709, #21676, #2550, #18277, #28085, #5951, #40886, #2337, #15296, #41096, #24892, #8290, #28513, #34700, #14875, #41520, #24461, #28302, #18911, #11903, #37889, #37466, #41308, #38319, #8714, #12326, #21260, #18072, #25314 ),
 ( #31922, #2758, #27877, #11688, #24674, #29348, #2958, #41938, #32763, #6775, #12736, #25726, #22303, #35540, #9339, #3596, #36177, #6566, #9755, #38733, #3376, #22722, #10171, #32334, #12533, #16559, #16772, #16343, #35327, #38523, #6996, #35750, #9540, #22511, #12943 ),
 ( #6359, #23139, #404, #25934, #38943, #19329, #19965, #189, #19536, #29569, #13373, #3165, #19121, #29129, #32983, #16126, #28920, #3808, #32127, #6154, #42149, #26360, #32543, #25523, #13162, #26152, #39154, #9960, #29776, #22931, #15922, #35962, #19743, #39368, #27206 ),
 ( #23358, #21008, #40220, #27414, #36393, #7209, #33820, #11016, #20169, #4230, #4648, #17813, #17605, #10386, #23995, #11220, #16978, #33611, #40010, #7414, #33397, #1031, #4022, #33193, #17191, #29977, #10803, #817, #13995, #39801, #40426, #30607, #27000, #23785, #10593 ),
 ( #4857, #37015, #34031, #23573, #36806, #26573, #17400, #4442, #614, #13792, #7624, #1447, #24204, #37216, #8035, #14407, #26790, #36595, #30395, #13585, #39581, #20374, #7832, #30189, #14200, #20583, #1244, #20795, #1863, #11426, #9088, #15250, #15464, #24413, #37419 ),
 ( #34651, #34865, #8456, #14825, #18226, #28466, #37838, #27829, #11855, #12064, #21415, #21836, #40836, #31445, #40629, #11638, #25050, #24624, #2287, #41471, #28251, #35083, #12278, #38055, #22055, #8238, #37631, #21210, #34441, #41256, #34236, #5276, #8873, #30811, #5068 ),
 ( #31228, #2071, #25268, #5696, #18656, #31661, #18438, #18021, #5904, #1659, #2500, #38272, #14614, #27618, #31019, #15036, #28037, #41045, #24842, #8664, #21624, #5478, #32294, #39323, #41683, #25891, #2712, #19705, #25485, #19495, #12696, #38481, #39112, #3335, #35711 ),
 ( #10129, #16304, #3556, #12490, #9299, #9917, #29305, #22261, #22465, #22887, #36134, #35925, #23102, #41897, #6735, #32722, #18866, #31871, #32506, #42108, #28672, #6520, #25687, #149, #16083, #13116, #15878, #9500, #361, #35285, #38899, #9711, #35494, #19288, #15666 ),
 ( #6112, #28885, #26107, #19075, #32080, #2917, #38692, #6315, #3123, #16515, #29521, #13327, #26315, #29089, #12903, #22676, #6952, #23950, #20751, #32935, #1399, #27367, #3765, #40171, #19920, #33353, #4182, #10553, #13543, #20326, #40378, #29727, #13953, #16724, #7789 ),
 ( #7164, #39963, #17146, #4602, #26746, #569, #10963, #11173, #10755, #26533, #39537, #30560, #30148, #20123, #33148, #7368, #987, #26951, #23737, #14355, #36350, #36968, #27157, #30345, #33775, #24158, #17357, #10343, #3976, #36757, #23314, #7576, #20537, #16937, #29936 ),
 ( #774, #13751, #17559, #39756, #23521, #33567, #36549, #4400, #1194, #14154, #14776, #28415, #12227, #34601, #21575, #8611, #24789, #14567, #37167, #7988, #12010, #8826, #20958, #31611, #15410, #33980, #28201, #4809, #21363, #34390, #40787, #1610, #8403, #41420, #17760 ),
 ( #38004, #27573, #37786, #30973, #30760, #18386, #5647, #11378, #27987, #5224, #1813, #27776, #37576, #40581, #24365, #11587, #37371, #18178, #8189, #31180, #34189, #34812, #25003, #2021, #14985, #5015, #18605, #11800, #40995, #41208, #21786, #21158, #17974, #24570, #2450 ),
 ( #5430, #31394, #2239, #15198, #6681, #22832, #29245, #18811, #5855, #29034, #3497, #90, #2658, #35656, #9861, #38845, #6061, #35868, #22003, #38433, #31820, #16456, #9654, #19647, #15616, #28621, #16242, #6469, #41632, #28835, #13055, #301, #26046, #29462, #19021 ),
 ( #25218, #38221, #22622, #6264, #35035, #12850, #32028, #19444, #22413, #32449, #22205, #15827, #32662, #12440, #3076, #16035, #41848, #25632, #9038, #3281, #35440, #25433, #25836, #9249, #19235, #35236, #12645, #38642, #2866, #42055, #39056, #32245, #9447, #930, #4548 ),
 ( #39480, #33090, #23255, #26686, #10907, #10700, #39907, #26893, #13903, #32877, #30504, #13273, #30294, #27103, #39267, #7732, #33722, #10073, #4343, #26258, #39696, #10496, #16882, #19861, #23466, #17506, #36076, #20272, #23045, #14104, #3708, #23680, #7109, #6893, #36700 ),
 ( #16667, #17304, #29674, #17089, #516, #13489, #36914, #36493, #26476, #10284, #13696, #7312, #33301, #30091, #20699, #36289, #1138, #33509, #7521, #40115, #20068, #20483, #3920, #29883, #4129, #721, #23897, #34347, #34763, #37118, #24519, #31343, #41156, #24955, #11962 ),
 ( #31135, #17711, #30928, #37525, #37955, #21112, #5596, #18552, #20908, #21527, #27938, #18131, #34558, #1973, #33929, #8779, #40945, #2188, #14727, #1560, #5177, #5383, #34137, #14518, #1766, #28150, #8349, #27529, #21319, #24739, #4963, #18340, #40535, #14936, #11122 ),
 ( #11751, #40736, #37742, #11331, #17923, #21739, #30710, #8565, #15146, #27728, #11537, #27314, #1346, #14302, #4760, #24110, #40328, #24316, #7938, #37323, #8139, #28576, #29779, #19968, #31980, #3378, #41584, #617, #6777, #191, #23142, #32985, #2612, #38172, #6011 ) ),
 .UNSPECIFIED., .T., .F., .F.,
 ( 4, 2, 2, 2, 1, 2, 2, 2, 2, 2, 2, 1, 2, 2, 4 ),
 ( 4, 1, 1, 1, 1, 1, 1, 1, 1, 1, 1, 1, 1, 1, 1, 1, 1, 1, 1, 1, 1, 1, 1, 1, 1, 1, 1, 1, 1, 1, 1, 1, 4 ),
 ( 0.000000000000000000, 0.06249999999999900080, 0.1249999999999978906, 0.2499999999999956701, 0.2812499999999951150, 0.3749999999999934497, 0.4374999999999933387, 0.5000000000000000000, 0.5624999999999930056, 0.6249999999999928946, 0.7500000000000000000, 0.7812499999999951150, 0.8749999999999963363, 0.9374999999999982236, 1.000000000000000000 ),
 ( 0.000000000000000000, 0.02711375962671787321, 0.05385523109991235263, 0.08027126036152537614, 0.1064096946071439176, 0.1323192412471900226, 0.1580495177521483718, 0.1882118685537063907, 0.2182788543618764954, 0.2483346178351386324, 0.2784631806910429774, 0.3054937156393619513, 0.3327069032348308197, 0.3601597580799023035, 0.3879077415152338837, 0.4160045136367338525, 0.4445017332217630623, 0.4734489055539064517, 0.5028932750457014711, 0.5328797594123376724, 0.5634509204570880003, 0.5946469669818265080, 0.6265057848166851739, 0.6590629893014032792, 0.6923519956652609553, 0.7264041031822485728, 0.7612485893105871426, 0.7986318966073006065, 0.8369441774603861850, 0.8762126957585177900, 0.9164627945539034481, 0.9577180065289634392, 1.000000000000000000 ),
 .UNSPECIFIED. ) ;
#10971 = CARTESIAN_POINT ( 'NONE',  ( 12.41677917861187375, 153.6617311634574037, 2.127417120026097397 ) ) ;
#10972 = DIRECTION ( 'NONE',  ( 0.8745520943968235761, -0.4849315768086558398, 4.268512490100410909E-16 ) ) ;
#10973 = AXIS2_PLACEMENT_3D ( 'NONE', #37640, #24419, #25059 ) ;
#10974 = CARTESIAN_POINT ( 'NONE',  ( 22.66375647020915807, 150.6386093215955100, 0.4528757910175261192 ) ) ;
#10975 = CARTESIAN_POINT ( 'NONE',  ( 2.430217625452450569, 5.689826410578260329, 8.062849060857743666 ) ) ;
#10976 = CARTESIAN_POINT ( 'NONE',  ( 7.609804580617480774, 122.3831840716419066, 0.4262428003126361165 ) ) ;
#10977 = EDGE_CURVE ( 'NONE', #15736, #32767, #5265, .T. ) ;
#10978 = CARTESIAN_POINT ( 'NONE',  ( 21.97872426622815922, 150.5960492154097778, -0.7309654607748478083 ) ) ;
#10979 = CARTESIAN_POINT ( 'NONE',  ( 5.334825861721729012, 105.1224662015457483, 0.01195819060410700969 ) ) ;
#10980 = TOROIDAL_SURFACE ( 'NONE', #36849, 0.7620000000000000107, 0.2540000000000000036 ) ;
#10981 = CARTESIAN_POINT ( 'NONE',  ( -0.03523692298783126509, 115.6909491485452719, 1.763399716047879817 ) ) ;
#10982 = CARTESIAN_POINT ( 'NONE',  ( -57.65203525413342334, 1.118929822212927361, 0.5921937322712250706 ) ) ;
#10983 = CARTESIAN_POINT ( 'NONE',  ( -15.19006826215924555, 156.0999766016731769, -0.2361313609475708120 ) ) ;
#10984 = ORIENTED_EDGE ( 'NONE', *, *, #5353, .F. ) ;
#10985 = EDGE_CURVE ( 'NONE', #31926, #588, #3220, .T. ) ;
#10986 = CARTESIAN_POINT ( 'NONE',  ( -47.01877684503696742, 24.36789988528162354, -2.430126310640470688 ) ) ;
#10987 = CARTESIAN_POINT ( 'NONE',  ( -6.843608447964458996, 121.5419263055753731, -0.7453496101816521335 ) ) ;
#10988 = CARTESIAN_POINT ( 'NONE',  ( -47.10086694478710712, 25.28009754960136490, -1.863548351662550617 ) ) ;
#10989 = ORIENTED_EDGE ( 'NONE', *, *, #28206, .F. ) ;
#10990 = CARTESIAN_POINT ( 'NONE',  ( 1.044095825906500297, 115.6909491485452719, -1.710621833244764245 ) ) ;
#10991 = CARTESIAN_POINT ( 'NONE',  ( -15.83762317627089189, 145.9541952667573810, -0.7712195890315685087 ) ) ;
#10992 = CARTESIAN_POINT ( 'NONE',  ( 2.370890509137566937, -15.02769382788871155, 5.804473790077508077 ) ) ;
#10993 = CIRCLE ( 'NONE', #140, 2.857500000000000817 ) ;
#10994 = CARTESIAN_POINT ( 'NONE',  ( -0.01887972822151516225, 159.3676309965788960, 0.9448188026860502298 ) ) ;
#10995 = CARTESIAN_POINT ( 'NONE',  ( -7.783246152616193569, 154.6561476914895081, -0.1555277812256514736 ) ) ;
#10996 = AXIS2_PLACEMENT_3D ( 'NONE', #21228, #31041, #8256 ) ;
#10997 = CARTESIAN_POINT ( 'NONE',  ( 22.98214253804986384, 150.1595482613961110, 0.5361612621683795599 ) ) ;
#10998 = ORIENTED_EDGE ( 'NONE', *, *, #25402, .T. ) ;
#10999 = CARTESIAN_POINT ( 'NONE',  ( -4.476207883417873568, -7.053342675672244155, -1.178223045331058705 ) ) ;
#11000 = EDGE_CURVE ( 'NONE', #39424, #18094, #3809, .T. ) ;
#11001 = CARTESIAN_POINT ( 'NONE',  ( -10.83330528665015891, 157.8980211815716928, -0.2164752214609687586 ) ) ;
#11002 = AXIS2_PLACEMENT_3D ( 'NONE', #40725, #24506, #21512 ) ;
#11003 = CARTESIAN_POINT ( 'NONE',  ( 13.51778232847667205, 17.08230797367789222, 5.016499999999999737 ) ) ;
#11004 = DIRECTION ( 'NONE',  ( -5.188838149069471174E-16, 1.699382548006136313E-16, 1.000000000000000000 ) ) ;
#11005 = VERTEX_POINT ( 'NONE', #22062 ) ;
#11006 = CARTESIAN_POINT ( 'NONE',  ( 6.352347778906425546, 119.4701337457096031, 1.260299788626464190 ) ) ;
#11007 = CARTESIAN_POINT ( 'NONE',  ( -2.734508853367146219, 0.3528594962865297391, 3.724956791467788353 ) ) ;
#11008 = CARTESIAN_POINT ( 'NONE',  ( 17.34281104028693576, 125.1846915036903027, 1.498326104650645973 ) ) ;
#11009 = CARTESIAN_POINT ( 'NONE',  ( -48.44329217233745055, 18.62907245612683838, -5.187175938578627132 ) ) ;
#11010 = CARTESIAN_POINT ( 'NONE',  ( 12.66950698665810648, 121.4495935343099688, -1.177842983441547808 ) ) ;
#11011 = CARTESIAN_POINT ( 'NONE',  ( -3.029891238501105644, -9.367638731076009861, 3.490193963561483148 ) ) ;
#11012 = CARTESIAN_POINT ( 'NONE',  ( -4.857111322523853580, 117.4312795728108227, -0.7492135168955066371 ) ) ;
#11013 = EDGE_CURVE ( 'NONE', #19376, #449, #4091, .T. ) ;
#11014 = ORIENTED_EDGE ( 'NONE', *, *, #198, .F. ) ;
#11015 = CARTESIAN_POINT ( 'NONE',  ( -2.930943089244575805, 156.0861408873597327, 0.1605890987591811481 ) ) ;
#11016 = CARTESIAN_POINT ( 'NONE',  ( 3.233725904218312408, -15.30436843596319463, 5.598328752637605099 ) ) ;
#11017 = CARTESIAN_POINT ( 'NONE',  ( -47.84356795211458291, 19.38525671449504983, 5.197506975155153697 ) ) ;
#11018 = CARTESIAN_POINT ( 'NONE',  ( -0.1816203019703736821, 118.1651005609832907, -0.8950686016172918480 ) ) ;
#11019 = ORIENTED_EDGE ( 'NONE', *, *, #6783, .T. ) ;
#11020 = CARTESIAN_POINT ( 'NONE',  ( 15.41952259888541121, 128.5596447653542498, 2.179146846741408350 ) ) ;
#11021 = LINE ( 'NONE', #27005, #14740 ) ;
#11022 = DIRECTION ( 'NONE',  ( -0.01997839162482761832, -1.040247600000950455E-18, 0.9998004120163610509 ) ) ;
#11023 = AXIS2_PLACEMENT_3D ( 'NONE', #2208, #12616, #8799 ) ;
#11024 = CARTESIAN_POINT ( 'NONE',  ( -22.27457866854819812, 149.8733841865972920, 0.8555749715664362487 ) ) ;
#11025 = CARTESIAN_POINT ( 'NONE',  ( 8.137580693842743074, 4.222088520697473868, -2.276242723817686997 ) ) ;
#11026 = CARTESIAN_POINT ( 'NONE',  ( 16.08743688339769662, 147.0533492130506943, 1.289446542218032787 ) ) ;
#11027 = DIRECTION ( 'NONE',  ( -9.627370216492862708E-17, -1.000000000000000000, 0.000000000000000000 ) ) ;
#11028 = EDGE_CURVE ( 'NONE', #16499, #18999, #39546, .T. ) ;
#11029 = CARTESIAN_POINT ( 'NONE',  ( 13.24393851483415752, 156.9672759736256467, -0.3459722171078643549 ) ) ;
#11030 = DIRECTION ( 'NONE',  ( 5.188838149069472160E-16, -1.699382548006136559E-16, -1.000000000000000000 ) ) ;
#11031 = CARTESIAN_POINT ( 'NONE',  ( -54.64736747358799818, 7.536306771770948210, 3.171698711319464792 ) ) ;
#11032 = CARTESIAN_POINT ( 'NONE',  ( -29.79391970787719757, 57.88946435418900194, -1.524000000000005128 ) ) ;
#11033 = CARTESIAN_POINT ( 'NONE',  ( -57.93941708942283952, 2.052042089854988483, 1.628789306319508245 ) ) ;
#11034 = CARTESIAN_POINT ( 'NONE',  ( -57.69320192990073082, 1.722488987974756025, 1.652538576205534460 ) ) ;
#11035 = CARTESIAN_POINT ( 'NONE',  ( -4.364241878784717699, 118.1821976670573804, 0.4477677367896528149 ) ) ;
#11036 = CARTESIAN_POINT ( 'NONE',  ( 3.182978606911899266, 107.7309519196391534, -4.270837756928458795 ) ) ;
#11037 = EDGE_LOOP ( 'NONE', ( #35481, #22247, #19582, #32473 ) ) ;
#11038 = CARTESIAN_POINT ( 'NONE',  ( -44.55074271434504851, 21.27721161058206789, 3.389857510897057224 ) ) ;
#11039 = CARTESIAN_POINT ( 'NONE',  ( 3.881581157509474078, 119.0007618588171852, -0.7751610500674797066 ) ) ;
#11040 = CARTESIAN_POINT ( 'NONE',  ( -7.694663930960380149, 124.9344662015457317, -0.1537576976229973191 ) ) ;
#11041 = CARTESIAN_POINT ( 'NONE',  ( 4.160719191527030958, 118.2392048939543798, 0.3834139420345348825 ) ) ;
#11042 = CARTESIAN_POINT ( 'NONE',  ( -10.97991518849998549, 126.1652090859982707, -0.9941924553172258872 ) ) ;
#11043 = SURFACE_STYLE_FILL_AREA ( #4469 ) ;
#11044 = CARTESIAN_POINT ( 'NONE',  ( 1.049180143938831522, 117.3993836601177065, -1.438948719551953248 ) ) ;
#11045 = ORIENTED_EDGE ( 'NONE', *, *, #40493, .F. ) ;
#11046 = CARTESIAN_POINT ( 'NONE',  ( 4.060783872423706420, 109.8065891650451249, -3.521960838153598505 ) ) ;
#11047 = CARTESIAN_POINT ( 'NONE',  ( -9.904299505090595090, 154.0333045108203009, -1.503511620041811714 ) ) ;
#11048 = CARTESIAN_POINT ( 'NONE',  ( -5.302405987100971885, 104.6144662015457101, 1.270606870302479541 ) ) ;
#11049 = CARTESIAN_POINT ( 'NONE',  ( -45.65533061069353238, 20.86966646997320396, 4.138311239626682791 ) ) ;
#11050 = CARTESIAN_POINT ( 'NONE',  ( 12.21488373879589240, 55.24500000000000455, 5.016499999999999737 ) ) ;
#11051 = CARTESIAN_POINT ( 'NONE',  ( -8.682609107657992098, 123.6667050411435582, -0.04289417010140435943 ) ) ;
#11052 = EDGE_CURVE ( 'NONE', #30132, #30491, #37901, .T. ) ;
#11053 = LINE ( 'NONE', #13830, #34757 ) ;
#11054 = CARTESIAN_POINT ( 'NONE',  ( 14.30760545269993500, 120.4308286971427862, 0.9551244717093423375 ) ) ;
#11055 = LINE ( 'NONE', #4688, #40280 ) ;
#11056 = CARTESIAN_POINT ( 'NONE',  ( 3.248418650160624033, -14.57852055173261618, 2.075358651653527620 ) ) ;
#11057 = CARTESIAN_POINT ( 'NONE',  ( -0.5101717508068956963, 119.1670848682014281, 0.5756831679880034525 ) ) ;
#11058 = CARTESIAN_POINT ( 'NONE',  ( 0.9729305924359374913, -6.768038221194544235, 0.04477287409810011554 ) ) ;
#11059 = CARTESIAN_POINT ( 'NONE',  ( -15.39807837497279408, 121.0727120035890323, -0.9152850519163394649 ) ) ;
#11060 = VECTOR ( 'NONE', #10571, 1000.000000000000000 ) ;
#11061 = EDGE_CURVE ( 'NONE', #29150, #4283, #39964, .T. ) ;
#11062 = CARTESIAN_POINT ( 'NONE',  ( 0.8997923272943838535, 13.09534505249760805, -0.3740510727227569499 ) ) ;
#11063 = B_SPLINE_CURVE_WITH_KNOTS ( 'NONE', 3,
 ( #37877, #40873, #18058, #41083, #35113, #5106, #28706, #41296, #34480, #5940, #25301, #21663, #31061, #12521, #28498, #38304, #31479, #41508, #9125, #8493, #14862, #25089, #38094, #37453, #27865, #2324, #18899, #31909, #2745, #5312, #15284, #24880, #11674, #8909, #21247, #12313, #11891, #18263, #34687, #31696, #31266, #18686, #2538, #34277, #24661, #37670, #15072, #28072, #19527, #29766, #9329, #29338, #29558, #3153, #38723, #19732, #3587, #602, #16117, #39144, #180, #22712, #29120, #6552, #35317, #13149, #32324, #25924, #35529, #38933, #26142, #42139, #6984, #41926, #3366, #32753, #25512, #35740, #32117, #9531, #12934, #26349, #2947, #25716, #22500, #6350, #9743, #19320, #32534, #23129, #16333, #9948, #22921, #38512, #35952, #6765, #16548, #12727, #22292, #15911, #28911, #393, #13360, #39355, #10159, #36166, #19954, #6144, #32972, #3797, #16759, #19109, #33810, #8026, #10792, #17181, #36795, #23346, #1234, #20364, #13986, #10584, #26990, #11007, #17803, #40415, #37005, #23774, #30800, #20158, #39790, #23562, #23986, #24195, #14397, #33183, #13783, #36584, #7402, #33386, #4220, #11211, #30180, #40209, #1021, #13576, #40001, #37205, #7613, #20575, #27405, #39571, #20997, #34022, #33601, #4011, #4847, #26564, #4434, #17392, #16968, #36384, #30383, #4638, #10377, #7824, #14191, #27196, #26779, #20786, #17595, #30599, #1437, #7200, #29967, #807, #5468, #40618, #27609, #25257, #11843, #41461, #11417, #35073, #34640, #40826, #12268, #31651, #2060, #24403, #22044, #21826, #2491, #24830, #34855 ),
 .UNSPECIFIED., .F., .F.,
 ( 4, 1, 1, 1, 1, 1, 1, 1, 1, 1, 1, 1, 1, 1, 1, 1, 1, 1, 1, 1, 1, 1, 1, 1, 1, 1, 1, 1, 1, 1, 1, 1, 1, 1, 1, 1, 1, 1, 1, 1, 1, 1, 1, 1, 1, 1, 1, 1, 1, 1, 1, 1, 1, 1, 1, 1, 1, 1, 1, 1, 1, 1, 1, 1, 1, 1, 1, 1, 1, 1, 1, 1, 1, 1, 1, 1, 1, 1, 1, 1, 1, 1, 1, 1, 1, 1, 1, 1, 1, 1, 1, 1, 1, 1, 1, 1, 1, 1, 1, 1, 1, 1, 1, 1, 1, 1, 1, 1, 1, 1, 1, 1, 1, 1, 1, 1, 1, 1, 1, 1, 1, 1, 1, 1, 1, 1, 1, 1, 1, 1, 1, 1, 1, 1, 1, 1, 1, 1, 1, 1, 1, 1, 1, 1, 1, 1, 1, 1, 1, 1, 1, 1, 1, 1, 1, 1, 1, 1, 1, 1, 1, 1, 1, 1, 1, 1, 1, 1, 1, 1, 1, 1, 1, 1, 1, 1, 1, 1, 1, 1, 1, 1, 1, 1, 1, 1, 1, 1, 1, 1, 1, 1, 4 ),
 ( 0.000000000000000000, 0.007812500000000423273, 0.01388888888888889506, 0.01562500000000000000, 0.02343749999999998959, 0.02777777777777778317, 0.03125000000000092981, 0.03906249999999999306, 0.04166666666666667823, 0.04687500000000000000, 0.05468749999999999306, 0.05555555555555556635, 0.06249999999999997918, 0.06944444444444446141, 0.07031250000000000000, 0.07812500000000000000, 0.08333333333333334259, 0.08593749999999998612, 0.09374999999999603095, 0.09722222222222223764, 0.1015625000000000139, 0.1093750000000000000, 0.1111111111111111188, 0.1171875000000000000, 0.1250000000000000000, 0.1328125000000000000, 0.1388888888888889228, 0.1406250000000000000, 0.1484375000000000000, 0.1527777777777778179, 0.1562500000000039690, 0.1640625000000000000, 0.1666666666666666852, 0.1718750000000000000, 0.1796875000000000000, 0.1805555555555555802, 0.1875000000000000000, 0.1944444444444444753, 0.1953125000000000000, 0.2031250000000000000, 0.2083333333333333703, 0.2109375000000000000, 0.2187499999999960310, 0.2222222222222222376, 0.2265625000000000000, 0.2343750000000000000, 0.2361111111111111327, 0.2421875000000000000, 0.2500000000000000000, 0.2578125000000000000, 0.2638888888888888951, 0.2656250000000000000, 0.2734375000000000000, 0.2777777777777777346, 0.2812500000000039968, 0.2890625000000000000, 0.2916666666666665741, 0.2968750000000000000, 0.3046875000000000000, 0.3055555555555554692, 0.3125000000000000000, 0.3194444444444443088, 0.3203125000000000000, 0.3281250000000000000, 0.3333333333333332038, 0.3359375000000000000, 0.3437499999999960587, 0.3472222222222220434, 0.3515625000000000000, 0.3593750000000000000, 0.3611111111111109384, 0.3671875000000000000, 0.3750000000000000000, 0.3828125000000000000, 0.3888888888888886175, 0.3906250000000000000, 0.3984375000000000000, 0.4027777777777775126, 0.4062500000000039968, 0.4140625000000000000, 0.4166666666666663521, 0.4218750000000000000, 0.4296875000000000000, 0.4305555555555552472, 0.4375000000000000000, 0.4444444444444440867, 0.4453125000000000000, 0.4531250000000000000, 0.4583333333333329818, 0.4609375000000000000, 0.4687499999999960587, 0.4722222222222218768, 0.4765625000000000000, 0.4843750000000000000, 0.4861111111111107719, 0.4921875000000000000, 0.5000000000000000000, 0.5078125000000000000, 0.5138888888888886175, 0.5156250000000000000, 0.5234375000000000000, 0.5277777777777775681, 0.5312500000000039968, 0.5390625000000000000, 0.5416666666666664076, 0.5468750000000000000, 0.5546875000000000000, 0.5555555555555553582, 0.5625000000000000000, 0.5694444444444443088, 0.5703125000000000000, 0.5781250000000000000, 0.5833333333333331483, 0.5859375000000000000, 0.5937499999999960032, 0.5972222222222220989, 0.6015625000000000000, 0.6093750000000000000, 0.6111111111111110494, 0.6171875000000000000, 0.6250000000000000000, 0.6328125000000000000, 0.6388888888888888395, 0.6406250000000000000, 0.6484375000000000000, 0.6527777777777777901, 0.6562500000000039968, 0.6640625000000000000, 0.6666666666666666297, 0.6718750000000000000, 0.6796875000000000000, 0.6805555555555555802, 0.6875000000000000000, 0.6944444444444445308, 0.6953125000000000000, 0.7031250000000000000, 0.7083333333333333703, 0.7109375000000000000, 0.7187499999999960032, 0.7222222222222223209, 0.7265625000000000000, 0.7343750000000000000, 0.7361111111111111605, 0.7421875000000000000, 0.7500000000000000000, 0.7578125000000000000, 0.7638888888888889506, 0.7656250000000000000, 0.7734375000000000000, 0.7777777777777779011, 0.7812500000000039968, 0.7890625000000000000, 0.7916666666666668517, 0.7968750000000000000, 0.8046875000000000000, 0.8055555555555556912, 0.8125000000000000000, 0.8194444444444446418, 0.8203125000000000000, 0.8281250000000000000, 0.8333333333333335924, 0.8359375000000000000, 0.8437499999999960032, 0.8472222222222224319, 0.8515625000000000000, 0.8593750000000000000, 0.8611111111111113825, 0.8671875000000000000, 0.8750000000000000000, 0.8828125000000000000, 0.8888888888888891726, 0.8906250000000000000, 0.8984375000000000000, 0.9027777777777781232, 0.9062500000000039968, 0.9140625000000000000, 0.9166666666666670737, 0.9218750000000000000, 0.9296875000000000000, 0.9305555555555559133, 0.9375000000000000000, 0.9444444444444447528, 0.9453125000000000000, 0.9531250000000000000, 0.9583333333333335924, 0.9609375000000000000, 0.9687499999999991118, 0.9722222222222224319, 0.9765625000000000000, 0.9843750000000000000, 0.9861111111111111605, 0.9921874999999995559, 1.000000000000000000 ),
 .UNSPECIFIED. ) ;
#11064 = VERTEX_POINT ( 'NONE', #7172 ) ;
#11065 = CARTESIAN_POINT ( 'NONE',  ( -49.09053848811835508, 14.44377425990215436, 0.7907028275641450055 ) ) ;
#11066 = CARTESIAN_POINT ( 'NONE',  ( -9.279111390949827509, 123.6186430441458981, 0.4039598099628549654 ) ) ;
#11067 = CARTESIAN_POINT ( 'NONE',  ( 4.668376822648329316, -11.99306229768662391, 1.198378876927704839 ) ) ;
#11068 = CARTESIAN_POINT ( 'NONE',  ( 0.8674473734592740293, 156.8926940187749324, -1.309446568524254451 ) ) ;
#11069 = VERTEX_POINT ( 'NONE', #13959 ) ;
#11070 = CARTESIAN_POINT ( 'NONE',  ( -4.138103288469840102, 104.6144662015457669, 2.504989205037290834 ) ) ;
#11071 = CARTESIAN_POINT ( 'NONE',  ( 2.976679874252225577, -13.20894259333504905, 0.9412263588231246647 ) ) ;
#11072 = CARTESIAN_POINT ( 'NONE',  ( -4.884145585883596041, 117.6381453523385687, -1.023340015079030163 ) ) ;
#11073 = CARTESIAN_POINT ( 'NONE',  ( 15.64855408859525099, 147.2205073051419504, 0.1844942485914530250 ) ) ;
#11074 = CIRCLE ( 'NONE', #24642, 6.350000000000004974 ) ;
#11075 = EDGE_LOOP ( 'NONE', ( #12438, #3792, #18892, #31958 ) ) ;
#11076 = CARTESIAN_POINT ( 'NONE',  ( 12.86454329319598067, 121.9120276846612256, 1.753115191834736963 ) ) ;
#11077 = CARTESIAN_POINT ( 'NONE',  ( -5.871452009091383317, 57.14999999999999147, 5.016499999999999737 ) ) ;
#11078 = CARTESIAN_POINT ( 'NONE',  ( 0.3704050251096834834, 117.3993836136686326, 1.500861956288976007 ) ) ;
#11079 = CARTESIAN_POINT ( 'NONE',  ( 0.006534887713546001439, 159.5822087645323393, -0.3270325034788579277 ) ) ;
#11080 = CARTESIAN_POINT ( 'NONE',  ( 1.843513859164539248, 116.5452236745340429, -0.1029321673164912687 ) ) ;
#11081 = DIRECTION ( 'NONE',  ( -5.188838149069471174E-16, 1.699382548006136313E-16, 1.000000000000000000 ) ) ;
#11082 = AXIS2_PLACEMENT_3D ( 'NONE', #26401, #32375, #29389 ) ;
#11083 = CARTESIAN_POINT ( 'NONE',  ( 2.002795586526139093, -15.67918376216764820, 5.544594217737087938 ) ) ;
#11084 = CARTESIAN_POINT ( 'NONE',  ( -11.05715273818225164, 82.67346420587206524, -1.269999999999999352 ) ) ;
#11085 = CARTESIAN_POINT ( 'NONE',  ( -3.406197898068538787, 31.16742545776281403, -0.5635140647784588896 ) ) ;
#11086 = CARTESIAN_POINT ( 'NONE',  ( 15.63125989577329733, 125.4375369430449609, 1.961567602338091243 ) ) ;
#11087 = EDGE_LOOP ( 'NONE', ( #32434, #28676, #17887, #386 ) ) ;
#11088 = CARTESIAN_POINT ( 'NONE',  ( -8.431077252155047219, 22.10977948022283357, 0.3997009428958171462 ) ) ;
#11089 = CARTESIAN_POINT ( 'NONE',  ( 5.572310759512880907, 117.9647318291645348, -0.8674352534993811092 ) ) ;
#11090 = CARTESIAN_POINT ( 'NONE',  ( -3.552294876605587515, 120.2162445758188056, -0.4839898749706282310 ) ) ;
#11091 = CARTESIAN_POINT ( 'NONE',  ( -5.885917553499150578, 77.12042444889114279, -1.523999999999996025 ) ) ;
#11092 = CARTESIAN_POINT ( 'NONE',  ( -0.02537255736359465483, 39.20946620154573736, 1.269746523260778082 ) ) ;
#11093 = CARTESIAN_POINT ( 'NONE',  ( -4.138103289099216653, 104.6144662015456959, 2.504989205464778212 ) ) ;
#11094 = AXIS2_PLACEMENT_3D ( 'NONE', #23371, #11030, #39813 ) ;
#11095 = CARTESIAN_POINT ( 'NONE',  ( 3.700881553190929374, 8.714383148187751615, -2.768892949411812854 ) ) ;
#11096 = CYLINDRICAL_SURFACE ( 'NONE', #6113, 0.2539999999999998925 ) ;
#11097 = CARTESIAN_POINT ( 'NONE',  ( -4.831981401426255651, 118.5264896598256854, 0.7492988386145865709 ) ) ;
#11098 = CARTESIAN_POINT ( 'NONE',  ( 3.154356104639033820, -12.65568165217861818, 0.8785170097314246584 ) ) ;
#11099 = CARTESIAN_POINT ( 'NONE',  ( 4.469499996959894972, 123.9529229959338608, 0.04273414237147030864 ) ) ;
#11100 = CARTESIAN_POINT ( 'NONE',  ( -2.690315046239569519, 30.48488075981191159, 3.827843980145978264 ) ) ;
#11101 = CARTESIAN_POINT ( 'NONE',  ( -25.77058783747419213, 72.83664265955201245, -1.524000000000005572 ) ) ;
#11102 = ORIENTED_EDGE ( 'NONE', *, *, #34542, .F. ) ;
#11103 = CARTESIAN_POINT ( 'NONE',  ( -2.611728715877724039, 105.1243698582466095, -4.651900295541603114 ) ) ;
#11104 = CARTESIAN_POINT ( 'NONE',  ( 5.059117473032719303, -15.50674158137822722, 2.046454293345789655 ) ) ;
#11105 = CARTESIAN_POINT ( 'NONE',  ( -8.792330854012698538, 120.0394951565550343, 1.134075770671235217 ) ) ;
#11106 = EDGE_CURVE ( 'NONE', #39412, #41136, #23320, .T. ) ;
#11107 = CARTESIAN_POINT ( 'NONE',  ( 0.5714185265493636479, 16.70905722793067838, 0.7929698740637279863 ) ) ;
#11108 = ORIENTED_EDGE ( 'NONE', *, *, #36604, .T. ) ;
#11109 = ORIENTED_EDGE ( 'NONE', *, *, #8932, .T. ) ;
#11110 = LINE ( 'NONE', #4328, #38123 ) ;
#11111 = CARTESIAN_POINT ( 'NONE',  ( 2.562387952376848688, 120.6526784328644339, 0.4448203013800775540 ) ) ;
#11112 = CARTESIAN_POINT ( 'NONE',  ( -10.37991283549673227, 123.8962982355681817, 0.8252603836154488448 ) ) ;
#11113 = CARTESIAN_POINT ( 'NONE',  ( -41.80860202649011370, 22.71167205159044045, 1.570694036847530173 ) ) ;
#11114 = CARTESIAN_POINT ( 'NONE',  ( 11.64488154209785087, 123.4149316504530702, -1.218180013452823562 ) ) ;
#11115 = STYLED_ITEM ( 'NONE', ( #9167 ), #24724 ) ;
#11116 = CARTESIAN_POINT ( 'NONE',  ( -14.40940766795072037, 123.3930721568691382, -1.837956572252895882 ) ) ;
#11117 = DIRECTION ( 'NONE',  ( -5.206863593109713661E-17, 1.000000000000000000, -1.077750396879097183E-30 ) ) ;
#11118 = CARTESIAN_POINT ( 'NONE',  ( 4.414058189832408274, 118.1799051844840704, -0.3934113130358646848 ) ) ;
#11119 = CIRCLE ( 'NONE', #26788, 0.7620000000000015650 ) ;
#11120 = CARTESIAN_POINT ( 'NONE',  ( 2.986828117522162263, 156.0959049650892041, -0.3398701836618409633 ) ) ;
#11121 = VERTEX_POINT ( 'NONE', #39327 ) ;
#11122 = CARTESIAN_POINT ( 'NONE',  ( 2.669030664778226480, -13.79969672238709499, -0.04828590215123814561 ) ) ;
#11123 = CARTESIAN_POINT ( 'NONE',  ( 12.21488373878702305, 55.49440886859300548, -5.016500000000000625 ) ) ;
#11124 = AXIS2_PLACEMENT_3D ( 'NONE', #30211, #17835, #5089 ) ;
#11125 = CARTESIAN_POINT ( 'NONE',  ( -50.47813777548210368, 15.38220854283604133, 4.696510882197381775 ) ) ;
#11126 = CARTESIAN_POINT ( 'NONE',  ( -4.360315236241580017, -1.596229544307166348, -1.535301415559372940 ) ) ;
#11127 = CARTESIAN_POINT ( 'NONE',  ( 16.94372847238220103, 146.2370505443881257, 1.929411111270964874 ) ) ;
#11128 = CARTESIAN_POINT ( 'NONE',  ( 1.737819774751971025, 35.35497751095494579, 1.681281876415605225 ) ) ;
#11129 = CARTESIAN_POINT ( 'NONE',  ( -5.756868464772181504, 120.3160329940760818, 0.2053529492706008819 ) ) ;
#11130 = CARTESIAN_POINT ( 'NONE',  ( -4.603678009535974169, 12.38766144714272066, -0.4343361176327051321 ) ) ;
#11131 = CARTESIAN_POINT ( 'NONE',  ( 15.76687399610631246, 145.9134097338176730, 0.4436328104633036062 ) ) ;
#11132 = CARTESIAN_POINT ( 'NONE',  ( -11.55299880265467394, 55.57741982016696625, 4.472382752598255351 ) ) ;
#11133 = CARTESIAN_POINT ( 'NONE',  ( -55.72901529264892417, 4.991126730481368234, -1.691135755076719649 ) ) ;
#11134 = CARTESIAN_POINT ( 'NONE',  ( -5.552814959551180429, 116.7375731949262700, -0.3279940554716652135 ) ) ;
#11135 = CARTESIAN_POINT ( 'NONE',  ( 16.62722885652246418, 62.94807988814252298, 4.514343177587269551 ) ) ;
#11136 = CIRCLE ( 'NONE', #39709, 9.048749999999998295 ) ;
#11137 = FACE_OUTER_BOUND ( 'NONE', #17088, .T. ) ;
#11138 = CARTESIAN_POINT ( 'NONE',  ( -0.6542591033984136439, 106.0194232803750509, 5.259796465664852150 ) ) ;
#11139 = DIRECTION ( 'NONE',  ( 0.1906721105965065721, -0.9816537812491090698, 2.657572025465716008E-16 ) ) ;
#11140 = CARTESIAN_POINT ( 'NONE',  ( 8.383109624418931816, 7.835852165998051788, -1.087619381312709077 ) ) ;
#11141 = CARTESIAN_POINT ( 'NONE',  ( 5.332935392244917416, 115.7029491189645825, 0.1065647408284378928 ) ) ;
#11142 = DIRECTION ( 'NONE',  ( -0.8745520943968240202, 0.4849315768086551737, -5.361993529360572958E-16 ) ) ;
#11143 = CARTESIAN_POINT ( 'NONE',  ( -58.32144855246983184, 1.173557705256414341, 1.098103182355992136 ) ) ;
#11144 = CARTESIAN_POINT ( 'NONE',  ( -3.831877602099685198, 71.07198261757335445, -1.523999999999993804 ) ) ;
#11145 = CARTESIAN_POINT ( 'NONE',  ( -23.26894437362541979, 149.0206351951634076, -0.01026395906018885695 ) ) ;
#11146 = AXIS2_PLACEMENT_3D ( 'NONE', #13915, #23269, #23481 ) ;
#11147 = ORIENTED_EDGE ( 'NONE', *, *, #25126, .T. ) ;
#11148 = CARTESIAN_POINT ( 'NONE',  ( -56.26154134543016738, 7.775270144418325202, -0.1976385065555597287 ) ) ;
#11149 = EDGE_LOOP ( 'NONE', ( #27571, #19948, #9883, #18592 ) ) ;
#11150 = CARTESIAN_POINT ( 'NONE',  ( -45.11690586071466669, 21.31720619196558886, -3.746636771225956952 ) ) ;
#11151 = CARTESIAN_POINT ( 'NONE',  ( -8.981069108608934926, 123.9698733229553937, -0.1794631345465900474 ) ) ;
#11152 = CARTESIAN_POINT ( 'NONE',  ( 6.307811598796486230, -13.53853427790793695, 1.133914056348525934 ) ) ;
#11153 = CARTESIAN_POINT ( 'NONE',  ( -0.02874440110946554008, 158.8294072187990196, 1.438487372358303595 ) ) ;
#11154 = CIRCLE ( 'NONE', #30883, 0.5080000000000000071 ) ;
#11155 = CARTESIAN_POINT ( 'NONE',  ( 23.10841651933900209, 148.9583646262859133, 1.191549328111825901 ) ) ;
#11156 = CARTESIAN_POINT ( 'NONE',  ( 9.476822779618517600, 118.5748184150550060, -0.6643292918320548024 ) ) ;
#11157 = DIRECTION ( 'NONE',  ( -5.188838149069472160E-16, 1.699382548006136559E-16, 1.000000000000000000 ) ) ;
#11158 = CARTESIAN_POINT ( 'NONE',  ( -23.30750959433838432, 148.8446908248229477, -0.7975424382754975339 ) ) ;
#11159 = CARTESIAN_POINT ( 'NONE',  ( -49.26965912534817704, 17.43349283265777672, -5.070912566603587024 ) ) ;
#11160 = ORIENTED_EDGE ( 'NONE', *, *, #24839, .F. ) ;
#11161 = CARTESIAN_POINT ( 'NONE',  ( -8.796889684792216002, 117.7044376108156172, -0.02762689297412515566 ) ) ;
#11162 = CARTESIAN_POINT ( 'NONE',  ( -13.68689207195655122, 152.4534842159446271, 1.543072478675916903 ) ) ;
#11163 = CARTESIAN_POINT ( 'NONE',  ( -57.79663075882820777, 0.9446393961914554271, -1.102772590789307339 ) ) ;
#11164 = CARTESIAN_POINT ( 'NONE',  ( 12.06323264149818364, 122.4500365997666336, -1.303827596403756672 ) ) ;
#11165 = CIRCLE ( 'NONE', #7780, 0.2539999999999998925 ) ;
#11166 = CARTESIAN_POINT ( 'NONE',  ( 0.9729305924359374913, -6.768038221194544235, 0.04477287409810011554 ) ) ;
#11167 = CARTESIAN_POINT ( 'NONE',  ( 0.009931510163623535892, 117.7854482299006378, -0.4970133802592048844 ) ) ;
#11168 = CARTESIAN_POINT ( 'NONE',  ( -46.25688858429101202, 20.73875112231587892, -4.700046123029353318 ) ) ;
#11169 = CARTESIAN_POINT ( 'NONE',  ( 16.24447748055625240, 147.7868695473139553, -0.9462090312511075574 ) ) ;
#11170 = CARTESIAN_POINT ( 'NONE',  ( -15.38000172822634326, 147.8312228277220868, -0.3073290368998167210 ) ) ;
#11171 = ORIENTED_EDGE ( 'NONE', *, *, #39593, .T. ) ;
#11172 = CARTESIAN_POINT ( 'NONE',  ( -17.73882382519380840, 148.9562551477873740, -2.372964443305867643 ) ) ;
#11173 = CARTESIAN_POINT ( 'NONE',  ( 2.989574797431095554, -15.77888062423098070, 5.070590765341169259 ) ) ;
#11174 = CARTESIAN_POINT ( 'NONE',  ( 10.92199999999999704, 56.51500000000000057, 5.016499999999999737 ) ) ;
#11175 = CARTESIAN_POINT ( 'NONE',  ( -4.286648012141172082, 118.2141956653288162, -0.5113893019683410923 ) ) ;
#11176 = CARTESIAN_POINT ( 'NONE',  ( -52.26939619200407350, 13.58078015197115818, -4.476849201000089096 ) ) ;
#11177 = DIRECTION ( 'NONE',  ( -5.188838149069472160E-16, 1.699382548006136559E-16, 1.000000000000000000 ) ) ;
#11178 = CARTESIAN_POINT ( 'NONE',  ( 15.79265013067990964, 150.9007765090757971, 2.261858994468948225 ) ) ;
#11179 = CARTESIAN_POINT ( 'NONE',  ( -6.538677740023618411E-14, 75.27746620154573520, -7.356392042280733227E-18 ) ) ;
#11180 = CARTESIAN_POINT ( 'NONE',  ( 23.42514220146282966, 142.8382549601284097, 0.4680900899253090941 ) ) ;
#11181 = CARTESIAN_POINT ( 'NONE',  ( 8.429690783291841072, 7.639065531857588631, 0.01617727833786941974 ) ) ;
#11182 = CARTESIAN_POINT ( 'NONE',  ( 15.80292465353828568, 145.7390459690742830, 0.7709107363076879160 ) ) ;
#11183 = CARTESIAN_POINT ( 'NONE',  ( 21.34935411394454974, 151.2846570542378117, -0.7363345373129175364 ) ) ;
#11184 = CARTESIAN_POINT ( 'NONE',  ( -8.095114962461808616, 74.19100168833409725, -1.269999999999996687 ) ) ;
#11185 = CARTESIAN_POINT ( 'NONE',  ( -13.15921246430372804, 51.38419125632634632, 1.524000000000004018 ) ) ;
#11186 = B_SPLINE_CURVE_WITH_KNOTS ( 'NONE', 3,
 ( #3770, #29734, #20541, #40382, #14159, #23954 ),
 .UNSPECIFIED., .F., .F.,
 ( 4, 2, 4 ),
 ( 0.000000000000000000, 0.4601069123251853576, 0.9202138246503707153 ),
 .UNSPECIFIED. ) ;
#11187 = CARTESIAN_POINT ( 'NONE',  ( -58.24002838079472610, 0.001074765447070524793, 0.6562585879479658768 ) ) ;
#11188 = CARTESIAN_POINT ( 'NONE',  ( -13.43120660244762732, 156.9273374874128137, -0.2039374989780117498 ) ) ;
#11189 = VERTEX_POINT ( 'NONE', #13757 ) ;
#11190 = CARTESIAN_POINT ( 'NONE',  ( -46.60530155212503445, 26.17382724835477958, -9.383119846931408523E-15 ) ) ;
#11191 = CARTESIAN_POINT ( 'NONE',  ( 7.938121089952706377, 121.9582077959725979, -0.6488383765127299085 ) ) ;
#11192 = CARTESIAN_POINT ( 'NONE',  ( -47.00737061382944404, 25.44871393995562769, -1.744193148937779769 ) ) ;
#11193 = ORIENTED_EDGE ( 'NONE', *, *, #11494, .T. ) ;
#11194 = CARTESIAN_POINT ( 'NONE',  ( 1.008887259173379736, 118.7629491485454025, -1.225340056906602415 ) ) ;
#11195 = CARTESIAN_POINT ( 'NONE',  ( -9.051149985089010030, 123.9289873439938674, -0.3396360471471666087 ) ) ;
#11196 = CARTESIAN_POINT ( 'NONE',  ( 2.037655544652288597, -15.20941935993469585, 5.943311982828837436 ) ) ;
#11197 = CARTESIAN_POINT ( 'NONE',  ( -21.77700140173218202, 149.0176745010074342, 1.274060564799276873 ) ) ;
#11198 = CARTESIAN_POINT ( 'NONE',  ( -13.59117098936157575, 150.2425924485623057, -0.2715839415567423143 ) ) ;
#11199 = CARTESIAN_POINT ( 'NONE',  ( 21.89464077100137018, 151.4392833230981239, 0.5893027811483441125 ) ) ;
#11200 = CARTESIAN_POINT ( 'NONE',  ( 7.043631758970988699, 122.0730096003205745, 0.1795708586965836517 ) ) ;
#11201 = EDGE_CURVE ( 'NONE', #32125, #1397, #29043, .T. ) ;
#11202 = ORIENTED_EDGE ( 'NONE', *, *, #11560, .T. ) ;
#11203 = CARTESIAN_POINT ( 'NONE',  ( 0.9442757308971110319, 28.15415565245834628, -0.2560175424543267297 ) ) ;
#11204 = EDGE_CURVE ( 'NONE', #31590, #3167, #40177, .T. ) ;
#11205 = CARTESIAN_POINT ( 'NONE',  ( -13.43845804798116106, 156.9141898299356512, -0.2685323735513600041 ) ) ;
#11206 = CARTESIAN_POINT ( 'NONE',  ( -41.05189575270516400, 23.09451173561988213, 0.7619999999999945706 ) ) ;
#11207 = ORIENTED_EDGE ( 'NONE', *, *, #31822, .T. ) ;
#11208 = DIRECTION ( 'NONE',  ( 4.017660918040594346E-17, -1.000000000000000000, -2.376309959284834438E-19 ) ) ;
#11209 = ORIENTED_EDGE ( 'NONE', *, *, #4240, .F. ) ;
#11210 = CARTESIAN_POINT ( 'NONE',  ( 5.083929588455360360, 119.2653419761957423, 1.105484519010427880 ) ) ;
#11211 = CARTESIAN_POINT ( 'NONE',  ( 0.2036312542886812293, -3.545347522689146214, -4.628372119175537591 ) ) ;
#11212 = CARTESIAN_POINT ( 'NONE',  ( 20.70408045738742686, 151.0745573368290593, 1.983427051661964535 ) ) ;
#11213 = CARTESIAN_POINT ( 'NONE',  ( -54.14414085402640353, 8.624088997047390848, -3.578441826534806580 ) ) ;
#11214 = CARTESIAN_POINT ( 'NONE',  ( 13.28772774122543332, 155.5383117973235585, -1.582857276444406436 ) ) ;
#11215 = CARTESIAN_POINT ( 'NONE',  ( -2.168033660621066172, 0.5777166996233511487, 4.103230905123370853 ) ) ;
#11216 = CARTESIAN_POINT ( 'NONE',  ( 0.01645572339161321951, 159.4324016994384010, -0.8235116888278192215 ) ) ;
#11217 = CARTESIAN_POINT ( 'NONE',  ( 4.840817968818798889, 117.7364599323587697, -0.8494325157683647598 ) ) ;
#11218 = EDGE_LOOP ( 'NONE', ( #25499, #39290, #6875, #28888 ) ) ;
#11219 = CARTESIAN_POINT ( 'NONE',  ( -15.25729751669411627, 143.4548391324710224, -0.07249109134377340613 ) ) ;
#11220 = CARTESIAN_POINT ( 'NONE',  ( 4.692294315076144251, -14.85586321182354119, 4.526698459197877611 ) ) ;
#11221 = DIRECTION ( 'NONE',  ( -0.8745520943968281280, 0.4849315768086481238, 5.653143757709536353E-15 ) ) ;
#11222 = FACE_OUTER_BOUND ( 'NONE', #815, .T. ) ;
#11223 = ORIENTED_EDGE ( 'NONE', *, *, #4045, .F. ) ;
#11224 = CARTESIAN_POINT ( 'NONE',  ( 19.20800265940873786, 147.1635184732690220, 2.509201515169785957 ) ) ;
#11225 = FACE_OUTER_BOUND ( 'NONE', #11985, .T. ) ;
#11226 = CARTESIAN_POINT ( 'NONE',  ( -29.73153358407946101, 68.50109170616188692, -1.270000000000007123 ) ) ;
#11227 = CARTESIAN_POINT ( 'NONE',  ( -10.29385411648731186, 157.8242135995235458, 0.8711791838966671531 ) ) ;
#11229 = ADVANCED_FACE ( 'NONE', ( #26753 ), #367, .T. ) ;
#11228 = CARTESIAN_POINT ( 'NONE',  ( -7.544985805786585509, 7.895591250050960852, -3.771097921825450783 ) ) ;
#11230 = CARTESIAN_POINT ( 'NONE',  ( 6.352854517228291975, 155.4084287100276072, 1.029490774253102758 ) ) ;
#11231 = CARTESIAN_POINT ( 'NONE',  ( 13.85159022459153988, 12.96416000000000146, -5.016499999999999737 ) ) ;
#11232 = AXIS2_PLACEMENT_3D ( 'NONE', #24220, #31243, #37231 ) ;
#11233 = CARTESIAN_POINT ( 'NONE',  ( 15.03447867299173879, 120.7699597703182945, -0.2997422626971646409 ) ) ;
#11234 = CARTESIAN_POINT ( 'NONE',  ( 13.85159022459153988, 12.96416000000000146, -5.016499999999999737 ) ) ;
#11235 = CARTESIAN_POINT ( 'NONE',  ( -57.28641868539627779, 2.042781982619619630, 1.582485259194238658 ) ) ;
#11236 = DIRECTION ( 'NONE',  ( -4.017660918040594346E-17, 1.000000000000000000, 2.376309959284834438E-19 ) ) ;
#11237 = CARTESIAN_POINT ( 'NONE',  ( -58.50860430493789721, 0.7049166599848305514, 0.9756837515128383709 ) ) ;
#11238 = CARTESIAN_POINT ( 'NONE',  ( -58.20197065718431162, 0.6251715515077186369, 1.133219051752172080 ) ) ;
#11239 = CARTESIAN_POINT ( 'NONE',  ( -10.28897677580358305, 57.14999999999998437, 5.016499999999999737 ) ) ;
#11240 = CARTESIAN_POINT ( 'NONE',  ( -4.122882846571666704, 118.2429491485453354, 0.1811355980067066163 ) ) ;
#11241 = CARTESIAN_POINT ( 'NONE',  ( 2.178604253908287269, 106.5598271223812787, -4.865891711899141825 ) ) ;
#11242 = ORIENTED_EDGE ( 'NONE', *, *, #28571, .T. ) ;
#11243 = CARTESIAN_POINT ( 'NONE',  ( -49.56090548067184898, 17.87959676410238430, 5.165259844110607013 ) ) ;
#11244 = CARTESIAN_POINT ( 'NONE',  ( -8.245768994288328102, 120.2537849201367095, -1.446217431822895083 ) ) ;
#11245 = CARTESIAN_POINT ( 'NONE',  ( -5.469471049222605075, 117.5088849381099436, -0.8278104034524697008 ) ) ;
#11246 = CARTESIAN_POINT ( 'NONE',  ( 4.242344989534921673, 118.2250577600451180, 0.4716094826914004612 ) ) ;
#11247 = CARTESIAN_POINT ( 'NONE',  ( -8.311356586562078874, 122.7091975629380585, -0.7066836605292579065 ) ) ;
#11248 = CARTESIAN_POINT ( 'NONE',  ( -0.3866802643631708225, 115.7034476216335150, -1.763796639264662014 ) ) ;
#11249 = LINE ( 'NONE', #28280, #824 ) ;
#11250 = EDGE_CURVE ( 'NONE', #35053, #3380, #17487, .T. ) ;
#11251 = ORIENTED_EDGE ( 'NONE', *, *, #15470, .F. ) ;
#11252 = CARTESIAN_POINT ( 'NONE',  ( 6.943414100881801332, 121.8132169909553966, -0.01755787080488244861 ) ) ;
#11253 = CARTESIAN_POINT ( 'NONE',  ( -0.7424407951590874521, 156.5584078035761593, -0.9879031837870262400 ) ) ;
#11254 = CARTESIAN_POINT ( 'NONE',  ( -41.05189575270519242, 23.09451173561980042, -1.270000000000005125 ) ) ;
#11255 = CARTESIAN_POINT ( 'NONE',  ( -46.36020037345180356, 20.58642004075764476, 4.649377256144936688 ) ) ;
#11256 = CARTESIAN_POINT ( 'NONE',  ( 7.794969618361607289, 122.5994144671777519, 0.004875389051802769477 ) ) ;
#11257 = CARTESIAN_POINT ( 'NONE',  ( -15.72449225221075508, 145.6795444674731641, -0.1123860360721776058 ) ) ;
#11258 = CARTESIAN_POINT ( 'NONE',  ( -33.20758249455312239, 49.81222039523557044, -1.524000000000005572 ) ) ;
#11259 = CARTESIAN_POINT ( 'NONE',  ( 2.866641708098013996, 116.8851979753409580, 0.4370437109847169488 ) ) ;
#11260 = CARTESIAN_POINT ( 'NONE',  ( 6.059261036834384662, 77.01756249999996840, -5.016499999999999737 ) ) ;
#11262 = CARTESIAN_POINT ( 'NONE',  ( 2.946692055775869346, 159.0164033662945258, -1.213088979206726092 ) ) ;
#11261 = CARTESIAN_POINT ( 'NONE',  ( 2.930607426163104545, -14.92094031927118714, 4.083576684136651203 ) ) ;
#11263 = CARTESIAN_POINT ( 'NONE',  ( -6.644289941094903895, 120.1594786313440011, 0.9502652795725031742 ) ) ;
#11264 = CARTESIAN_POINT ( 'NONE',  ( -0.9608913863540493594, -11.74124177384809542, -0.1559992898937096195 ) ) ;
#11265 = CARTESIAN_POINT ( 'NONE',  ( -6.899218498549055667, 117.3903047926647787, -0.5887349169472961830 ) ) ;
#11266 = CARTESIAN_POINT ( 'NONE',  ( 0.9476013557874021220, 22.48150014755712078, -0.2491751695904415032 ) ) ;
#11267 = VERTEX_POINT ( 'NONE', #575 ) ;
#11268 = ADVANCED_FACE ( 'NONE', ( #4191 ), #13549, .F. ) ;
#11269 = CARTESIAN_POINT ( 'NONE',  ( -52.42931032121356338, 11.92852722686772005, 4.179465640474072430 ) ) ;
#11270 = CONTEXT_DEPENDENT_SHAPE_REPRESENTATION ( #5589, #3831 ) ;
#11271 = AXIS2_PLACEMENT_3D ( 'NONE', #20828, #27033, #10835 ) ;
#11272 = CARTESIAN_POINT ( 'NONE',  ( -9.625125523471179889, 124.0356975489027036, 0.4152212053287654969 ) ) ;
#11273 = CARTESIAN_POINT ( 'NONE',  ( 4.637598599007382916, -11.68863464395987428, 0.6963472677309354708 ) ) ;
#11274 = CARTESIAN_POINT ( 'NONE',  ( 6.553475369667514983, 120.9817801663137971, -0.6941111757064588605 ) ) ;
#11275 = ORIENTED_EDGE ( 'NONE', *, *, #23821, .F. ) ;
#11276 = CARTESIAN_POINT ( 'NONE',  ( 0.7902916588979997936, 115.7028258067067696, 1.754551533761817161 ) ) ;
#11277 = CARTESIAN_POINT ( 'NONE',  ( 2.870361413894247260, -14.70454541201141119, 4.341408117703424274 ) ) ;
#11278 = CARTESIAN_POINT ( 'NONE',  ( -5.208405493689605592, 31.38331509014777154, -0.6716542322870747705 ) ) ;
#11279 = CARTESIAN_POINT ( 'NONE',  ( 15.73072674608048338, 146.8994026175788008, 0.1860059585639197988 ) ) ;
#11280 = EDGE_LOOP ( 'NONE', ( #36640, #19553, #17378, #21240 ) ) ;
#11281 = CARTESIAN_POINT ( 'NONE',  ( 4.966515250750292765, 118.7197616721209670, 1.086191325688556919 ) ) ;
#11282 = CARTESIAN_POINT ( 'NONE',  ( 2.987839817974693002, 108.3452893864955087, 4.269252900506888437 ) ) ;
#11283 = CARTESIAN_POINT ( 'NONE',  ( -0.02983097946891718685, 117.3993836135855418, 1.492864285907047561 ) ) ;
#11284 = EDGE_CURVE ( 'NONE', #8589, #27091, #33782, .T. ) ;
#11285 = DIRECTION ( 'NONE',  ( -0.9469626219732555361, -0.3213437296502561491, -8.537024980200885913E-16 ) ) ;
#11286 = CARTESIAN_POINT ( 'NONE',  ( 5.797208421814580959, 116.9567987913546006, -0.006983082090869404714 ) ) ;
#11287 = EDGE_CURVE ( 'NONE', #3752, #11376, #11685, .T. ) ;
#11288 = CARTESIAN_POINT ( 'NONE',  ( 14.80692295515832058, 78.04183178746352212, -5.016499999999999737 ) ) ;
#11289 = ADVANCED_FACE ( 'NONE', ( #32943 ), #36556, .F. ) ;
#11290 = CARTESIAN_POINT ( 'NONE',  ( 1.779277909118444301, -15.52187590737404221, 5.925248486025581407 ) ) ;
#11291 = CARTESIAN_POINT ( 'NONE',  ( 4.756814333351318425, 117.4032681585794791, 1.206529664789174339 ) ) ;
#11292 = LINE ( 'NONE', #37281, #3546 ) ;
#11293 = CARTESIAN_POINT ( 'NONE',  ( -4.692483838673591201, 117.9823884840737094, 0.6748481237222451190 ) ) ;
#11294 = VECTOR ( 'NONE', #5440, 1000.000000000000000 ) ;
#11295 = EDGE_LOOP ( 'NONE', ( #8270, #35214, #13541, #28004, #5878 ) ) ;
#11296 = CARTESIAN_POINT ( 'NONE',  ( -6.616342194955179501, 21.00577804425827111, -5.270772580892629122 ) ) ;
#11297 = CARTESIAN_POINT ( 'NONE',  ( -5.678132272250597801, 118.5192932620585111, -1.203295300969776660 ) ) ;
#11298 = CARTESIAN_POINT ( 'NONE',  ( -1.155851712377470530, 107.4826764677166864, -4.671650131992445054 ) ) ;
#11299 = CARTESIAN_POINT ( 'NONE',  ( 4.886742582885162278, 117.6636387720722325, 0.9830068712545340093 ) ) ;
#11300 = CARTESIAN_POINT ( 'NONE',  ( -11.11710224467015351, 56.30409367656761788, -5.016499999999996184 ) ) ;
#11301 = CARTESIAN_POINT ( 'NONE',  ( -0.004379098344380600097, 122.8649044353672934, 0.2191479880734042429 ) ) ;
#11302 = CARTESIAN_POINT ( 'NONE',  ( 4.617411384770501392, 7.639850289152962048, 0.2838591255797697777 ) ) ;
#11303 = DIRECTION ( 'NONE',  ( -0.000000000000000000, 1.000000000000000000, -0.000000000000000000 ) ) ;
#11304 = CARTESIAN_POINT ( 'NONE',  ( -4.831905115772525683, 118.5264896598256854, 0.7498331390262092944 ) ) ;
#11305 = CARTESIAN_POINT ( 'NONE',  ( 2.509002420848308823, -14.82469439542799527, 5.007744185041904217 ) ) ;
#11306 = CARTESIAN_POINT ( 'NONE',  ( 4.831936455160824373, 120.7138498849978987, -0.2122769985084470012 ) ) ;
#11307 = CARTESIAN_POINT ( 'NONE',  ( -2.010917461066705325, 115.7029473869310010, 1.638936349488617328 ) ) ;
#11308 = ORIENTED_EDGE ( 'NONE', *, *, #5033, .F. ) ;
#11309 = CARTESIAN_POINT ( 'NONE',  ( -4.505775810132860215, 104.6144662015457527, -1.759455372407346729 ) ) ;
#11310 = CARTESIAN_POINT ( 'NONE',  ( 4.228161069935173266, -15.38163066151135361, 0.6048619776675213666 ) ) ;
#11311 = CARTESIAN_POINT ( 'NONE',  ( -19.63947405400097779, 148.8045834396381508, 1.723899180582558310 ) ) ;
#11312 = CARTESIAN_POINT ( 'NONE',  ( 0.7179688673824197176, 19.28876970375581479, -0.6613080194383522681 ) ) ;
#11313 = ORIENTED_EDGE ( 'NONE', *, *, #41740, .F. ) ;
#11314 = ORIENTED_EDGE ( 'NONE', *, *, #28462, .F. ) ;
#11315 = CARTESIAN_POINT ( 'NONE',  ( -3.831877602099685198, 71.07198261757335445, -1.523999999999993804 ) ) ;
#11316 = CARTESIAN_POINT ( 'NONE',  ( 1.574582893473400746, 118.9836165220538504, 0.7747311016372978587 ) ) ;
#11317 =( NAMED_UNIT ( * ) PLANE_ANGLE_UNIT ( ) SI_UNIT ( $, .RADIAN. ) );
#11318 = CARTESIAN_POINT ( 'NONE',  ( -10.11798836042646244, 123.5826510519420509, 0.8100524519737971607 ) ) ;
#11319 = CARTESIAN_POINT ( 'NONE',  ( 17.68910244842765778, 0.6349999999999984546, 0.000000000000000000 ) ) ;
#11320 = CARTESIAN_POINT ( 'NONE',  ( 4.601232872588083112, 118.0405793793079283, -0.6545214583194519653 ) ) ;
#11321 = CARTESIAN_POINT ( 'NONE',  ( 11.08663849088095255, 154.4909003399924643, -1.626836423318808400 ) ) ;
#11322 = CARTESIAN_POINT ( 'NONE',  ( -6.753855533487248763, 118.7881172115286148, -1.217991184693928641 ) ) ;
#11323 = CYLINDRICAL_SURFACE ( 'NONE', #1839, 16.60960244842765832 ) ;
#11324 = VERTEX_POINT ( 'NONE', #23956 ) ;
#11325 = CIRCLE ( 'NONE', #10623, 0.2540000000000025016 ) ;
#11326 = CARTESIAN_POINT ( 'NONE',  ( 4.172298354059645220, 118.2392279447537220, -0.2172812281923733324 ) ) ;
#11327 = CARTESIAN_POINT ( 'NONE',  ( 9.542306315654297322, 124.2661852542617709, -0.2373755145837088965 ) ) ;
#11328 = EDGE_CURVE ( 'NONE', #32447, #17471, #26022, .T. ) ;
#11329 = VECTOR ( 'NONE', #789, 1000.000000000000114 ) ;
#11330 = VERTEX_POINT ( 'NONE', #8832 ) ;
#11331 = CARTESIAN_POINT ( 'NONE',  ( 2.102813808753936087, -15.18136450426021256, 5.202461169095355942 ) ) ;
#11332 = FACE_OUTER_BOUND ( 'NONE', #37421, .T. ) ;
#11333 = CARTESIAN_POINT ( 'NONE',  ( -54.56827866224503509, 7.775013980772373934, 3.396949012664772560 ) ) ;
#11334 = CARTESIAN_POINT ( 'NONE',  ( -4.598078022480850180, -10.86695742004451404, -0.5832510952623800593 ) ) ;
#11335 = CARTESIAN_POINT ( 'NONE',  ( 5.120605266512749942, 120.5246234221128248, 0.8194923670329071763 ) ) ;
#11336 = CARTESIAN_POINT ( 'NONE',  ( -3.958300029084214522, 28.23836431654049761, 1.224951011016432556 ) ) ;
#11337 = CARTESIAN_POINT ( 'NONE',  ( -5.007645675277699659, 117.8491495069952748, 0.5952962186315863269 ) ) ;
#11338 = AXIS2_PLACEMENT_3D ( 'NONE', #17918, #31765, #28144 ) ;
#11339 = EDGE_CURVE ( 'NONE', #35679, #14172, #15801, .T. ) ;
#11340 = CARTESIAN_POINT ( 'NONE',  ( 1.398650104629075797, 0.06838872207683838189, -4.420329592304430122 ) ) ;
#11341 = CARTESIAN_POINT ( 'NONE',  ( 15.73024628025046567, 145.6958675726371553, 0.4429222902984593091 ) ) ;
#11342 = CARTESIAN_POINT ( 'NONE',  ( -10.62867326514792410, 56.48194529650098872, 4.405924061720235763 ) ) ;
#11343 = EDGE_CURVE ( 'NONE', #34378, #11774, #31463, .T. ) ;
#11344 = CARTESIAN_POINT ( 'NONE',  ( -56.89722832398061314, 2.603431824206650536, -0.9028745487782567913 ) ) ;
#11345 = CARTESIAN_POINT ( 'NONE',  ( 2.176363917357261979, 116.2587084501870009, -0.1247648271736234021 ) ) ;
#11346 = AXIS2_PLACEMENT_3D ( 'NONE', #9547, #23145, #35333 ) ;
#11347 = CARTESIAN_POINT ( 'NONE',  ( 1.650612623617701257E-15, 17.14499999999999957, 0.000000000000000000 ) ) ;
#11348 = CARTESIAN_POINT ( 'NONE',  ( -1.899626047278970109, 106.4942957007743587, 4.984479252724743681 ) ) ;
#11349 = CARTESIAN_POINT ( 'NONE',  ( -6.442660433036017764, 29.32943145771791649, -0.01012415147099491285 ) ) ;
#11350 = CARTESIAN_POINT ( 'NONE',  ( 2.469379016249674486, 9.589258615745848147, -8.089366445887874235 ) ) ;
#11351 = CARTESIAN_POINT ( 'NONE',  ( -46.73713699923415277, 25.40205342722763859, 1.701536002565660510 ) ) ;
#11352 = CARTESIAN_POINT ( 'NONE',  ( -7.842268484490568348, 73.30875693322846587, 1.270000000000002904 ) ) ;
#11353 = DIRECTION ( 'NONE',  ( -0.4849315768086534528, -0.8745520943968250194, -1.030032898892974942E-16 ) ) ;
#11354 = CARTESIAN_POINT ( 'NONE',  ( -58.37241122568488549, -0.2962816677227753104, 0.2416009568453807987 ) ) ;
#11355 = CARTESIAN_POINT ( 'NONE',  ( -15.52406334459491255, 121.0440340969820596, 0.2084667659489263247 ) ) ;
#11356 = AXIS2_PLACEMENT_3D ( 'NONE', #736, #11139, #24125 ) ;
#11357 = EDGE_LOOP ( 'NONE', ( #12775, #34408, #17188, #20825 ) ) ;
#11358 = DIRECTION ( 'NONE',  ( 0.5149185422762221354, -0.8572391118119440101, 4.128606161907601007E-16 ) ) ;
#11359 = VERTEX_POINT ( 'NONE', #14573 ) ;
#11360 = CARTESIAN_POINT ( 'NONE',  ( -44.00561601145676605, 21.61144970255528008, -2.814601217460917404 ) ) ;
#11361 = CARTESIAN_POINT ( 'NONE',  ( -9.049782359939607446, 124.0675141969884692, -0.1808361888366265546 ) ) ;
#11362 = CARTESIAN_POINT ( 'NONE',  ( 4.209311184370442049, -15.24947937046475310, 4.910682269069504891 ) ) ;
#11363 = CARTESIAN_POINT ( 'NONE',  ( -20.28847770310441234, 149.9354415288716780, 1.565775960057087746 ) ) ;
#11364 = CARTESIAN_POINT ( 'NONE',  ( 22.48855060683864693, 149.3130771379323392, -0.8549704587061032202 ) ) ;
#11365 = CARTESIAN_POINT ( 'NONE',  ( 0.4746723515649934888, 24.68197512780947278, 4.609222710213416896 ) ) ;
#11366 = CARTESIAN_POINT ( 'NONE',  ( -5.710605682675778283, 159.1232349745254453, -0.3332304182141800353 ) ) ;
#11367 = CARTESIAN_POINT ( 'NONE',  ( -51.02349128109572263, 14.61359224283002511, -4.685075518275549911 ) ) ;
#11368 = ORIENTED_EDGE ( 'NONE', *, *, #16629, .T. ) ;
#11369 = CARTESIAN_POINT ( 'NONE',  ( -8.798071503329609300, 117.6842349159552867, -0.1758064076808953657 ) ) ;
#11370 = CARTESIAN_POINT ( 'NONE',  ( -14.72636943223162120, 131.2156652454908112, 1.433095336252470098 ) ) ;
#11371 = CARTESIAN_POINT ( 'NONE',  ( -52.16429070073207441, 12.35296858188530145, -4.167432729078118570 ) ) ;
#11372 = CARTESIAN_POINT ( 'NONE',  ( 10.43940122747806676, 155.6679353847891321, -1.745147575944303364 ) ) ;
#11373 = CARTESIAN_POINT ( 'NONE',  ( -18.99721151120906626, 152.1029585079319020, -2.158688780372492566 ) ) ;
#11374 = CARTESIAN_POINT ( 'NONE',  ( -47.67648637180143822, 19.71513033058998232, -5.327979952964785326 ) ) ;
#11375 = CARTESIAN_POINT ( 'NONE',  ( 15.86865214134231650, 143.7482200480382346, -0.8098737496861395657 ) ) ;
#11376 = VERTEX_POINT ( 'NONE', #18184 ) ;
#11377 = CARTESIAN_POINT ( 'NONE',  ( -2.442377090744360935, 119.5064228623769225, -0.7372000016323176919 ) ) ;
#11378 = CARTESIAN_POINT ( 'NONE',  ( 2.770358398913809861, -15.65020961539316602, 4.804192819214700982 ) ) ;
#11379 = CARTESIAN_POINT ( 'NONE',  ( -4.522469723682791987, 118.1110480853273543, -0.6888394697316272408 ) ) ;
#11380 = CARTESIAN_POINT ( 'NONE',  ( -58.83227707057486811, -0.08366279997995551554, -1.273395421382134774E-15 ) ) ;
#11381 = CIRCLE ( 'NONE', #38616, 0.5080000000000014504 ) ;
#11382 = CARTESIAN_POINT ( 'NONE',  ( -4.916103084303564685, 117.4785598539236986, 0.9401160097163984153 ) ) ;
#11383 = CARTESIAN_POINT ( 'NONE',  ( 8.285153246922861925, 121.0263440914440736, 1.363535410649704849 ) ) ;
#11384 = DIRECTION ( 'NONE',  ( -0.000000000000000000, -0.000000000000000000, -1.000000000000000000 ) ) ;
#11385 = EDGE_CURVE ( 'NONE', #4082, #14480, #21901, .T. ) ;
#11386 = CARTESIAN_POINT ( 'NONE',  ( 14.87733005835116096, 120.3210621052586475, 0.2473824415510234298 ) ) ;
#11387 = EDGE_CURVE ( 'NONE', #36274, #35500, #40315, .T. ) ;
#11388 = CARTESIAN_POINT ( 'NONE',  ( 7.354229849910361771, -2.730604093522916109, 4.103208822889532925 ) ) ;
#11389 = CARTESIAN_POINT ( 'NONE',  ( 15.44350913713179274, 147.8441550597069352, 0.7585189891071874024 ) ) ;
#11390 = CARTESIAN_POINT ( 'NONE',  ( 4.263816225517785163, 117.9847045463029076, -0.8023379542233743944 ) ) ;
#11391 = CARTESIAN_POINT ( 'NONE',  ( -6.451606698686837575E-14, 65.62546620154573418, 4.217636114931141265E-29 ) ) ;
#11392 = CARTESIAN_POINT ( 'NONE',  ( -4.411262628599642355, 117.9394518360175539, 1.007827510414607719 ) ) ;
#11393 = DIRECTION ( 'NONE',  ( 6.353134868986659519E-16, -1.000000000000000000, 0.000000000000000000 ) ) ;
#11394 = TOROIDAL_SURFACE ( 'NONE', #41340, 0.7620000000000000107, 0.2540000000000000036 ) ;
#11395 = CARTESIAN_POINT ( 'NONE',  ( -58.37241122568488549, -0.2962816677227753104, -1.039428729632917149E-14 ) ) ;
#11396 = CARTESIAN_POINT ( 'NONE',  ( -23.40703704692324649, 142.8142681763856388, -0.3922439843285878136 ) ) ;
#11397 = VERTEX_POINT ( 'NONE', #33986 ) ;
#11398 = CARTESIAN_POINT ( 'NONE',  ( -48.57235503434458224, 24.64055110436136431, -0.2038152558995032504 ) ) ;
#11399 = CARTESIAN_POINT ( 'NONE',  ( -5.885250668960954279, 121.3397778740266233, -0.3730483248005934671 ) ) ;
#11400 = CARTESIAN_POINT ( 'NONE',  ( -8.044334902818970789, 121.4620208242423018, 0.8712540157608216207 ) ) ;
#11401 = ORIENTED_EDGE ( 'NONE', *, *, #39176, .F. ) ;
#11402 = CARTESIAN_POINT ( 'NONE',  ( 4.855010706778257301, 115.6909491485452435, -1.281361498471799365 ) ) ;
#11403 = CARTESIAN_POINT ( 'NONE',  ( -15.67344897587556396, 147.2319784351455780, -0.6427785636300452632 ) ) ;
#11404 = CARTESIAN_POINT ( 'NONE',  ( 4.627184959846470491, -11.70336558297383611, 0.7419505617825855603 ) ) ;
#11405 = CARTESIAN_POINT ( 'NONE',  ( -19.57327063168412451, 152.2820370773569323, 1.161482255138348130 ) ) ;
#11406 = CARTESIAN_POINT ( 'NONE',  ( 5.692269266617126178, 78.90431106374074943, -5.047924920909481195 ) ) ;
#11407 = CARTESIAN_POINT ( 'NONE',  ( 20.68667083660084316, 152.5691845998198346, 0.5628278541506293031 ) ) ;
#11408 = CARTESIAN_POINT ( 'NONE',  ( 15.72385166996613570, 146.8976323831864477, 0.3141999770531622160 ) ) ;
#11409 = CARTESIAN_POINT ( 'NONE',  ( 1.824656174747253168, -15.25388738520313225, 5.420764384989097628 ) ) ;
#11410 = CARTESIAN_POINT ( 'NONE',  ( 0.5513313392710353922, 29.23057874652566923, -0.8050760855368327418 ) ) ;
#11411 = CARTESIAN_POINT ( 'NONE',  ( -3.300851927471685432, 159.4676453237595410, -0.08072286411353189750 ) ) ;
#11412 = CARTESIAN_POINT ( 'NONE',  ( -46.58415285064482703, 20.65776990352928877, -4.869103069372410886 ) ) ;
#11413 = ORIENTED_EDGE ( 'NONE', *, *, #31584, .F. ) ;
#11414 = DIRECTION ( 'NONE',  ( -0.9998004120163609398, 0.000000000000000000, -0.01997839162482749689 ) ) ;
#11415 = ORIENTED_EDGE ( 'NONE', *, *, #11052, .T. ) ;
#11416 = CARTESIAN_POINT ( 'NONE',  ( -6.195589306716754230, 119.0760157020015129, 1.000162390493852138 ) ) ;
#11417 = CARTESIAN_POINT ( 'NONE',  ( -0.7749869142727341398, -12.81603963768374044, -4.556214072895795830 ) ) ;
#11418 = CARTESIAN_POINT ( 'NONE',  ( 22.03849170948978298, 148.8299554149626260, 2.028895537808247607 ) ) ;
#11419 = CARTESIAN_POINT ( 'NONE',  ( -58.34556966141492040, -0.2407783058112067387, -0.1938516799453308959 ) ) ;
#11420 = CARTESIAN_POINT ( 'NONE',  ( 4.101170551582069557, 118.4217611105734846, -0.8082045602434785314 ) ) ;
#11421 = CARTESIAN_POINT ( 'NONE',  ( 5.482275759465073506, 24.31437370403141784, -6.390863428313894978 ) ) ;
#11422 = CARTESIAN_POINT ( 'NONE',  ( -0.3477286622124562965, 117.0882377308211773, -0.3718801884458513007 ) ) ;
#11423 = CARTESIAN_POINT ( 'NONE',  ( 4.953217389033119034, 117.5439133103682110, -0.8526271701310890183 ) ) ;
#11424 = VERTEX_POINT ( 'NONE', #17767 ) ;
#11425 = CARTESIAN_POINT ( 'NONE',  ( -6.494470876743877241, 121.7611753534313550, -0.002333837952680380395 ) ) ;
#11426 = CARTESIAN_POINT ( 'NONE',  ( 6.243909332557862513, -14.15813981987112946, 1.248599486541194681 ) ) ;
#11427 = DIRECTION ( 'NONE',  ( -1.000000000000000000, 0.000000000000000000, 0.000000000000000000 ) ) ;
#11428 = ORIENTED_EDGE ( 'NONE', *, *, #18395, .F. ) ;
#11429 = CARTESIAN_POINT ( 'NONE',  ( -0.03245814172817904769, 157.7902383798253538, 1.624338139048501883 ) ) ;
#11430 = CARTESIAN_POINT ( 'NONE',  ( -4.095482865093060809, 71.62450171983788039, 1.270000000000005347 ) ) ;
#11431 = CARTESIAN_POINT ( 'NONE',  ( -7.961576494521614755, 72.55615504727386167, -1.523999999999996247 ) ) ;
#11432 = CARTESIAN_POINT ( 'NONE',  ( -0.9959059386944214554, 109.5507526474568607, 3.831187545969641395 ) ) ;
#11433 = CARTESIAN_POINT ( 'NONE',  ( -0.4581589521676752153, 10.92003791307801208, 8.418874016967684781 ) ) ;
#11434 = CARTESIAN_POINT ( 'NONE',  ( 2.692664463852532108, 120.6505882111413683, 0.3986361418428905901 ) ) ;
#11435 = CARTESIAN_POINT ( 'NONE',  ( -4.744878939582974020, 118.5930653697794384, -1.015278495842544482 ) ) ;
#11436 = CARTESIAN_POINT ( 'NONE',  ( 22.64827982350381319, 150.3405807453409579, -0.2709709482530829328 ) ) ;
#11437 = DIRECTION ( 'NONE',  ( -0.8745520943968423389, 0.4849315768086222556, -5.691349986800581405E-16 ) ) ;
#11438 = CARTESIAN_POINT ( 'NONE',  ( -57.88388651883108338, 0.7560526178991631152, 1.004446660134626912 ) ) ;
#11439 = DIRECTION ( 'NONE',  ( -0.9998004120163608288, 0.000000000000000000, -0.01997839162482749342 ) ) ;
#11440 = CARTESIAN_POINT ( 'NONE',  ( -52.50609217148328867, 12.02659833652626808, 4.260190243505617147 ) ) ;
#11441 = DIRECTION ( 'NONE',  ( 0.9998004120163609398, 0.000000000000000000, 0.01997839162482749689 ) ) ;
#11442 = CARTESIAN_POINT ( 'NONE',  ( -4.161924923179597613, 118.2393572185476813, 0.2292740676127673349 ) ) ;
#11443 = CARTESIAN_POINT ( 'NONE',  ( 2.100690617099141289, 106.6620211890832195, -4.900160429241310567 ) ) ;
#11444 = VERTEX_POINT ( 'NONE', #37791 ) ;
#11445 = CARTESIAN_POINT ( 'NONE',  ( -52.42133349025997546, 11.92692459785933679, 4.172736198742178715 ) ) ;
#11446 = CARTESIAN_POINT ( 'NONE',  ( 6.260578210526342779, 119.7762395299752427, -0.9857573057594839483 ) ) ;
#11447 = DIRECTION ( 'NONE',  ( 1.000000000000000000, 0.000000000000000000, 0.000000000000000000 ) ) ;
#11448 = CARTESIAN_POINT ( 'NONE',  ( 4.374182175873362333, 118.1842224889937256, 0.5915927881597164983 ) ) ;
#11449 = CARTESIAN_POINT ( 'NONE',  ( -1.544162262334034308, 120.7289827521893670, -0.2751094044070050981 ) ) ;
#11450 = CARTESIAN_POINT ( 'NONE',  ( -6.059261036834475256, 57.15000000000000568, 5.016499999999999737 ) ) ;
#11451 = ORIENTED_EDGE ( 'NONE', *, *, #3434, .F. ) ;
#11452 = CARTESIAN_POINT ( 'NONE',  ( 3.548611814566905664, 16.26088872207684943, 2.983771105379771971 ) ) ;
#11453 = CARTESIAN_POINT ( 'NONE',  ( -11.45052794940122709, 153.2879862121713757, -1.711174725579351463 ) ) ;
#11454 = FACE_OUTER_BOUND ( 'NONE', #11520, .T. ) ;
#11455 = CARTESIAN_POINT ( 'NONE',  ( -43.90699889932533040, 21.43881162649801908, 2.872437248226452411 ) ) ;
#11456 = CARTESIAN_POINT ( 'NONE',  ( -20.79116009376201646, 79.67004825550966984, -1.524000000000004018 ) ) ;
#11457 = CARTESIAN_POINT ( 'NONE',  ( 6.075908422621684402, 121.4480918675926517, 0.1456406178164729448 ) ) ;
#11458 = CIRCLE ( 'NONE', #25748, 3.683000000000001162 ) ;
#11459 = DIRECTION ( 'NONE',  ( 0.3256999990547897461, 0.9454731675810318370, 0.000000000000000000 ) ) ;
#11460 = CARTESIAN_POINT ( 'NONE',  ( 22.59100494123591929, 149.3758529064199934, 1.630758705999802327 ) ) ;
#11461 = CARTESIAN_POINT ( 'NONE',  ( 5.241362157049035631, 88.73331249999999670, -5.310945289804168468 ) ) ;
#11463 = CARTESIAN_POINT ( 'NONE',  ( 17.75928342660597181, 128.5843929717815115, -1.279242276855531157 ) ) ;
#11462 = CARTESIAN_POINT ( 'NONE',  ( 3.220686968960577712, -14.48737495597347902, 2.486805533510040078 ) ) ;
#11464 = CARTESIAN_POINT ( 'NONE',  ( -10.01831529487298234, 155.4362223408194836, 1.706801840347523358 ) ) ;
#11465 = AXIS2_PLACEMENT_3D ( 'NONE', #30465, #23004, #10032 ) ;
#11466 = CARTESIAN_POINT ( 'NONE',  ( -4.556403025205056245, 17.84477460162305107, -0.8067276567318153457 ) ) ;
#11467 = CARTESIAN_POINT ( 'NONE',  ( -1.362313394648154485, 159.5452856091935132, -0.5382632954014162641 ) ) ;
#11468 = CARTESIAN_POINT ( 'NONE',  ( 0.9697834966998255535, 21.94565095173003400, 0.09096683575692042500 ) ) ;
#11469 = ORIENTED_EDGE ( 'NONE', *, *, #11519, .F. ) ;
#11470 = CARTESIAN_POINT ( 'NONE',  ( -50.29507671575589001, 15.72791930032348873, 4.796563717952099459 ) ) ;
#11471 = CARTESIAN_POINT ( 'NONE',  ( -1.553919893302708743, 120.7289827521893670, 0.2132023499116274534 ) ) ;
#11472 = CARTESIAN_POINT ( 'NONE',  ( 4.871446434089309108, -12.86987818651588711, 2.618604111146097591 ) ) ;
#11473 = CARTESIAN_POINT ( 'NONE',  ( 17.12300761254194725, 147.7912591418244403, -1.363423146152763943 ) ) ;
#11474 = VERTEX_POINT ( 'NONE', #30566 ) ;
#11475 = CARTESIAN_POINT ( 'NONE',  ( 2.609136386454064649, 115.7032548281754458, 1.690807494954503998 ) ) ;
#11476 = ORIENTED_EDGE ( 'NONE', *, *, #5278, .T. ) ;
#11477 = CARTESIAN_POINT ( 'NONE',  ( 2.917951099372082080, -14.56804730652265434, 4.441407531948645904 ) ) ;
#11478 = CARTESIAN_POINT ( 'NONE',  ( -4.794479500060544019, 117.6747142900968015, -1.098999508304763006 ) ) ;
#11479 = ADVANCED_FACE ( 'NONE', ( #34820, #14782 ), #5436, .F. ) ;
#11480 = CARTESIAN_POINT ( 'NONE',  ( 1.572870384098442376, 156.2570369995211479, -0.04660437260867165976 ) ) ;
#11481 = ORIENTED_EDGE ( 'NONE', *, *, #5292, .T. ) ;
#11482 = CARTESIAN_POINT ( 'NONE',  ( 17.92333008985171361, 151.7072807693909340, 2.394054079121862078 ) ) ;
#11483 = DIRECTION ( 'NONE',  ( -0.9998004120163608288, 0.000000000000000000, -0.01997839162482747608 ) ) ;
#11484 = SHAPE_REPRESENTATION ( 'Corkscrew Body', ( #3275 ), #40037 ) ;
#11485 = DIRECTION ( 'NONE',  ( -1.000000000000000000, 0.000000000000000000, 0.000000000000000000 ) ) ;
#11486 = ADVANCED_FACE ( 'NONE', ( #14362 ), #2242, .T. ) ;
#11487 = DIRECTION ( 'NONE',  ( -0.8745520943968245753, 0.4849315768086539524, -5.691349986800526185E-16 ) ) ;
#11488 = CARTESIAN_POINT ( 'NONE',  ( 21.55438672983820680, 132.6250929350426020, 0.2276674992303582834 ) ) ;
#11489 = AXIS2_PLACEMENT_3D ( 'NONE', #21235, #5093, #9317 ) ;
#11490 = DIRECTION ( 'NONE',  ( 0.1906721105964953034, -0.9816537812491112902, 0.000000000000000000 ) ) ;
#11491 = CARTESIAN_POINT ( 'NONE',  ( 1.870953937135939604, -15.14421219162230514, 5.894613027636500746 ) ) ;
#11492 = CARTESIAN_POINT ( 'NONE',  ( 10.96186877710231755, 56.39406130473820156, 5.016499999999998849 ) ) ;
#11493 = DIRECTION ( 'NONE',  ( -1.000000000000000000, 0.000000000000000000, 0.000000000000000000 ) ) ;
#11494 = EDGE_CURVE ( 'NONE', #38361, #21382, #11074, .T. ) ;
#11495 = CARTESIAN_POINT ( 'NONE',  ( -4.639824337899648654, 117.9546834919162279, 0.7580944945253588196 ) ) ;
#11496 = ORIENTED_EDGE ( 'NONE', *, *, #40277, .T. ) ;
#11497 = ORIENTED_EDGE ( 'NONE', *, *, #870, .F. ) ;
#11498 = DIRECTION ( 'NONE',  ( -0.9454731675810338354, 0.3256999990547844170, -5.459396135145338185E-16 ) ) ;
#11499 = CARTESIAN_POINT ( 'NONE',  ( 8.597804290853659381, 118.7612935373479814, -0.8549226474316184987 ) ) ;
#11500 = CARTESIAN_POINT ( 'NONE',  ( -2.044121638888310777, 114.8832439220486350, -1.972317757894941570 ) ) ;
#11501 = CARTESIAN_POINT ( 'NONE',  ( 4.947893305883586557, 117.4718310785403332, 1.024415023481761056 ) ) ;
#11502 = CARTESIAN_POINT ( 'NONE',  ( 17.14499999999999957, 71.11999999999999034, -1.904999999999999583 ) ) ;
#11503 = CARTESIAN_POINT ( 'NONE',  ( -0.3585272760099085243, 113.0327356262573915, 2.615547676125328014 ) ) ;
#11504 = CARTESIAN_POINT ( 'NONE',  ( 3.315635589170360831, -10.27688868798473720, -3.234826238065521053 ) ) ;
#11505 = CARTESIAN_POINT ( 'NONE',  ( -58.20820809768405013, 1.420579653404072218, 1.355822160094593887 ) ) ;
#11506 = CARTESIAN_POINT ( 'NONE',  ( -17.14500000000000313, 71.11999999999999034, -5.080000000000000959 ) ) ;
#11507 = CARTESIAN_POINT ( 'NONE',  ( 3.480220535011376182, -13.66934472092314046, 3.064489479733436106 ) ) ;
#11508 = CARTESIAN_POINT ( 'NONE',  ( 6.874578817172041667, 121.8312213470058225, -0.01890686361713992888 ) ) ;
#11509 = CARTESIAN_POINT ( 'NONE',  ( 0.9635274152722271834, 39.00291388108365709, 1.327368659714503574 ) ) ;
#11510 = ADVANCED_FACE ( 'NONE', ( #2245 ), #18392, .T. ) ;
#11511 = DIRECTION ( 'NONE',  ( 0.9998004120163608288, 0.000000000000000000, 0.01997839162482749342 ) ) ;
#11512 = CARTESIAN_POINT ( 'NONE',  ( -4.556757383386185190, 31.49269130883712720, -0.6906699653381264126 ) ) ;
#11513 = ORIENTED_EDGE ( 'NONE', *, *, #406, .F. ) ;
#11514 = CARTESIAN_POINT ( 'NONE',  ( -3.608349438833787559, 105.1232419943577554, -3.942834359180669601 ) ) ;
#11515 = CARTESIAN_POINT ( 'NONE',  ( 4.514867502249738429, -15.46117574218924773, 1.158286244139274279 ) ) ;
#11516 = CARTESIAN_POINT ( 'NONE',  ( -3.262238196373905108, 118.8118204130220903, 0.7766580032327177197 ) ) ;
#11517 = CARTESIAN_POINT ( 'NONE',  ( 0.9727671068909850005, -1.206248505109467795, 0.1081409728948927729 ) ) ;
#11518 = CARTESIAN_POINT ( 'NONE',  ( -0.8572797930410298584, 14.11360927180527014, 0.4650159543037101773 ) ) ;
#11519 = EDGE_CURVE ( 'NONE', #22696, #31590, #4815, .T. ) ;
#11520 = EDGE_LOOP ( 'NONE', ( #28821, #1136, #18908, #37271 ) ) ;
#11521 = ORIENTED_EDGE ( 'NONE', *, *, #8464, .F. ) ;
#11522 = DIRECTION ( 'NONE',  ( 1.000000000000000000, -1.288607544181256449E-16, 0.000000000000000000 ) ) ;
#11523 = CARTESIAN_POINT ( 'NONE',  ( 3.776803835208212501, 121.1194860566822626, 0.3725146398702260386 ) ) ;
#11524 = SHAPE_REPRESENTATION_RELATIONSHIP ( 'NONE' , 'NONE' ,  #26424, #38189 ) ;
#11525 = CARTESIAN_POINT ( 'NONE',  ( -6.537359847799236512, 121.1369950346570192, 0.6189803324213468683 ) ) ;
#11526 = DIRECTION ( 'NONE',  ( -4.017660918040594346E-17, 1.000000000000000000, 2.376309959284834438E-19 ) ) ;
#11527 = ADVANCED_FACE ( 'NONE', ( #21164 ), #25327, .F. ) ;
#11528 = CIRCLE ( 'NONE', #31933, 3.175000000000001155 ) ;
#11529 = CARTESIAN_POINT ( 'NONE',  ( 4.554470953189297511, 118.0726681490097860, -0.6231005214564631078 ) ) ;
#11530 = CARTESIAN_POINT ( 'NONE',  ( 11.27566272104525780, 154.5781333488962446, -1.670651684902623835 ) ) ;
#11531 = CARTESIAN_POINT ( 'NONE',  ( -6.715107731706678962, 119.1290971219625021, -1.270026890958220633 ) ) ;
#11532 = CARTESIAN_POINT ( 'NONE',  ( -5.924740142096584172, 65.21691166894066782, 1.270000000000005125 ) ) ;
#11533 = EDGE_CURVE ( 'NONE', #6038, #21991, #36925, .T. ) ;
#11534 = CARTESIAN_POINT ( 'NONE',  ( 4.074910602682932925, 118.2429491485453354, -0.1454311599470142491 ) ) ;
#11535 = CARTESIAN_POINT ( 'NONE',  ( 8.758948435532664334, 123.3024417045633498, -0.2233049321804337906 ) ) ;
#11536 = ORIENTED_EDGE ( 'NONE', *, *, #39798, .F. ) ;
#11537 = CARTESIAN_POINT ( 'NONE',  ( 2.857130780617909149, -14.87311083204414786, 4.269097905712053276 ) ) ;
#11538 = CARTESIAN_POINT ( 'NONE',  ( -4.980827880492125992, 117.4083494260662661, 0.8692259800077603016 ) ) ;
#11539 = CARTESIAN_POINT ( 'NONE',  ( -50.55264109715174214, 15.40887103991305018, 4.805487048261737115 ) ) ;
#11540 = CARTESIAN_POINT ( 'NONE',  ( 4.406646451516359697, -6.344046434980911364, 1.391598188203984288 ) ) ;
#11541 = CARTESIAN_POINT ( 'NONE',  ( 4.884089373684489033, 156.1188696671683260, 1.381267178739763457 ) ) ;
#11542 = CARTESIAN_POINT ( 'NONE',  ( -3.114615542158560846, 28.50392562220115877, 0.5887488407975547400 ) ) ;
#11543 = CARTESIAN_POINT ( 'NONE',  ( -1.441108623025377566, 106.3840144300045409, 5.062828720429449980 ) ) ;
#11544 = CARTESIAN_POINT ( 'NONE',  ( 0.3994026957563919789, 5.465888722076803319, 4.619092260001838923 ) ) ;
#11545 = CARTESIAN_POINT ( 'NONE',  ( 14.19780223135870045, 138.9094276006951247, 0.4095818057664821765 ) ) ;
#11546 = CIRCLE ( 'NONE', #33309, 0.3810000000000000053 ) ;
#11547 = CARTESIAN_POINT ( 'NONE',  ( 1.958624548881832350, -3.744965520567712147, -8.202033116754515518 ) ) ;
#11548 = CARTESIAN_POINT ( 'NONE',  ( -57.22211421646271390, 1.778355698664496609, -0.1074917508089587859 ) ) ;
#11549 = CARTESIAN_POINT ( 'NONE',  ( 8.779668897515529480, 117.8111319902365466, -0.2054863605742794086 ) ) ;
#11550 = CARTESIAN_POINT ( 'NONE',  ( 0.0006472084742443534513, 124.6436471961814476, -0.03238895860161133955 ) ) ;
#11551 = CARTESIAN_POINT ( 'NONE',  ( -19.05000000000000782, 71.11999999999999034, 5.715000000000000746 ) ) ;
#11552 = LINE ( 'NONE', #24535, #32246 ) ;
#11553 = CARTESIAN_POINT ( 'NONE',  ( -0.7326219338007132764, 37.28220708697721619, 2.048504824603447627 ) ) ;
#11554 = CARTESIAN_POINT ( 'NONE',  ( 8.274862188802355689, -1.658786094895864149, -1.630640499628306372 ) ) ;
#11555 = CARTESIAN_POINT ( 'NONE',  ( 0.3815321866612710888, 118.1588879786102524, 0.9088679235907958232 ) ) ;
#11556 = CARTESIAN_POINT ( 'NONE',  ( 3.174366308151882254, 63.33946620154573282, 0.06343139340882729404 ) ) ;
#11557 = DIRECTION ( 'NONE',  ( 5.188838149069472160E-16, -1.699382548006136559E-16, -1.000000000000000000 ) ) ;
#11558 = CARTESIAN_POINT ( 'NONE',  ( -11.66725022231030984, 55.24499999999999034, 5.016499999999999737 ) ) ;
#11559 = CARTESIAN_POINT ( 'NONE',  ( -9.710933996004797564, 118.1218853900603136, 0.2424195399123783012 ) ) ;
#11560 = EDGE_CURVE ( 'NONE', #24684, #26813, #4949, .T. ) ;
#11561 = ORIENTED_EDGE ( 'NONE', *, *, #22948, .T. ) ;
#11562 = CARTESIAN_POINT ( 'NONE',  ( -58.79341205368594814, 0.01963237121659078266, -0.1476394306258474176 ) ) ;
#11563 = EDGE_CURVE ( 'NONE', #5054, #36653, #37579, .T. ) ;
#11564 = ORIENTED_EDGE ( 'NONE', *, *, #34197, .F. ) ;
#11565 = CARTESIAN_POINT ( 'NONE',  ( -43.98070909378276383, 21.30087824701856647, -2.736222515986692194 ) ) ;
#11566 = CARTESIAN_POINT ( 'NONE',  ( -8.935197197525255319, 123.9063447689825779, -0.1785465045940570761 ) ) ;
#11567 = CARTESIAN_POINT ( 'NONE',  ( 4.578653272329702872, -15.42525073102989097, 4.254151796826286969 ) ) ;
#11568 = CARTESIAN_POINT ( 'NONE',  ( -10.51304382037013951, 120.0128241960130424, 1.064055063733757356 ) ) ;
#11569 = CARTESIAN_POINT ( 'NONE',  ( 14.77829941377241774, 121.3346631531286164, -0.7297537739211614749 ) ) ;
#11570 = CARTESIAN_POINT ( 'NONE',  ( 0.6590154617207463206, 19.50938314818779062, -4.574821423538240950 ) ) ;
#11571 = CARTESIAN_POINT ( 'NONE',  ( -22.75358200450901336, 150.3871190066015799, -0.9055542368224056560 ) ) ;
#11572 = CARTESIAN_POINT ( 'NONE',  ( -52.37404615337990776, 12.26367279239957320, -4.302067587320100195 ) ) ;
#11573 = ORIENTED_EDGE ( 'NONE', *, *, #40256, .T. ) ;
#11574 = CARTESIAN_POINT ( 'NONE',  ( -2.185546054340737232, 116.2009413105890019, -0.01666836221661271641 ) ) ;
#11575 = FACE_OUTER_BOUND ( 'NONE', #33594, .T. ) ;
#11576 = CARTESIAN_POINT ( 'NONE',  ( -9.357607378341853632, 155.0893615026619159, 1.530462696531121658 ) ) ;
#11577 = CARTESIAN_POINT ( 'NONE',  ( -51.57356029563064226, 13.43704833176837354, -4.363522926272087155 ) ) ;
#11578 = EDGE_CURVE ( 'NONE', #5098, #25709, #3584, .T. ) ;
#11579 = CARTESIAN_POINT ( 'NONE',  ( 2.387896358646802941, 119.0637060312156024, -0.6953999086667945750 ) ) ;
#11580 = CARTESIAN_POINT ( 'NONE',  ( -21.29237892510571584, 148.2102652567764380, -2.313897094871049553 ) ) ;
#11581 = CARTESIAN_POINT ( 'NONE',  ( -52.42133349025997546, 11.92692459785933679, -4.172736198742198255 ) ) ;
#11582 = EDGE_CURVE ( 'NONE', #10724, #2340, #11806, .T. ) ;
#11583 = B_SPLINE_CURVE_WITH_KNOTS ( 'NONE', 3,
 ( #1731, #37705, #15534, #4930, #31301, #8104, #38130, #14688 ),
 .UNSPECIFIED., .F., .F.,
 ( 4, 2, 2, 4 ),
 ( 0.000000000000000000, 0.2500000000000000000, 0.5000000000000000000, 1.000000000000000000 ),
 .UNSPECIFIED. ) ;
#11584 = CARTESIAN_POINT ( 'NONE',  ( 6.388910139315798986, 155.4084287100276072, -0.7748799927007736787 ) ) ;
#11585 = VERTEX_POINT ( 'NONE', #12015 ) ;
#11586 = CARTESIAN_POINT ( 'NONE',  ( -11.77984014550172631, 123.3160021321619695, -1.727726820665321128 ) ) ;
#11587 = CARTESIAN_POINT ( 'NONE',  ( 3.676215660907734328, -15.61639409997438221, 3.572853394304201569 ) ) ;
#11588 = ADVANCED_FACE ( 'NONE', ( #25010 ), #19028, .T. ) ;
#11589 = CARTESIAN_POINT ( 'NONE',  ( -4.491445922219573283, 118.1274274216726923, -0.6813552275993676188 ) ) ;
#11590 = CARTESIAN_POINT ( 'NONE',  ( -57.80205714066466527, 2.371715784325115095, -1.753227392946310470 ) ) ;
#11591 = CARTESIAN_POINT ( 'NONE',  ( -4.924473681474931475, 117.4782309372925795, 0.9294218393982265347 ) ) ;
#11592 = CARTESIAN_POINT ( 'NONE',  ( 17.91131452944944868, 148.1388135707062474, 2.335088068787735782 ) ) ;
#11593 = DIRECTION ( 'NONE',  ( -0.9454731675810332803, 0.3256999990547855828, -8.537024980200802097E-16 ) ) ;
#11594 = AXIS2_PLACEMENT_3D ( 'NONE', #3589, #26351, #26566 ) ;
#11595 = CARTESIAN_POINT ( 'NONE',  ( -7.218840658378264052, 2.017470825009220370, -4.342437029863850384 ) ) ;
#11596 = CARTESIAN_POINT ( 'NONE',  ( 1.615823435711507994, 156.2764358050213787, 0.4002269557471578865 ) ) ;
#11597 = CARTESIAN_POINT ( 'NONE',  ( -54.98111839650035648, 8.542840639972862249, -3.427624633821342304 ) ) ;
#11599 = ORIENTED_EDGE ( 'NONE', *, *, #37833, .T. ) ;
#11598 = CARTESIAN_POINT ( 'NONE',  ( -41.05189575270519242, 23.09451173561983950, -0.4656666666666720023 ) ) ;
#11600 = CARTESIAN_POINT ( 'NONE',  ( -2.011069428279017579, 117.9394519721141421, 1.285232015002204520 ) ) ;
#11601 = CIRCLE ( 'NONE', #35395, 0.2539999999999937863 ) ;
#11602 = CARTESIAN_POINT ( 'NONE',  ( -14.73199999999999932, 12.96416000000000146, 0.000000000000000000 ) ) ;
#11603 = CARTESIAN_POINT ( 'NONE',  ( -58.29601494275114959, -0.1585044380288253008, 0.03613930236862695350 ) ) ;
#11604 = CARTESIAN_POINT ( 'NONE',  ( -49.59816314059868603, 17.91649583374772092, 5.069000701391646935 ) ) ;
#11605 = CARTESIAN_POINT ( 'NONE',  ( -20.37188742667035157, 129.0035756037533758, -0.2165721192533106021 ) ) ;
#11606 = ORIENTED_EDGE ( 'NONE', *, *, #28977, .F. ) ;
#11607 = CARTESIAN_POINT ( 'NONE',  ( -48.00704091872448487, 20.04541143072568232, -5.176114466449832641 ) ) ;
#11608 = CARTESIAN_POINT ( 'NONE',  ( 5.931653563816388974, 121.3754646592592792, -0.09967777454307100160 ) ) ;
#11609 = CARTESIAN_POINT ( 'NONE',  ( -8.334503520420923905, 120.0709494557484049, 1.118110265123132718 ) ) ;
#11610 = EDGE_LOOP ( 'NONE', ( #22348, #29589, #21399 ) ) ;
#11611 = CARTESIAN_POINT ( 'NONE',  ( 0.2209820516631312570, 118.7629491485454025, -1.272057036781818251 ) ) ;
#11612 = CARTESIAN_POINT ( 'NONE',  ( 0.003550340867665223877, 156.3099534201614631, -0.1776735749810080256 ) ) ;
#11613 = CARTESIAN_POINT ( 'NONE',  ( 5.392686582494618186, -13.55334589181164695, 3.069518437182660264 ) ) ;
#11614 = CARTESIAN_POINT ( 'NONE',  ( -14.51588022701143643, 121.7426775721902175, 0.9381456983900906543 ) ) ;
#11615 = CARTESIAN_POINT ( 'NONE',  ( 2.026107803274938668, 117.3993837373488134, -1.369929326007458315 ) ) ;
#11616 = CARTESIAN_POINT ( 'NONE',  ( 16.84361796505724485, 155.2300590059875844, 0.4756075834919733514 ) ) ;
#11617 = CARTESIAN_POINT ( 'NONE',  ( 13.59117098933499790, 150.2425924485890505, 0.2715839415562140702 ) ) ;
#11618 = CARTESIAN_POINT ( 'NONE',  ( -5.019158082560326584, 117.3993830232448659, 0.7013206397503667366 ) ) ;
#11619 = CARTESIAN_POINT ( 'NONE',  ( -0.8868740923517060004, 23.60745955286466824, 0.4068859645678858938 ) ) ;
#11620 = CARTESIAN_POINT ( 'NONE',  ( -13.64397932274300551, 119.6379125180634446, -0.3727430486357817818 ) ) ;
#11621 = FACE_OUTER_BOUND ( 'NONE', #31979, .T. ) ;
#11622 = CARTESIAN_POINT ( 'NONE',  ( 12.69999999999999929, 11.53894877578616907, 1.555301434917138235E-15 ) ) ;
#11623 = ORIENTED_EDGE ( 'NONE', *, *, #32030, .F. ) ;
#11624 = CARTESIAN_POINT ( 'NONE',  ( 6.152576065035590069, 119.0783712746871572, 1.247159342819149863 ) ) ;
#11625 = CARTESIAN_POINT ( 'NONE',  ( -17.14500000000000313, 71.11999999999999034, -5.714999999999998970 ) ) ;
#11626 = CARTESIAN_POINT ( 'NONE',  ( 21.74891716461452518, 141.9756885651356413, 2.029123422127836029 ) ) ;
#11627 = CARTESIAN_POINT ( 'NONE',  ( -58.44555280191370628, -0.4200408777308817232, -0.3231375529350146159 ) ) ;
#11628 = CARTESIAN_POINT ( 'NONE',  ( 20.05916364549907982, 149.8444905389382882, -1.617669260345511173 ) ) ;
#11629 = CARTESIAN_POINT ( 'NONE',  ( 1.217031898716552707, 25.17763362506526192, -8.368877290174015826 ) ) ;
#11630 = CARTESIAN_POINT ( 'NONE',  ( -8.073283135001606325, 117.9965348323767671, -0.8851005009521593081 ) ) ;
#11631 = CARTESIAN_POINT ( 'NONE',  ( 4.936719870595172921, 117.6322946229582982, -0.7900978698212627327 ) ) ;
#11632 = AXIS2_PLACEMENT_3D ( 'NONE', #17230, #4686, #24038 ) ;
#11633 = EDGE_CURVE ( 'NONE', #34925, #11585, #22211, .T. ) ;
#11634 = CARTESIAN_POINT ( 'NONE',  ( 5.571761382372238280, 117.9391977826196296, 0.7470240521525302047 ) ) ;
#11635 = ORIENTED_EDGE ( 'NONE', *, *, #36593, .F. ) ;
#11636 = CARTESIAN_POINT ( 'NONE',  ( -13.04043193504470288, 133.9378623523624299, 0.05483593244790770094 ) ) ;
#11637 = CARTESIAN_POINT ( 'NONE',  ( -18.75244783997693787, 140.8526363637247982, -2.516729932275435289 ) ) ;
#11638 = CARTESIAN_POINT ( 'NONE',  ( 4.666472529085985421, -15.22678077218547799, 4.383143511210439769 ) ) ;
#11639 = AXIS2_PLACEMENT_3D ( 'NONE', #31982, #31559, #11752 ) ;
#11640 = DIRECTION ( 'NONE',  ( 6.829619984160660610E-15, 0.000000000000000000, 1.000000000000000000 ) ) ;
#11641 = CARTESIAN_POINT ( 'NONE',  ( -3.354700091392308181, 117.9496054330418104, -1.286735144063386738 ) ) ;
#11642 = B_SPLINE_CURVE_WITH_KNOTS ( 'NONE', 3,
 ( #10960, #20323, #20955, #36546, #7365, #17143, #984, #10752, #36754, #7573, #20534, #12172, #25781, #12999, #18756, #35382, #41791, #9193, #35181, #2815, #5801, #12589, #2608, #15567, #15774, #28779, #38584, #19183, #9812, #31766, #6416, #22569, #38789, #35599, #6624, #12792, #22778, #41580, #25578, #28361, #32188, #28572, #12388, #9393, #25375, #21948, #3022, #34979, #38380, #19387, #9600, #22150, #6007, #25168, #18969 ),
 .UNSPECIFIED., .F., .F.,
 ( 4, 2, 2, 2, 2, 1, 2, 2, 2, 2, 2, 1, 2, 2, 2, 2, 2, 1, 1, 2, 2, 2, 2, 2, 1, 2, 2, 2, 2, 4 ),
 ( 0.000000000000000000, 0.03125000000005594830, 0.06250000000011189660, 0.09375000000016779633, 0.1093750000001957601, 0.1171875000002130657, 0.1210937500002182976, 0.1250000000002235157, 0.1875000000003034240, 0.2187500000003434197, 0.2343750000003604617, 0.2421875000003690104, 0.2460937500003703704, 0.2500000000003717027, 0.3750000000004340972, 0.4375000000004619083, 0.4687500000004758416, 0.4843750000004827250, 0.4921875000004831135, 0.4960937500004862777, 0.5000000000004893863, 0.6250000000003956835, 0.6875000000003488321, 0.7187500000003254064, 0.7343750000003137490, 0.7421875000003078648, 0.7500000000003018696, 0.8750000000001509903, 0.9375000000000754952, 1.000000000000000000 ),
 .UNSPECIFIED. ) ;
#11643 = VERTEX_POINT ( 'NONE', #12855 ) ;
#11644 = CARTESIAN_POINT ( 'NONE',  ( 19.21961548592736690, 147.3692480224366079, 2.508364867928686071 ) ) ;
#11645 = FACE_OUTER_BOUND ( 'NONE', #1681, .T. ) ;
#11646 = CARTESIAN_POINT ( 'NONE',  ( -5.295281529786937114, 115.6909491485389054, -0.7215990444303079787 ) ) ;
#11647 = CARTESIAN_POINT ( 'NONE',  ( -2.327868625978157358, 124.9344662015457175, -0.04651635516647301821 ) ) ;
#11648 = CARTESIAN_POINT ( 'NONE',  ( -0.9165671635830696662, -12.81903285835614525, -8.372742598224451882 ) ) ;
#11649 = CARTESIAN_POINT ( 'NONE',  ( 16.28325953274104165, 146.1553843108282820, 1.442930602569015175 ) ) ;
#11650 = CARTESIAN_POINT ( 'NONE',  ( -4.796232024291369633, 115.6909491485453003, -1.474888944111601319 ) ) ;
#11651 = CARTESIAN_POINT ( 'NONE',  ( 22.30840772692673823, 150.5193240506149550, -0.5167903241875734244 ) ) ;
#11652 = CARTESIAN_POINT ( 'NONE',  ( 5.511275327887530828, 56.51500000000046242, -5.111309966001113203 ) ) ;
#11653 = CARTESIAN_POINT ( 'NONE',  ( -58.01159622203579858, 0.4793617641021541420, 0.8436046718122062194 ) ) ;
#11654 = CARTESIAN_POINT ( 'NONE',  ( -29.63955833213042013, 69.20431239923942712, -1.524000000000007127 ) ) ;
#11655 = VECTOR ( 'NONE', #14716, 1000.000000000000114 ) ;
#11656 = CARTESIAN_POINT ( 'NONE',  ( 1.975269416564897629, -15.10067923695700642, 5.832845082603782316 ) ) ;
#11657 = CARTESIAN_POINT ( 'NONE',  ( -4.297166465714638228, 118.2143479842866611, 0.3467644725669444261 ) ) ;
#11658 = CARTESIAN_POINT ( 'NONE',  ( 4.780914974771698134, 111.8766742162016357, -2.439331676452292097 ) ) ;
#11659 = VERTEX_POINT ( 'NONE', #41640 ) ;
#11660 = CARTESIAN_POINT ( 'NONE',  ( -48.38589991294942649, 19.15920805527091630, 5.452675306770309760 ) ) ;
#11661 = CARTESIAN_POINT ( 'NONE',  ( 6.194152875776375744, 119.6356763387034334, -1.001677016561595801 ) ) ;
#11663 = CARTESIAN_POINT ( 'NONE',  ( 4.159337697990636684, 118.2392943130565470, 0.3847892076047124688 ) ) ;
#11662 = VECTOR ( 'NONE', #16522, 1000.000000000000000 ) ;
#11664 = CARTESIAN_POINT ( 'NONE',  ( -16.05307823990510485, 146.0544122543811341, -1.176040581308521960 ) ) ;
#11665 = CARTESIAN_POINT ( 'NONE',  ( 4.886022116125724679, 117.7561648045584519, -0.7145573245312663024 ) ) ;
#11666 = CARTESIAN_POINT ( 'NONE',  ( 0.3903998909774342718, 117.9496051583923872, -1.393992266905087485 ) ) ;
#11667 = VERTEX_POINT ( 'NONE', #32456 ) ;
#11668 = CARTESIAN_POINT ( 'NONE',  ( -1.287880193524239658, 20.15907059199006923, -4.440276399826991849 ) ) ;
#11669 = CARTESIAN_POINT ( 'NONE',  ( -4.379744549753617378, 120.5100497556178567, -0.6885478749808131571 ) ) ;
#11670 = DIRECTION ( 'NONE',  ( -5.188838149069472160E-16, 1.699382548006136559E-16, 1.000000000000000000 ) ) ;
#11671 = CARTESIAN_POINT ( 'NONE',  ( -41.09670346151852982, 23.04688172093030474, 1.270085369932500763 ) ) ;
#11672 = LINE ( 'NONE', #11456, #35815 ) ;
#11673 = CARTESIAN_POINT ( 'NONE',  ( 7.793607028369248901, 122.5636234448803776, 0.3703801320152458887 ) ) ;
#11674 = CARTESIAN_POINT ( 'NONE',  ( 1.072590735131739414, 20.86836736082219801, 4.503669761903479341 ) ) ;
#11675 = CARTESIAN_POINT ( 'NONE',  ( 19.50329963654020915, 128.7319734376252143, 1.320013405138365181 ) ) ;
#11676 = CARTESIAN_POINT ( 'NONE',  ( -6.486711254249450261E-14, 72.48346620154573827, 1.207165459670006807E-19 ) ) ;
#11678 = CARTESIAN_POINT ( 'NONE',  ( 13.58393798013047871, 155.6725583577350278, -1.480266515874766542 ) ) ;
#11677 = CARTESIAN_POINT ( 'NONE',  ( 3.151249207183300260, -14.28495848352401332, 1.742053583190615207 ) ) ;
#11679 = CARTESIAN_POINT ( 'NONE',  ( -18.19397457907797744, 146.9188445454784357, 1.620492285849223446 ) ) ;
#11680 = AXIS2_PLACEMENT_3D ( 'NONE', #33742, #4566, #20926 ) ;
#11681 = CARTESIAN_POINT ( 'NONE',  ( 0.4015916885733669117, -14.54189033959780808, -0.8905040343298938899 ) ) ;
#11682 = CARTESIAN_POINT ( 'NONE',  ( -21.60506836338294789, 151.3813297165527274, -1.270904734852022377 ) ) ;
#11683 = CARTESIAN_POINT ( 'NONE',  ( 0.1924800537393606958, 19.99376482044840486, 0.9543378882872525226 ) ) ;
#11684 = ORIENTED_EDGE ( 'NONE', *, *, #42074, .F. ) ;
#11685 = B_SPLINE_CURVE_WITH_KNOTS ( 'NONE', 3,
 ( #29736, #17364, #36140, #10558, #36357, #20131, #20333, #23743, #13333, #33359, #16943, #23529, #23106, #6957, #1201, #19926, #14161 ),
 .UNSPECIFIED., .F., .F.,
 ( 4, 1, 1, 1, 1, 1, 1, 1, 1, 1, 1, 1, 1, 1, 4 ),
 ( 0.000000000000000000, 0.05527712972171117123, 0.1031936715418271255, 0.1452310937008415292, 0.1830547385316705356, 0.2184069929475541683, 0.2529008548920727018, 0.3331866173837648715, 0.4227704555254401253, 0.5212776283956739309, 0.6247903393790393833, 0.7282327622823181468, 0.8267193445215066383, 0.9169988606028186551, 1.000000000000000000 ),
 .UNSPECIFIED. ) ;
#11686 = CARTESIAN_POINT ( 'NONE',  ( -54.82379132704179625, 7.242239488055856711, 3.238872252923468587 ) ) ;
#11687 = CARTESIAN_POINT ( 'NONE',  ( -9.485477581651585055, 123.8597080710187015, 0.4105858232041853517 ) ) ;
#11688 = CARTESIAN_POINT ( 'NONE',  ( 2.458590490134419770, -15.31022926314896893, 5.890968354261565842 ) ) ;
#11689 = CARTESIAN_POINT ( 'NONE',  ( 1.452025732293782179, 120.0849730816093910, -0.4508766852696773908 ) ) ;
#11690 = ORIENTED_EDGE ( 'NONE', *, *, #19395, .F. ) ;
#11691 = CIRCLE ( 'NONE', #21851, 5.588000000000006295 ) ;
#11692 = CARTESIAN_POINT ( 'NONE',  ( 1.214457255922167134, 115.7029375523520116, 1.741465633879825781 ) ) ;
#11693 = CIRCLE ( 'NONE', #23222, 4.826000000000001400 ) ;
#11694 = CARTESIAN_POINT ( 'NONE',  ( 3.403332384622693052, -13.60094159685824877, 2.654810364998238192 ) ) ;
#11695 = CARTESIAN_POINT ( 'NONE',  ( -4.750525968156759760, 117.8920781161146181, -0.9101660372078754779 ) ) ;
#11696 = CARTESIAN_POINT ( 'NONE',  ( 11.06366964751653192, 128.0319838675845290, 0.1805508315534841424 ) ) ;
#11697 = ORIENTED_EDGE ( 'NONE', *, *, #27784, .F. ) ;
#11698 = CARTESIAN_POINT ( 'NONE',  ( 11.58042324368370046, 121.0393782313542346, 1.653871040030608697 ) ) ;
#11699 = CYLINDRICAL_SURFACE ( 'NONE', #9515, 0.2540000000000015024 ) ;
#11700 = DIRECTION ( 'NONE',  ( -0.9998004120163608288, -4.016384292689131511E-17, -0.01997839162482749342 ) ) ;
#11701 = CARTESIAN_POINT ( 'NONE',  ( 0.009748065369120871224, 159.5507987164374981, -0.4878330526048096361 ) ) ;
#11702 = CARTESIAN_POINT ( 'NONE',  ( 21.84047376210808267, 151.4369626909183637, -0.009531295849831044470 ) ) ;
#11703 = AXIS2_PLACEMENT_3D ( 'NONE', #5192, #27952, #2204 ) ;
#11704 = FACE_OUTER_BOUND ( 'NONE', #31053, .T. ) ;
#11705 = CARTESIAN_POINT ( 'NONE',  ( 1.637592558569015644, -15.41088763797304750, 5.642738181119684171 ) ) ;
#11706 = CARTESIAN_POINT ( 'NONE',  ( -6.654617103318593247E-14, 104.6144662015457243, 1.534725424433578570E-31 ) ) ;
#11707 = CARTESIAN_POINT ( 'NONE',  ( -6.059261036834472591, 56.51499999999997925, -4.547742611252458822 ) ) ;
#11708 = CARTESIAN_POINT ( 'NONE',  ( -4.845225939460884312, 117.8262844396378739, 0.6941112827358852932 ) ) ;
#11709 = EDGE_LOOP ( 'NONE', ( #5989, #3292, #22617, #23328 ) ) ;
#11710 = VERTEX_POINT ( 'NONE', #9661 ) ;
#11711 = DIRECTION ( 'NONE',  ( 0.3256999990547897461, 0.9454731675810318370, 0.000000000000000000 ) ) ;
#11712 = B_SPLINE_CURVE_WITH_KNOTS ( 'NONE', 3,
 ( #4184, #30346, #40172, #3766 ),
 .UNSPECIFIED., .F., .F.,
 ( 4, 4 ),
 ( 0.000000000000000000, 1.000000000000000000 ),
 .UNSPECIFIED. ) ;
#11713 = CARTESIAN_POINT ( 'NONE',  ( 3.124214023240655891, 118.2564054494065999, -0.7679563639302000588 ) ) ;
#11714 = CARTESIAN_POINT ( 'NONE',  ( -4.119305931990809633, 118.0988315448752530, -0.8046943418515851709 ) ) ;
#11715 = CARTESIAN_POINT ( 'NONE',  ( 4.831148843770026069, 117.6432307235636046, 1.088101262527759960 ) ) ;
#11716 = CARTESIAN_POINT ( 'NONE',  ( -23.69188486464780752, 78.08202335040543574, 1.269999999999993801 ) ) ;
#11717 = CARTESIAN_POINT ( 'NONE',  ( -0.9377939088481974661, 122.9246775559910390, 0.1697371007065933135 ) ) ;
#11718 = AXIS2_PLACEMENT_3D ( 'NONE', #22384, #35409, #1994 ) ;
#11719 = CARTESIAN_POINT ( 'NONE',  ( 4.349802767100347189, -10.92635770930747796, -1.576909098649299512 ) ) ;
#11720 = CYLINDRICAL_SURFACE ( 'NONE', #8805, 0.6350000000000014522 ) ;
#11721 = CARTESIAN_POINT ( 'NONE',  ( 5.586884702347364673, 87.97746620154572383, 0.1116392523995368424 ) ) ;
#11722 = CARTESIAN_POINT ( 'NONE',  ( 2.022490532284443088, -15.01207906941262671, 5.472131392975311925 ) ) ;
#11723 = CARTESIAN_POINT ( 'NONE',  ( 4.798759560707918759, 116.6039038697339549, -0.9352253033319916087 ) ) ;
#11724 = CARTESIAN_POINT ( 'NONE',  ( 17.14499999999999957, 71.11999999999999034, 5.016499999999999737 ) ) ;
#11725 = DIRECTION ( 'NONE',  ( -0.9998004120163610509, -4.016384292689131511E-17, -0.01997839162482749689 ) ) ;
#11726 = CARTESIAN_POINT ( 'NONE',  ( -1.708516274928095990, 115.7028613054959436, 1.661197570522961575 ) ) ;
#11727 = CARTESIAN_POINT ( 'NONE',  ( -4.544942180623752215, 12.81246518813932589, 0.8472608254572608910 ) ) ;
#11728 = ORIENTED_EDGE ( 'NONE', *, *, #11204, .T. ) ;
#11729 = CARTESIAN_POINT ( 'NONE',  ( 4.653890175952837716, 105.1215341841791258, -2.614083570717117944 ) ) ;
#11730 = CARTESIAN_POINT ( 'NONE',  ( 2.493951430369484523, -15.64112390455543711, 5.038688225235472551 ) ) ;
#11731 = CARTESIAN_POINT ( 'NONE',  ( -6.464497043865880421, 157.5392376370035095, 1.685792624679405716 ) ) ;
#11732 = CARTESIAN_POINT ( 'NONE',  ( -0.9510052327539034733, 17.61975311242802533, 0.2078495401503242801 ) ) ;
#11733 = CARTESIAN_POINT ( 'NONE',  ( -0.9148265087109853644, 12.81245955126885505, -0.3394028602373861392 ) ) ;
#11734 = ADVANCED_FACE ( 'NONE', ( #35663, #25639 ), #15622, .F. ) ;
#11735 = EDGE_CURVE ( 'NONE', #12494, #21058, #6271, .T. ) ;
#11736 = ORIENTED_EDGE ( 'NONE', *, *, #738, .F. ) ;
#11737 = TOROIDAL_SURFACE ( 'NONE', #8336, 5.080000000000005400, 0.5080000000000000071 ) ;
#11738 = VERTEX_POINT ( 'NONE', #18818 ) ;
#11739 = CARTESIAN_POINT ( 'NONE',  ( -4.293188133933578676, 27.89088472858528078, 0.5134395162472098484 ) ) ;
#11740 = CARTESIAN_POINT ( 'NONE',  ( 1.569003042721580865, 118.7759820277219944, 0.8276293794157989492 ) ) ;
#11741 = PRESENTATION_STYLE_ASSIGNMENT (( #40933 ) ) ;
#11742 = CARTESIAN_POINT ( 'NONE',  ( -10.15138120625600138, 123.9924233945428682, 0.7101534938561541166 ) ) ;
#11743 = CARTESIAN_POINT ( 'NONE',  ( -17.09258512000246455, 84.17916046765628835, 1.269999999999996243 ) ) ;
#11744 = CARTESIAN_POINT ( 'NONE',  ( 1.858891552337619935, -15.10179129218686178, 5.555419934288654993 ) ) ;
#11745 = CARTESIAN_POINT ( 'NONE',  ( 9.322612814602670994, 121.5662863950884400, -1.087844926965479742 ) ) ;
#11746 = CARTESIAN_POINT ( 'NONE',  ( -12.64856329662766043, 122.0451665396574725, -1.778165442619766834 ) ) ;
#11747 = DIRECTION ( 'NONE',  ( 1.011795553208986377E-16, 1.000000000000000000, -0.000000000000000000 ) ) ;
#11748 = CARTESIAN_POINT ( 'NONE',  ( 4.121223586692221552, 118.2429491485453497, -0.1829416065829389815 ) ) ;
#11749 = CARTESIAN_POINT ( 'NONE',  ( 6.491509040564920952, 121.7133186976561205, -0.1169240713195676962 ) ) ;
#11750 = ORIENTED_EDGE ( 'NONE', *, *, #10911, .F. ) ;
#11751 = CARTESIAN_POINT ( 'NONE',  ( 1.824654213811243819, -15.25386490109567639, 5.420715704377902178 ) ) ;
#11752 = DIRECTION ( 'NONE',  ( -1.000000000000000000, 0.000000000000000000, 0.000000000000000000 ) ) ;
#11753 = TOROIDAL_SURFACE ( 'NONE', #27382, 0.7620000000000000107, 0.2540000000000000036 ) ;
#11754 = CARTESIAN_POINT ( 'NONE',  ( -58.41956937744257061, -0.3672969284060638717, 0.3776070891698000143 ) ) ;
#11755 = CARTESIAN_POINT ( 'NONE',  ( 2.913282581332740762, -14.11548038430587937, -3.586046950971230274 ) ) ;
#11756 = CARTESIAN_POINT ( 'NONE',  ( 10.14627733936753451, 123.6566696788710686, 1.220144418243291229 ) ) ;
#11757 = CARTESIAN_POINT ( 'NONE',  ( -2.818619619938098175, 29.34630912614251130, 1.292122882726251420 ) ) ;
#11758 = CARTESIAN_POINT ( 'NONE',  ( -2.169980103648603720, 106.6933082031156772, 4.882050113528205948 ) ) ;
#11759 = AXIS2_PLACEMENT_3D ( 'NONE', #40441, #15682, #34457 ) ;
#11760 = CARTESIAN_POINT ( 'NONE',  ( -4.609222696788063622, 3.091975128091568159, 0.4746723485708761459 ) ) ;
#11761 = CARTESIAN_POINT ( 'NONE',  ( -0.01249116623180958861, 38.87185441664305330, -1.227828225846576693 ) ) ;
#11762 = ADVANCED_FACE ( 'NONE', ( #41853 ), #19242, .F. ) ;
#11763 = CARTESIAN_POINT ( 'NONE',  ( -8.165053131321412749, -1.372107735949496421, -2.092221094348168275 ) ) ;
#11764 = CARTESIAN_POINT ( 'NONE',  ( -57.34787435976329562, 1.552391619547732748, -0.09937746155961837968 ) ) ;
#11765 = CARTESIAN_POINT ( 'NONE',  ( 5.538936621065253085, 116.8894077038538768, -0.3445561300999038790 ) ) ;
#11766 = CARTESIAN_POINT ( 'NONE',  ( -1.058386756517351923, 124.8229041592835387, -0.03077316225166099040 ) ) ;
#11767 = DIRECTION ( 'NONE',  ( -1.000000000000000000, 0.000000000000000000, 0.000000000000000000 ) ) ;
#11768 = CARTESIAN_POINT ( 'NONE',  ( 4.300553167417687561, 27.50566818391071422, -1.719522505244270860 ) ) ;
#11769 = CARTESIAN_POINT ( 'NONE',  ( 0.5436740362654144398, 117.9394487757135295, 1.407118881397579457 ) ) ;
#11770 = CARTESIAN_POINT ( 'NONE',  ( 18.13811525448111439, 9.293884745518885993, 0.000000000000000000 ) ) ;
#11771 = CARTESIAN_POINT ( 'NONE',  ( -29.94429436251954613, 71.80236127745905605, -1.270000000000007345 ) ) ;
#11772 = CARTESIAN_POINT ( 'NONE',  ( 0.3819982885357794955, 122.2435587914033022, -0.2867773152523557245 ) ) ;
#11773 = CARTESIAN_POINT ( 'NONE',  ( -13.30261597551697150, 156.9705208988102640, 0.2305920065817563536 ) ) ;
#11774 = VERTEX_POINT ( 'NONE', #25223 ) ;
#11775 = CARTESIAN_POINT ( 'NONE',  ( -58.69054519303719530, 0.2722345423086247607, -0.6021937201626393898 ) ) ;
#11776 = VERTEX_POINT ( 'NONE', #31826 ) ;
#11777 = LINE ( 'NONE', #20727, #41689 ) ;
#11778 = CIRCLE ( 'NONE', #30812, 0.2539999999999989488 ) ;
#11779 = CARTESIAN_POINT ( 'NONE',  ( -8.041889123127157646, 122.8518031662551948, -0.1606960833125206101 ) ) ;
#11780 = CARTESIAN_POINT ( 'NONE',  ( 2.462693652799142541, -15.54209007114785912, 5.820364621994587040 ) ) ;
#11781 = CARTESIAN_POINT ( 'NONE',  ( -2.800559387825789948, 158.6924860557018064, 1.442603686385967254 ) ) ;
#11782 = CARTESIAN_POINT ( 'NONE',  ( 22.40052491088791697, 148.4347612714453248, -0.9998933253014313793 ) ) ;
#11783 = CARTESIAN_POINT ( 'NONE',  ( -1.756104463947763206, 14.33678105357426702, 4.288642365192034234 ) ) ;
#11784 = CARTESIAN_POINT ( 'NONE',  ( -2.814065556059573314, 116.6946238705719594, -0.3036003272628903238 ) ) ;
#11785 = CARTESIAN_POINT ( 'NONE',  ( -51.00929282542724508, 14.63754895018605140, -4.688694305049216915 ) ) ;
#11786 = ORIENTED_EDGE ( 'NONE', *, *, #18115, .T. ) ;
#11787 = CARTESIAN_POINT ( 'NONE',  ( -2.183620640279838376, 116.1905378774015105, -0.03043059125181128352 ) ) ;
#11788 = CARTESIAN_POINT ( 'NONE',  ( -10.18297664959815663, 77.66688486464208552, 1.270000000000000906 ) ) ;
#11789 = CARTESIAN_POINT ( 'NONE',  ( -1.409223554827573999, 119.7856413326322667, 0.5222593444346083080 ) ) ;
#11790 = CARTESIAN_POINT ( 'NONE',  ( -56.17496734581288109, 4.395220231953922863, -2.356759703232587100 ) ) ;
#11791 = CARTESIAN_POINT ( 'NONE',  ( 11.67114148714781940, 122.1450671466348439, -1.284540048876763096 ) ) ;
#11792 = CARTESIAN_POINT ( 'NONE',  ( -7.848884907109314746, 118.8455990504009492, -1.250143668394028129 ) ) ;
#11793 = CARTESIAN_POINT ( 'NONE',  ( -56.78650302187183740, 3.241477563879227475, -2.205756828360271093 ) ) ;
#11794 = VECTOR ( 'NONE', #15484, 1000.000000000000000 ) ;
#11795 = EDGE_CURVE ( 'NONE', #30484, #39372, #34862, .T. ) ;
#11796 = CARTESIAN_POINT ( 'NONE',  ( 16.29799532358056524, 145.9442052555630767, -0.7927408685852873615 ) ) ;
#11797 = EDGE_LOOP ( 'NONE', ( #35754, #14813, #3615, #15345 ) ) ;
#11798 = CARTESIAN_POINT ( 'NONE',  ( -10.71425622041622994, 122.7614441063800399, -1.568315134061840865 ) ) ;
#11799 = B_SPLINE_CURVE_WITH_KNOTS ( 'NONE', 3,
 ( #39635, #10648, #20430, #33035, #14051, #1505, #14252, #27055, #30452, #4076, #27260, #7050, #3863, #7470, #17452, #668, #14460, #16827, #33457, #29830, #13636, #7260, #40063, #40275, #30033, #20220, #39852, #37069, #17249, #33246, #11070, #23194, #36649, #23629, #17035, #10855 ),
 .UNSPECIFIED., .F., .F.,
 ( 4, 2, 2, 2, 2, 2, 2, 2, 2, 2, 2, 2, 2, 2, 2, 2, 2, 4 ),
 ( 0.01468215474677663467, 0.01563221235945116278, 0.01658226997212569609, 0.01705729877846295928, 0.01753232758480022246, 0.01848238519747474884, 0.01943244281014927521, 0.02038250042282380159, 0.02133255803549833143, 0.02228261564817285781, 0.02323267326084738418, 0.02418273087352190709, 0.02513278848619643693, 0.02608284609887095984, 0.02703290371154548968, 0.02798296132422001606, 0.02893301893689454243, 0.02988307654956906881 ),
 .UNSPECIFIED. ) ;
#11800 = CARTESIAN_POINT ( 'NONE',  ( 4.222520559145931607, -15.42613134656034646, 1.120547993087879446 ) ) ;
#11801 = CARTESIAN_POINT ( 'NONE',  ( -4.516505043337477154, 118.0894658202221592, -0.7769319744564929797 ) ) ;
#11802 = CARTESIAN_POINT ( 'NONE',  ( -58.20820809768403592, 1.420579653404085985, -1.355822160094614759 ) ) ;
#11803 = CARTESIAN_POINT ( 'NONE',  ( -4.901356651777482476, 117.4105916379840266, 0.9668049386046483340 ) ) ;
#11804 = CARTESIAN_POINT ( 'NONE',  ( 9.288997298956278570, 155.0893615026619159, 1.903066234436351145 ) ) ;
#11805 = ADVANCED_FACE ( 'NONE', ( #26053 ), #23925, .T. ) ;
#11806 = LINE ( 'NONE', #31403, #6980 ) ;
#11807 = CONICAL_SURFACE ( 'NONE', #20647, 13.46199999999999619, 0.7853981633974497223 ) ;
#11808 = CARTESIAN_POINT ( 'NONE',  ( 7.466160517099046601, -1.205741384250370363, -3.973931221679563919 ) ) ;
#11809 = CARTESIAN_POINT ( 'NONE',  ( 2.922188055539069573, 156.0861408873597327, 0.2775485887099104487 ) ) ;
#11810 = DIRECTION ( 'NONE',  ( -1.000000000000000000, 0.000000000000000000, 0.000000000000000000 ) ) ;
#11811 = EDGE_CURVE ( 'NONE', #15919, #11643, #35875, .T. ) ;
#11813 = ORIENTED_EDGE ( 'NONE', *, *, #12782, .F. ) ;
#11812 = CARTESIAN_POINT ( 'NONE',  ( -42.83068693079387401, 21.70476352389080787, -1.889833665869970369 ) ) ;
#11814 = CARTESIAN_POINT ( 'NONE',  ( -3.414070525044812676, 117.3993835098938661, 1.238193295900473334 ) ) ;
#11815 = CARTESIAN_POINT ( 'NONE',  ( 4.722564864159155995, 118.7629491485453741, 0.9939262365100323127 ) ) ;
#11816 = AXIS2_PLACEMENT_3D ( 'NONE', #1723, #39862, #13859 ) ;
#11817 = ADVANCED_FACE ( 'NONE', ( #18610 ), #9237, .T. ) ;
#11818 = CARTESIAN_POINT ( 'NONE',  ( -58.15296624161964445, 0.1186235457594081444, 0.2061892363119880722 ) ) ;
#11819 = CARTESIAN_POINT ( 'NONE',  ( -50.06058399760020450, 19.37794936593257589, 3.106418048087394634 ) ) ;
#11820 = CARTESIAN_POINT ( 'NONE',  ( -16.83721787035681317, 155.2408147041404050, -0.1288212628531381632 ) ) ;
#11821 = ORIENTED_EDGE ( 'NONE', *, *, #15383, .F. ) ;
#11822 = CARTESIAN_POINT ( 'NONE',  ( -47.68734114412297487, 23.26096984540084023, -2.152999274035564792 ) ) ;
#11823 = CARTESIAN_POINT ( 'NONE',  ( 7.931070413917881368, 121.9907963680717558, -0.6304219912953731297 ) ) ;
#11824 = CARTESIAN_POINT ( 'NONE',  ( -7.845668857088636372, 122.3864107004520889, 0.3364293298510350194 ) ) ;
#11825 = AXIS2_PLACEMENT_3D ( 'NONE', #39426, #32606, #29409 ) ;
#11826 = ORIENTED_EDGE ( 'NONE', *, *, #3029, .F. ) ;
#11827 = CARTESIAN_POINT ( 'NONE',  ( 0.3836050358042789599, 115.7029491485453292, -1.750603908414250176 ) ) ;
#11829 = CIRCLE ( 'NONE', #20665, 0.5080000000000002292 ) ;
#11828 = CARTESIAN_POINT ( 'NONE',  ( -15.41061421316654823, 147.8340308814284754, -0.6362464400602065862 ) ) ;
#11830 = CARTESIAN_POINT ( 'NONE',  ( 5.123467091704872800, -13.13098499675426112, 2.859697440480786668 ) ) ;
#11831 = CARTESIAN_POINT ( 'NONE',  ( -13.99438190394165282, 121.2764344996515717, 0.9244547817413872881 ) ) ;
#11832 = DIRECTION ( 'NONE',  ( 9.627370216492862708E-17, 1.000000000000000000, -0.000000000000000000 ) ) ;
#11833 = CARTESIAN_POINT ( 'NONE',  ( 23.32994265436196457, 149.0590277239482475, 0.6203886826157013479 ) ) ;
#11834 = CARTESIAN_POINT ( 'NONE',  ( 9.104209967887914701, 153.9432936505793066, 0.1819237819739444872 ) ) ;
#11835 = DIRECTION ( 'NONE',  ( 0.3582377630123937395, -0.9336303900108844367, -4.972540365716860457E-16 ) ) ;
#11836 = CARTESIAN_POINT ( 'NONE',  ( 0.8015440831811396771, 19.08345756868062892, -0.5584349385947994238 ) ) ;
#11837 = CARTESIAN_POINT ( 'NONE',  ( -6.898502017095935912, 117.1694300671557727, -0.1814136226821929376 ) ) ;
#11838 = CARTESIAN_POINT ( 'NONE',  ( 5.008434261519718156, 117.3975399490705342, -0.7758999597088642730 ) ) ;
#11839 = DIRECTION ( 'NONE',  ( -0.7548010569845218232, -0.6559537821943318692, 8.877513919532275149E-16 ) ) ;
#11840 = ADVANCED_FACE ( 'NONE', ( #5184 ), #31777, .T. ) ;
#11841 = EDGE_LOOP ( 'NONE', ( #13671, #25984, #9287, #6100 ) ) ;
#11842 = CARTESIAN_POINT ( 'NONE',  ( -8.556400685085039370, 118.9707913172079543, 0.9328110640611807503 ) ) ;
#11843 = CARTESIAN_POINT ( 'NONE',  ( -1.997604609866625580, -12.39122764300357105, -4.168859717980781809 ) ) ;
#11844 = CARTESIAN_POINT ( 'NONE',  ( 21.88420111187364725, 149.4141677464492091, 2.022441453707984227 ) ) ;
#11845 = CARTESIAN_POINT ( 'NONE',  ( -58.63679809531399201, -0.7731007215647841546, 1.400195018401728875E-12 ) ) ;
#11846 = CARTESIAN_POINT ( 'NONE',  ( 12.47042458399945986, 121.5863879130357503, -1.220378502514999797 ) ) ;
#11847 = AXIS2_PLACEMENT_3D ( 'NONE', #37913, #28108, #18300 ) ;
#11848 = CARTESIAN_POINT ( 'NONE',  ( 4.770677904581660300, 21.51973835935561041, 6.970347630165958819 ) ) ;
#11849 = CARTESIAN_POINT ( 'NONE',  ( -14.16249321059125599, 121.1589565784038456, -1.397539518993202723 ) ) ;
#11850 = CARTESIAN_POINT ( 'NONE',  ( 4.908480440954034130, 117.5478834382789302, -0.9161991286228470255 ) ) ;
#11851 = CARTESIAN_POINT ( 'NONE',  ( 7.277551686224362548, 123.0424313102424492, 0.2142739940110135466 ) ) ;
#11852 = ORIENTED_EDGE ( 'NONE', *, *, #21925, .F. ) ;
#11853 = CARTESIAN_POINT ( 'NONE',  ( -9.140193528981251703, 153.9061766533773152, 0.01708403265280381694 ) ) ;
#11854 = CARTESIAN_POINT ( 'NONE',  ( 0.01133701094395666610, 119.0130636887059410, -0.5673503866435168908 ) ) ;
#11855 = CARTESIAN_POINT ( 'NONE',  ( 3.423347803338410156, -15.46749709811699702, 5.412694551837634371 ) ) ;
#11856 = LINE ( 'NONE', #15251, #41751 ) ;
#11857 = EDGE_CURVE ( 'NONE', #41093, #19493, #1545, .T. ) ;
#11858 = CARTESIAN_POINT ( 'NONE',  ( -4.297733157312593200, 118.1651005001141925, -0.6725186956912113656 ) ) ;
#11859 = EDGE_CURVE ( 'NONE', #8945, #17215, #28729, .T. ) ;
#11860 = EDGE_LOOP ( 'NONE', ( #25357, #41608, #19765, #24136, #12824, #33750, #8311, #10853, #16518, #5121 ) ) ;
#11861 = CARTESIAN_POINT ( 'NONE',  ( 4.079782966556019908, 157.3082466949932723, 1.825029598092313909 ) ) ;
#11862 = DIRECTION ( 'NONE',  ( -0.8745520943968235761, 0.4849315768086558398, -4.268512490100410909E-16 ) ) ;
#11863 = DIRECTION ( 'NONE',  ( 5.188838149069472160E-16, -1.699382548006136559E-16, -1.000000000000000000 ) ) ;
#11864 = CARTESIAN_POINT ( 'NONE',  ( -0.7355314204969178871, 116.0160817474902331, 1.626749668116675318 ) ) ;
#11865 = CARTESIAN_POINT ( 'NONE',  ( -4.948315225313974608, -9.142465695005178361, 6.828157318318492486 ) ) ;
#11866 = CARTESIAN_POINT ( 'NONE',  ( 12.05573777011642100, 128.3964238929853252, 1.202367467897996089 ) ) ;
#11867 = CARTESIAN_POINT ( 'NONE',  ( -43.93316818929329770, 24.49458088220322338, -1.524000000000007349 ) ) ;
#11868 = CARTESIAN_POINT ( 'NONE',  ( 16.51027305157931480, 155.2380866766625047, -0.5525915368032876529 ) ) ;
#11869 = CARTESIAN_POINT ( 'NONE',  ( 5.223971174379742344, 56.51500000000003610, -4.542495777410184843 ) ) ;
#11870 = CARTESIAN_POINT ( 'NONE',  ( -58.31137634086686461, -0.1683406079603727845, 0.3070011007334173536 ) ) ;
#11871 = CARTESIAN_POINT ( 'NONE',  ( -4.556757383386185190, 31.49269130883712720, -0.6906699653381264126 ) ) ;
#11872 = ADVANCED_FACE ( 'NONE', ( #38797 ), #21745, .F. ) ;
#11873 = CARTESIAN_POINT ( 'NONE',  ( 2.009495809369670649, -15.14277677434764335, 5.899592854099827477 ) ) ;
#11874 = CARTESIAN_POINT ( 'NONE',  ( -4.250218791031737275, 118.2249388686620080, 0.3102279370716315432 ) ) ;
#11875 = CARTESIAN_POINT ( 'NONE',  ( -23.34372044207216845, 149.0681261006882039, -0.4664630893996629113 ) ) ;
#11876 = ORIENTED_EDGE ( 'NONE', *, *, #41268, .T. ) ;
#11877 = CARTESIAN_POINT ( 'NONE',  ( -54.32300027520380326, 9.724537220608771904, 3.743864951777626349 ) ) ;
#11878 = CARTESIAN_POINT ( 'NONE',  ( -6.145739716626447802, 119.6364497148305901, -1.247725477666507654 ) ) ;
#11879 = CARTESIAN_POINT ( 'NONE',  ( -5.302405987100971885, 104.6144662015457101, 1.270606870302479541 ) ) ;
#11880 = CARTESIAN_POINT ( 'NONE',  ( 4.357495859860891940, 118.1846395343606275, 0.6082252339746802017 ) ) ;
#11881 = CARTESIAN_POINT ( 'NONE',  ( -15.79391552826349354, 147.6293441119438512, -1.163731531224506677 ) ) ;
#11882 = DIRECTION ( 'NONE',  ( 5.188838149069472160E-16, -1.699382548006136559E-16, -1.000000000000000000 ) ) ;
#11883 = CARTESIAN_POINT ( 'NONE',  ( 15.97340373827820947, 121.0409387471171101, 0.3191866212789526425 ) ) ;
#11884 = ORIENTED_EDGE ( 'NONE', *, *, #13594, .T. ) ;
#11885 = CARTESIAN_POINT ( 'NONE',  ( -1.648064503646425649, 29.87956589480163316, -4.325937074807028715 ) ) ;
#11886 = CARTESIAN_POINT ( 'NONE',  ( -29.57045817498815410, 58.76046099843313897, 1.523999999999994026 ) ) ;
#11887 = CARTESIAN_POINT ( 'NONE',  ( 5.008579095262371439, 117.3966161975143052, -0.7759206765000108419 ) ) ;
#11888 = CARTESIAN_POINT ( 'NONE',  ( -41.09676540851936011, 23.04694042099051998, 1.523999999999990917 ) ) ;
#11889 = LINE ( 'NONE', #15070, #14722 ) ;
#11890 = CARTESIAN_POINT ( 'NONE',  ( 7.788256506714744454, 122.5981892255041572, 0.2834234761349876397 ) ) ;
#11891 = CARTESIAN_POINT ( 'NONE',  ( -1.535301415185580609, 19.99377045568717293, 4.360315235486975638 ) ) ;
#11892 = CARTESIAN_POINT ( 'NONE',  ( 12.99089357651411980, 156.9259531928012734, 1.181820989919032838 ) ) ;
#11893 = CARTESIAN_POINT ( 'NONE',  ( -4.831223284439005283, 104.6144662015457669, -0.2225614094029600976 ) ) ;
#11895 = CARTESIAN_POINT ( 'NONE',  ( 16.85638304633359752, 153.6818489539412553, -1.479736204719017900 ) ) ;
#11894 = CARTESIAN_POINT ( 'NONE',  ( 3.162461164278121739, -14.57801340048104777, 3.369881103115548893 ) ) ;
#11896 = CARTESIAN_POINT ( 'NONE',  ( -14.24002733280072164, 152.6618899727951089, 1.673933364105639088 ) ) ;
#11897 = CARTESIAN_POINT ( 'NONE',  ( 4.064150447026247726, 23.66704930264554818, -2.198397014704132513 ) ) ;
#11898 = CARTESIAN_POINT ( 'NONE',  ( -22.95323918608241343, 146.5883926500602001, -1.439717189780889584 ) ) ;
#11899 = CARTESIAN_POINT ( 'NONE',  ( -0.3594991891230457370, 15.46976683256975704, -0.9053751552070300468 ) ) ;
#11900 = VERTEX_POINT ( 'NONE', #32198 ) ;
#11901 = CARTESIAN_POINT ( 'NONE',  ( -56.40094345217906380, 3.567796355414390330, 1.062368598836890499 ) ) ;
#11902 = CARTESIAN_POINT ( 'NONE',  ( -6.492529462933222639, 121.6679077367135591, 0.1901135952749838376 ) ) ;
#11903 = CARTESIAN_POINT ( 'NONE',  ( 5.545296128261989033, -13.31524510490228508, 2.629257322947794684 ) ) ;
#11904 = CARTESIAN_POINT ( 'NONE',  ( 7.932268303790880992, 121.8456834504061845, -0.6952039612942494395 ) ) ;
#11905 = EDGE_LOOP ( 'NONE', ( #37868, #7292, #13226, #7904 ) ) ;
#11906 = CARTESIAN_POINT ( 'NONE',  ( 0.6559343604812126749, 115.7031630020738504, 1.758495348668634772 ) ) ;
#11907 = ORIENTED_EDGE ( 'NONE', *, *, #8919, .F. ) ;
#11908 = CARTESIAN_POINT ( 'NONE',  ( -4.765159595197983933, 117.6707466944635456, -1.115707916067754546 ) ) ;
#11909 = CARTESIAN_POINT ( 'NONE',  ( 8.831233598306480914, 123.6950213215744583, 0.09329271932673280365 ) ) ;
#11911 = ORIENTED_EDGE ( 'NONE', *, *, #8269, .F. ) ;
#11910 = VECTOR ( 'NONE', #21853, 1000.000000000000000 ) ;
#11912 = CARTESIAN_POINT ( 'NONE',  ( 12.21120734956418019, 121.7247091083657153, 1.742548127100890243 ) ) ;
#11913 = CARTESIAN_POINT ( 'NONE',  ( -5.861642722916909243, 64.54502714855203749, 1.270000000000005347 ) ) ;
#11914 = PLANE ( 'NONE',  #4858 ) ;
#11915 = CARTESIAN_POINT ( 'NONE',  ( 0.02400040557466870741, 156.7459281804771365, -1.201078436782489378 ) ) ;
#11916 = CARTESIAN_POINT ( 'NONE',  ( 10.78032506485370945, 157.9328640892066460, -0.04097195671286529839 ) ) ;
#11917 = FACE_OUTER_BOUND ( 'NONE', #29552, .T. ) ;
#11918 = CARTESIAN_POINT ( 'NONE',  ( 2.058562980619487615, -15.15559995322061937, 5.883026903270092589 ) ) ;
#11919 = CARTESIAN_POINT ( 'NONE',  ( 12.21488373879589240, 17.14499999999999957, 5.016499999999999737 ) ) ;
#11920 = CARTESIAN_POINT ( 'NONE',  ( -6.442348895218290093E-14, 63.84746620154572838, 4.408874939877717575E-29 ) ) ;
#11921 = CARTESIAN_POINT ( 'NONE',  ( -4.657921323837626915, 117.9598333327476638, 0.7454012569311468939 ) ) ;
#11922 = ORIENTED_EDGE ( 'NONE', *, *, #38918, .T. ) ;
#11923 = ORIENTED_EDGE ( 'NONE', *, *, #30489, .T. ) ;
#11924 = CARTESIAN_POINT ( 'NONE',  ( -0.02551629667440783247, 118.7629491485454025, 1.276939826302096348 ) ) ;
#11925 = CARTESIAN_POINT ( 'NONE',  ( 2.764682666223415630, 117.8403247707871628, -0.7160347503476400810 ) ) ;
#11926 = CARTESIAN_POINT ( 'NONE',  ( -0.4858112859843613518, 106.1608668108878817, -5.224277761219202176 ) ) ;
#11927 = CARTESIAN_POINT ( 'NONE',  ( 4.851132313076204738, 117.6731831347222794, 1.041893731173013204 ) ) ;
#11928 = CARTESIAN_POINT ( 'NONE',  ( -4.612970356601876709, 117.9306742281530660, -0.9648483343165797921 ) ) ;
#11929 = CARTESIAN_POINT ( 'NONE',  ( -0.9632506926928976476, 123.2612876230388395, 0.1349244037310163846 ) ) ;
#11930 = CARTESIAN_POINT ( 'NONE',  ( 0.4343283552818534288, -9.202337043772711667, -4.603842121470758997 ) ) ;
#11931 = CARTESIAN_POINT ( 'NONE',  ( -18.88948446928058544, 80.17638627449419175, -1.270000000000003348 ) ) ;
#11932 = CARTESIAN_POINT ( 'NONE',  ( -10.84307050033138431, 78.30450799593342026, -1.269999999999998685 ) ) ;
#11933 = CARTESIAN_POINT ( 'NONE',  ( 3.537338181458673070, -13.91857904597952533, 4.048280000481319973 ) ) ;
#11934 = CARTESIAN_POINT ( 'NONE',  ( 2.376338430377524347, 108.4767889311100362, -4.155189222081930644 ) ) ;
#11935 = CARTESIAN_POINT ( 'NONE',  ( -15.22212811258888898, 150.6904849259475441, -2.083262412922771922 ) ) ;
#11936 = CARTESIAN_POINT ( 'NONE',  ( 6.079889189570776509, 121.4459138077559714, 0.1214906566337395633 ) ) ;
#11937 = DIRECTION ( 'NONE',  ( -0.8745520943968250194, 0.4849315768086532863, -5.361993529360574930E-16 ) ) ;
#11938 = CIRCLE ( 'NONE', #9900, 0.2539999999999990599 ) ;
#11939 = CARTESIAN_POINT ( 'NONE',  ( -1.821252105156915713, 115.7029441824943063, 1.652972720107705573 ) ) ;
#11940 = CARTESIAN_POINT ( 'NONE',  ( -0.9211762648548540433, 10.43857344512876040, -4.529598961101950927 ) ) ;
#11942 = VERTEX_POINT ( 'NONE', #34771 ) ;
#11941 = CARTESIAN_POINT ( 'NONE',  ( 22.39330865153371874, 150.7562895891929031, 1.036336034128335415 ) ) ;
#11943 = CARTESIAN_POINT ( 'NONE',  ( 3.944401187668185038, 104.6144662015587983, -3.607510279707207168 ) ) ;
#11944 = CARTESIAN_POINT ( 'NONE',  ( 4.191701569836151720, -15.46661069841161229, 1.593937231346424843 ) ) ;
#11945 = CARTESIAN_POINT ( 'NONE',  ( -13.45896140341262637, 123.7870877700634509, 1.380644293323453065 ) ) ;
#11946 = CARTESIAN_POINT ( 'NONE',  ( -0.9667957141098567631, 26.69201124214932719, -0.1227653459084327853 ) ) ;
#11947 = CARTESIAN_POINT ( 'NONE',  ( 0.8487236205744517203, 17.35912690172634143, 0.4866769997786373203 ) ) ;
#11948 = ORIENTED_EDGE ( 'NONE', *, *, #41205, .F. ) ;
#11949 = ORIENTED_EDGE ( 'NONE', *, *, #30623, .F. ) ;
#11950 = CARTESIAN_POINT ( 'NONE',  ( -11.05715273818225342, 82.67346420587206524, 1.269999999999999796 ) ) ;
#11951 = CARTESIAN_POINT ( 'NONE',  ( 1.507062556099364459, 116.9323294830472122, 1.352967057238088300 ) ) ;
#11952 = CARTESIAN_POINT ( 'NONE',  ( -10.20798870728745200, 124.0743415861677903, 0.7134647857254747816 ) ) ;
#11953 = CARTESIAN_POINT ( 'NONE',  ( -19.33375693323417011, 80.42273151551299293, -1.270000000000003570 ) ) ;
#11954 = CARTESIAN_POINT ( 'NONE',  ( 3.666546702136318725, -13.72720857325485078, 3.759896688191319836 ) ) ;
#11955 = CARTESIAN_POINT ( 'NONE',  ( 0.9295719194792341211, 157.1975648536147787, -1.475660455335214616 ) ) ;
#11956 = CARTESIAN_POINT ( 'NONE',  ( -0.4360227397042136244, 118.4074432378348689, -0.6062663470103504260 ) ) ;
#11957 = CARTESIAN_POINT ( 'NONE',  ( 12.87096146653068196, 58.93153423982063543, -10.60403923708992835 ) ) ;
#11958 = CARTESIAN_POINT ( 'NONE',  ( -4.897950286213627713, 117.7356713384708087, 0.7215056066125844492 ) ) ;
#11959 = CARTESIAN_POINT ( 'NONE',  ( -2.169500164636428696, 35.42160933236649356, 3.123960633263314968 ) ) ;
#11960 = CARTESIAN_POINT ( 'NONE',  ( 15.92043486079644943, 145.9828583539951126, -0.2780828054990247544 ) ) ;
#11961 = ORIENTED_EDGE ( 'NONE', *, *, #16452, .F. ) ;
#11962 = CARTESIAN_POINT ( 'NONE',  ( 2.755019269514601632, -14.09852029293599784, -0.1464032776252038315 ) ) ;
#11963 = CARTESIAN_POINT ( 'NONE',  ( -4.394136353581306054, 70.68697878297604120, 1.524000000000005350 ) ) ;
#11964 = CARTESIAN_POINT ( 'NONE',  ( -3.938977128594349342, 28.07268674286775223, 0.7495841607770360460 ) ) ;
#11965 = CARTESIAN_POINT ( 'NONE',  ( -52.86182053370306733, 11.13604294806845729, 4.079049242073634396 ) ) ;
#11966 = CIRCLE ( 'NONE', #26965, 0.5079999999999997851 ) ;
#11967 = CARTESIAN_POINT ( 'NONE',  ( 0.8067276567327370529, -3.745225398377231674, -4.556403025205434609 ) ) ;
#11968 = CARTESIAN_POINT ( 'NONE',  ( 11.65596162629424626, 126.1299551460304542, 1.384704262848757805 ) ) ;
#11969 = CARTESIAN_POINT ( 'NONE',  ( -0.8587611443208003070, 32.35200983223521121, 3.578619333304415839 ) ) ;
#11970 = CARTESIAN_POINT ( 'NONE',  ( -7.093755517943445277, 122.4291926079955317, -0.03209900709771745103 ) ) ;
#11971 = CARTESIAN_POINT ( 'NONE',  ( 1.360477052538118681, -3.804838552850991817, 4.419457122809256511 ) ) ;
#11972 = CARTESIAN_POINT ( 'NONE',  ( 6.503408402854558013, 121.7799126398724354, 0.1299535771408518448 ) ) ;
#11973 = CARTESIAN_POINT ( 'NONE',  ( 8.086262078954034038, 3.373778641329666872, 2.357548046588672008 ) ) ;
#11974 = CARTESIAN_POINT ( 'NONE',  ( -58.03414100541873211, 0.4564111095344824953, -0.9708715263941704032 ) ) ;
#11975 = CARTESIAN_POINT ( 'NONE',  ( -5.526528724494175648, 116.8573403164261464, -0.5291618397137183294 ) ) ;
#11976 = CARTESIAN_POINT ( 'NONE',  ( -0.3558893179482170432, 120.1716774721349168, -0.6349178681961804571 ) ) ;
#11977 = CARTESIAN_POINT ( 'NONE',  ( -15.74027684387364978, 85.27021604205610572, 1.523999999999996913 ) ) ;
#11978 = CARTESIAN_POINT ( 'NONE',  ( -8.095114962461808616, 74.19100168833409725, 1.270000000000002460 ) ) ;
#11979 = CARTESIAN_POINT ( 'NONE',  ( 7.253464168720983096, -10.72948646729439659, -4.330533999219945862 ) ) ;
#11980 = CARTESIAN_POINT ( 'NONE',  ( 3.969496458384241588, 117.3993838096581754, 1.318317423491925933 ) ) ;
#11981 = DIRECTION ( 'NONE',  ( 5.188838149069472160E-16, -1.699382548006136559E-16, -1.000000000000000000 ) ) ;
#11982 = DIRECTION ( 'NONE',  ( -4.017660918040594346E-17, 1.000000000000000000, 2.376309959284834438E-19 ) ) ;
#11983 = CARTESIAN_POINT ( 'NONE',  ( 0.3766127027001021088, 114.7739974199301116, -2.035987775551919565 ) ) ;
#11984 = CARTESIAN_POINT ( 'NONE',  ( -18.44051311885898059, 154.1649927243852858, 0.3121108635588942803 ) ) ;
#11985 = EDGE_LOOP ( 'NONE', ( #20643, #32853, #16744, #747, #2754, #29009, #28759, #26268, #32504, #18155 ) ) ;
#11986 = CARTESIAN_POINT ( 'NONE',  ( -58.83227707057486811, -0.08366279997995551554, -5.898546760656774196E-15 ) ) ;
#11987 = ORIENTED_EDGE ( 'NONE', *, *, #27682, .T. ) ;
#11988 = CARTESIAN_POINT ( 'NONE',  ( -6.640726327341849406E-14, 100.6774662015457409, -1.320564745697255449E-18 ) ) ;
#11989 = CARTESIAN_POINT ( 'NONE',  ( -14.67804715971658602, 148.8626627518845282, -0.1611556191706381425 ) ) ;
#11990 = CARTESIAN_POINT ( 'NONE',  ( 2.090134903116885656, -15.63197564439436427, 5.828951795168951122 ) ) ;
#11991 = CARTESIAN_POINT ( 'NONE',  ( -13.13885824085865828, 121.7804325175133755, 1.194399340605180049 ) ) ;
#11992 = CARTESIAN_POINT ( 'NONE',  ( 20.10769848529506021, 132.0867704272472452, -0.9164310550120229326 ) ) ;
#11993 = CARTESIAN_POINT ( 'NONE',  ( 3.548611814566905664, 16.26088872207684943, 2.983771105379771971 ) ) ;
#11994 = VECTOR ( 'NONE', #16162, 1000.000000000000114 ) ;
#11995 = CARTESIAN_POINT ( 'NONE',  ( -11.61197380483888608, 118.7506923092098674, -0.5208889651483785688 ) ) ;
#11996 = CARTESIAN_POINT ( 'NONE',  ( -58.50406900891774598, -0.02849845305888287772, -0.6794360696606426275 ) ) ;
#11997 = VERTEX_POINT ( 'NONE', #28988 ) ;
#11998 = AXIS2_PLACEMENT_3D ( 'NONE', #41429, #8621, #8414 ) ;
#11999 = CARTESIAN_POINT ( 'NONE',  ( -8.798384421702362346, 117.6845712617741526, -0.1566951044598125509 ) ) ;
#12000 = DIRECTION ( 'NONE',  ( -0.9998004120163609398, 0.000000000000000000, -0.01997839162482749689 ) ) ;
#12001 = CARTESIAN_POINT ( 'NONE',  ( -17.47151851664391842, 144.3974720067888313, 1.548345126349529810 ) ) ;
#12002 = AXIS2_PLACEMENT_3D ( 'NONE', #4505, #10240, #20657 ) ;
#12003 = CARTESIAN_POINT ( 'NONE',  ( -56.18489917335774209, 4.374450811265827355, -2.350758010980142920 ) ) ;
#12004 = CARTESIAN_POINT ( 'NONE',  ( 12.31762543427494627, 122.6846661264431191, -1.317417697584883030 ) ) ;
#12005 = CARTESIAN_POINT ( 'NONE',  ( -21.20529034131901369, 148.8133262010608462, -2.309157841868048067 ) ) ;
#12006 = CARTESIAN_POINT ( 'NONE',  ( -51.81113891419111894, 13.24950054771400332, -4.495723625053127392 ) ) ;
#12007 = CARTESIAN_POINT ( 'NONE',  ( 9.588254403178050111, 123.8224200044116827, -0.4900104160083061933 ) ) ;
#12008 = ORIENTED_EDGE ( 'NONE', *, *, #26687, .F. ) ;
#12009 = CARTESIAN_POINT ( 'NONE',  ( -6.574985064279145419, 120.4115791468657903, -1.154926965394999172 ) ) ;
#12010 = CARTESIAN_POINT ( 'NONE',  ( 4.238804029399687145, -15.60588767656335918, 2.735912002563000822 ) ) ;
#12011 = CARTESIAN_POINT ( 'NONE',  ( -4.158055769619781294, 118.2393601024573542, -0.3861629315888617242 ) ) ;
#12012 = CARTESIAN_POINT ( 'NONE',  ( -57.39043856515510811, 2.569568763584578974, -1.997829887931768411 ) ) ;
#12013 = CARTESIAN_POINT ( 'NONE',  ( -4.922306677375791750, 117.4109580117980016, 0.9480543157666212473 ) ) ;
#12014 = CARTESIAN_POINT ( 'NONE',  ( 2.483060992037590786, 119.7126118883416410, 0.6995635895845426777 ) ) ;
#12015 = CARTESIAN_POINT ( 'NONE',  ( -19.68500000000000227, 71.11999999999999034, 1.904999999999987592 ) ) ;
#12016 = CIRCLE ( 'NONE', #29728, 0.6350000000000014522 ) ;
#12017 = EDGE_CURVE ( 'NONE', #37307, #13736, #3032, .T. ) ;
#12018 = CARTESIAN_POINT ( 'NONE',  ( -1.495267265506447174, 0.7142801726123456652, -8.304712878169773660 ) ) ;
#12019 = CARTESIAN_POINT ( 'NONE',  ( 1.593749994915877100, 120.9451058151398399, 0.1271097986196582930 ) ) ;
#12020 = CARTESIAN_POINT ( 'NONE',  ( -21.18564099849817950, 70.71717898851710515, 1.523999999999996691 ) ) ;
#12021 = CIRCLE ( 'NONE', #7936, 0.2540000000000010583 ) ;
#12023 = VERTEX_POINT ( 'NONE', #25792 ) ;
#12022 = DIRECTION ( 'NONE',  ( -0.000000000000000000, -1.000000000000000000, -0.000000000000000000 ) ) ;
#12024 = CARTESIAN_POINT ( 'NONE',  ( -58.83227707057486811, -0.08366279997995551554, -1.995625700055530397E-14 ) ) ;
#12025 = CARTESIAN_POINT ( 'NONE',  ( 2.168162777261974927, 118.7629491485453883, 1.225215063869133703 ) ) ;
#12026 = CARTESIAN_POINT ( 'NONE',  ( -5.664977208693889210, 53.58606249999999704, -5.033228321271210781 ) ) ;
#12027 = CARTESIAN_POINT ( 'NONE',  ( -49.65811535071824778, 19.11229591699006036, 3.935810587595351517 ) ) ;
#12028 = EDGE_CURVE ( 'NONE', #22529, #11997, #9609, .T. ) ;
#12029 = CARTESIAN_POINT ( 'NONE',  ( -23.19846888548993746, 149.6199392087789306, -0.2334144245939552276 ) ) ;
#12030 = ORIENTED_EDGE ( 'NONE', *, *, #6503, .F. ) ;
#12031 = CARTESIAN_POINT ( 'NONE',  ( -49.59145623469802899, 21.58002366008788542, -1.574391596335681154 ) ) ;
#12032 = CARTESIAN_POINT ( 'NONE',  ( 6.935819294119811573, 121.8978577362516234, -0.1235646913352505261 ) ) ;
#12033 = PLANE ( 'NONE',  #31227 ) ;
#12034 = EDGE_LOOP ( 'NONE', ( #31513, #21724, #10282, #1546 ) ) ;
#12035 = CARTESIAN_POINT ( 'NONE',  ( 1.835530157581306332, 115.7029480720426591, -1.651926545036461302 ) ) ;
#12036 = CARTESIAN_POINT ( 'NONE',  ( -6.489379754819826651, 121.7611753534313550, -0.2571143975131356951 ) ) ;
#12037 = CARTESIAN_POINT ( 'NONE',  ( 5.228661469329079381, -12.87456325985388084, 2.426867231591100182 ) ) ;
#12038 = CARTESIAN_POINT ( 'NONE',  ( -5.877369116562103812, 117.9059190437751141, 0.7167914486236911520 ) ) ;
#12039 = AXIS2_PLACEMENT_3D ( 'NONE', #14099, #30085, #17501 ) ;
#12040 = CARTESIAN_POINT ( 'NONE',  ( 0.8290186328064587107, 117.3993839335269485, -1.455277270773371434 ) ) ;
#12041 = CARTESIAN_POINT ( 'NONE',  ( 9.803363283900793590, 117.9968303279965340, 0.2884128246907768922 ) ) ;
#12042 = TOROIDAL_SURFACE ( 'NONE', #14771, 3.683000000000000718, 0.5080000000000000071 ) ;
#12043 = CARTESIAN_POINT ( 'NONE',  ( 15.64098958305955023, 147.2213129253950399, 0.3794339001978928594 ) ) ;
#12044 = CARTESIAN_POINT ( 'NONE',  ( -17.14499999999999957, 71.11999999999999034, 5.016499999999999737 ) ) ;
#12045 = CARTESIAN_POINT ( 'NONE',  ( -0.7219274401084647685, 31.37879824840181442, -0.6700674276139703123 ) ) ;
#12046 = CARTESIAN_POINT ( 'NONE',  ( -8.067923148479989592, 158.6666700270975525, -0.2162342711943721629 ) ) ;
#12047 = DIRECTION ( 'NONE',  ( -0.9998004120163609398, 0.000000000000000000, -0.01997839162482749689 ) ) ;
#12048 = CARTESIAN_POINT ( 'NONE',  ( -5.938381009910493447, 56.51499999999998636, -4.381499999999999950 ) ) ;
#12049 = VERTEX_POINT ( 'NONE', #2618 ) ;
#12050 = CARTESIAN_POINT ( 'NONE',  ( -6.005079809368049304, 118.6866504246635685, 0.9671915185187860420 ) ) ;
#12051 = DIRECTION ( 'NONE',  ( 0.01997839162482749342, 1.040247600000944484E-18, -0.9998004120163608288 ) ) ;
#12052 = CARTESIAN_POINT ( 'NONE',  ( 7.361208496634183973, 158.3992165788449711, 1.430753602065345298 ) ) ;
#12053 = AXIS2_PLACEMENT_3D ( 'NONE', #31877, #38277, #41903 ) ;
#12054 = CARTESIAN_POINT ( 'NONE',  ( 19.44243145639580916, 150.5708382285403388, -1.622132703307645585 ) ) ;
#12055 = CARTESIAN_POINT ( 'NONE',  ( 4.581910832313284665, -15.30292673639559098, -0.5105377408573423814 ) ) ;
#12056 = CARTESIAN_POINT ( 'NONE',  ( -2.976591712665178857, 117.3922842568077698, -0.6615242749010380452 ) ) ;
#12057 = CARTESIAN_POINT ( 'NONE',  ( 4.888091618989467868, 117.6742611811322377, -0.8477283077776146536 ) ) ;
#12058 = CARTESIAN_POINT ( 'NONE',  ( 0.1515127994569460956, 105.8822825325953261, 5.338933990912773098 ) ) ;
#12059 = EDGE_CURVE ( 'NONE', #35669, #14129, #19872, .T. ) ;
#12060 = AXIS2_PLACEMENT_3D ( 'NONE', #42018, #9831, #38607 ) ;
#12061 = CARTESIAN_POINT ( 'NONE',  ( -9.118838228053551376, 124.0847320388339625, -0.09724818526966641508 ) ) ;
#12062 = CARTESIAN_POINT ( 'NONE',  ( -8.179471065859175383, 156.5149677146980309, -2.065073912022258984 ) ) ;
#12063 = EDGE_CURVE ( 'NONE', #20091, #18538, #36233, .T. ) ;
#12064 = CARTESIAN_POINT ( 'NONE',  ( 3.628834229889370544, -15.44114452258853198, 5.288308529986511353 ) ) ;
#12065 = CARTESIAN_POINT ( 'NONE',  ( 4.795789683585542029, 115.6909491485453145, 1.474960089930022145 ) ) ;
#12066 = ADVANCED_FACE ( 'NONE', ( #15578 ), #38392, .T. ) ;
#12067 = CARTESIAN_POINT ( 'NONE',  ( -2.526208763716937700, 118.1651004855683880, -0.8247881296101019499 ) ) ;
#12068 = ORIENTED_EDGE ( 'NONE', *, *, #12649, .F. ) ;
#12069 = CARTESIAN_POINT ( 'NONE',  ( 6.619107555072841542, 119.9895581359321994, 1.245414878088068278 ) ) ;
#12070 = CARTESIAN_POINT ( 'NONE',  ( -2.958531772299361151, 39.20946620154573736, -1.329372033065077119 ) ) ;
#12071 = CARTESIAN_POINT ( 'NONE',  ( -4.228827370592760815, 117.9846523178514985, -0.9720340673296122835 ) ) ;
#12072 = AXIS2_PLACEMENT_3D ( 'NONE', #21776, #2227, #41410 ) ;
#12073 = CARTESIAN_POINT ( 'NONE',  ( -3.315740949751885491, 124.7872298565087021, -0.06001882965729953001 ) ) ;
#12074 = CARTESIAN_POINT ( 'NONE',  ( -2.878135459294852705, -8.718908198948343014, 7.912908975683875745 ) ) ;
#12075 = CARTESIAN_POINT ( 'NONE',  ( 4.469395743914975405, 155.8822484669112214, 0.8121950557409373106 ) ) ;
#12076 = DIRECTION ( 'NONE',  ( -0.8745520943968245753, 0.4849315768086539524, -5.691349986800526185E-16 ) ) ;
#12077 = CARTESIAN_POINT ( 'NONE',  ( 3.207477133065330221, 159.4163042773305676, -0.4796247595147197784 ) ) ;
#12078 = CARTESIAN_POINT ( 'NONE',  ( 5.224225543104745739, 57.15000000000486580, -5.327462464253549079 ) ) ;
#12079 = CARTESIAN_POINT ( 'NONE',  ( -58.18307367792519358, 0.1082273239375445423, 0.5849402378816875858 ) ) ;
#12080 = CARTESIAN_POINT ( 'NONE',  ( 6.266702236064160658, 78.85741254032750192, 4.063604302808982105 ) ) ;
#12081 = UNCERTAINTY_MEASURE_WITH_UNIT (LENGTH_MEASURE( 1.000000000000000082E-05 ), #18962, 'distance_accuracy_value', 'NONE');
#12082 = DIRECTION ( 'NONE',  ( -0.9998004120163608288, 0.000000000000000000, -0.01997839162482750383 ) ) ;
#12083 = CARTESIAN_POINT ( 'NONE',  ( -4.160656731207808434, 118.2392941210594017, 0.2307236797113647875 ) ) ;
#12084 = CARTESIAN_POINT ( 'NONE',  ( -2.732111087507159475, 116.5293111276780849, -0.05459408159141355271 ) ) ;
#12085 = ORIENTED_EDGE ( 'NONE', *, *, #14599, .F. ) ;
#12086 = CARTESIAN_POINT ( 'NONE',  ( -54.97180548219925100, 8.422794459035404913, 3.467293221275778325 ) ) ;
#12087 = CARTESIAN_POINT ( 'NONE',  ( 4.076354001419692175, 119.1815227253801055, -0.7633122449047639035 ) ) ;
#12088 = CARTESIAN_POINT ( 'NONE',  ( 0.1065646865915093611, 105.8844662015456777, -5.332932678536313809 ) ) ;
#12089 = CARTESIAN_POINT ( 'NONE',  ( -5.883037304650423849, 121.3687970875902806, -0.4830333308872107878 ) ) ;
#12090 = LINE ( 'NONE', #37443, #22634 ) ;
#12091 = CARTESIAN_POINT ( 'NONE',  ( -36.65473259702431363, 28.27472347546385834, 1.523999999999995802 ) ) ;
#12092 = ORIENTED_EDGE ( 'NONE', *, *, #27688, .F. ) ;
#12093 = CARTESIAN_POINT ( 'NONE',  ( -1.471791394198959102, 24.03230288535706549, 4.399545648925609065 ) ) ;
#12094 = CARTESIAN_POINT ( 'NONE',  ( -29.10098582464626915, 61.33321833257333822, 1.523999999999994026 ) ) ;
#12095 = CARTESIAN_POINT ( 'NONE',  ( 2.666490510518176649, -13.49855353256042712, 0.05227394649444803282 ) ) ;
#12096 = CARTESIAN_POINT ( 'NONE',  ( 5.653927021192486357, 78.90752773945908416, -4.880377097574617906 ) ) ;
#12097 = CARTESIAN_POINT ( 'NONE',  ( -29.82321757229076908, 71.17901112636586447, 1.523999999999992250 ) ) ;
#12098 = CARTESIAN_POINT ( 'NONE',  ( -6.080819731615315860, 121.3676167066096241, 0.1940160119882017309 ) ) ;
#12099 = DIRECTION ( 'NONE',  ( 0.9998501190848629872, 0.01731298258490743258, 8.537024980200819846E-16 ) ) ;
#12100 = ADVANCED_FACE ( 'NONE', ( #29198 ), #12399, .T. ) ;
#12101 = CARTESIAN_POINT ( 'NONE',  ( 19.35449845750112274, 128.7092500879292345, 1.403651888282934079 ) ) ;
#12102 = DIRECTION ( 'NONE',  ( -0.9998004120163609398, 0.000000000000000000, -0.01997839162482749689 ) ) ;
#12104 = CARTESIAN_POINT ( 'NONE',  ( 21.36815210116601804, 148.0064520001644723, -1.462276224275803838 ) ) ;
#12103 = CARTESIAN_POINT ( 'NONE',  ( 1.979187190576821465, -15.21425526833739639, 5.301287498526151332 ) ) ;
#12105 = CARTESIAN_POINT ( 'NONE',  ( -18.22365405440210395, 148.2327041560005512, 1.660465927639720451 ) ) ;
#12106 = CARTESIAN_POINT ( 'NONE',  ( -2.673854242087471356, 19.56896771519852862, 3.769861741755948348 ) ) ;
#12107 = CARTESIAN_POINT ( 'NONE',  ( -5.539025187978821485, 159.0643023895801491, -0.7880117631591500027 ) ) ;
#12108 = AXIS2_PLACEMENT_3D ( 'NONE', #19585, #23189, #26412 ) ;
#12109 = CARTESIAN_POINT ( 'NONE',  ( 0.7196250225040555781, 4.026961778641204859, -0.6563066166970625837 ) ) ;
#12110 = EDGE_LOOP ( 'NONE', ( #14983, #33747, #33115, #21411, #30259, #9247, #17002, #880, #16285, #29177, #20885, #985, #19047 ) ) ;
#12111 = CARTESIAN_POINT ( 'NONE',  ( -55.83515739322315596, 4.224161455597911008, 0.1887094293950665747 ) ) ;
#12112 = CARTESIAN_POINT ( 'NONE',  ( -13.73699108721726425, 150.2158912636999730, 0.3005180155469770464 ) ) ;
#12113 = CARTESIAN_POINT ( 'NONE',  ( 2.642260502442670855, -15.21879886190521880, 5.833332612881661383 ) ) ;
#12114 = CARTESIAN_POINT ( 'NONE',  ( 13.46182233857065746, 130.9706359334022920, -1.049250031952806639 ) ) ;
#12115 = ORIENTED_EDGE ( 'NONE', *, *, #27647, .T. ) ;
#12116 = CARTESIAN_POINT ( 'NONE',  ( 2.402331870585372897, 115.7029513689469837, 1.700325149627530896 ) ) ;
#12117 = ADVANCED_FACE ( 'NONE', ( #18559 ), #25178, .F. ) ;
#12118 = ORIENTED_EDGE ( 'NONE', *, *, #11533, .F. ) ;
#12119 = CARTESIAN_POINT ( 'NONE',  ( -4.798808526209403347, 117.8360179528525009, -0.9160348425365787417 ) ) ;
#12120 = CARTESIAN_POINT ( 'NONE',  ( 15.72486432277149504, 146.8976350983841144, 0.2628874744899977189 ) ) ;
#12121 = ORIENTED_EDGE ( 'NONE', *, *, #2518, .F. ) ;
#12122 = CARTESIAN_POINT ( 'NONE',  ( 19.54281269640863883, 149.4594839399872512, 2.484111515072797260 ) ) ;
#12123 = FACE_OUTER_BOUND ( 'NONE', #12323, .T. ) ;
#12124 = CARTESIAN_POINT ( 'NONE',  ( 5.460472493305315922, 56.51499999999995794, 4.448254263655320173 ) ) ;
#12125 = EDGE_CURVE ( 'NONE', #22885, #28739, #26700, .T. ) ;
#12126 = CARTESIAN_POINT ( 'NONE',  ( 3.174366308151882254, 65.62546620154573418, 0.06343139340882768262 ) ) ;
#12127 = CARTESIAN_POINT ( 'NONE',  ( 23.07880092997886834, 149.8841935741895384, 0.1310273949726225018 ) ) ;
#12128 = CARTESIAN_POINT ( 'NONE',  ( 0.03519895179119666290, 115.7029491485446613, -1.761499482103947800 ) ) ;
#12129 = CARTESIAN_POINT ( 'NONE',  ( 4.794367976492847738, 118.7629491485453030, -0.7451781752328570096 ) ) ;
#12130 = CARTESIAN_POINT ( 'NONE',  ( -46.86699512455117400, 25.83114541775341522, 0.4845221143632131300 ) ) ;
#12131 = CARTESIAN_POINT ( 'NONE',  ( 1.689144583495898244, -15.40064781548841566, 5.488289493485431159 ) ) ;
#12132 = CARTESIAN_POINT ( 'NONE',  ( -45.14658554404967106, 22.88857079803865346, 2.562886992506556272 ) ) ;
#12133 = CARTESIAN_POINT ( 'NONE',  ( -4.691480036221459038, 117.9634116254975851, 0.7149672312120951556 ) ) ;
#12134 = ORIENTED_EDGE ( 'NONE', *, *, #1925, .T. ) ;
#12135 = ORIENTED_EDGE ( 'NONE', *, *, #6636, .F. ) ;
#12136 = CARTESIAN_POINT ( 'NONE',  ( -18.27007371177420936, 83.88799758123168715, -1.524000000000003574 ) ) ;
#12137 = AXIS2_PLACEMENT_3D ( 'NONE', #3392, #35974, #16358 ) ;
#12138 = CARTESIAN_POINT ( 'NONE',  ( -5.705078924488119263, 118.5997860065700706, -1.215602027761154336 ) ) ;
#12139 = CARTESIAN_POINT ( 'NONE',  ( -3.997939770797883874, 117.2022048034790487, -1.046317678458332345 ) ) ;
#12140 = CARTESIAN_POINT ( 'NONE',  ( 4.768425879922006949, 117.4736019235508451, 1.192991665150185066 ) ) ;
#12141 = DIRECTION ( 'NONE',  ( 0.000000000000000000, 1.000000000000000000, 0.000000000000000000 ) ) ;
#12142 = CARTESIAN_POINT ( 'NONE',  ( -0.3095834102099264129, 110.3683645023726427, 3.577238406694227546 ) ) ;
#12143 = CARTESIAN_POINT ( 'NONE',  ( 4.224370802630715183, -2.505441902618962935, 1.893578447770203566 ) ) ;
#12144 = DIRECTION ( 'NONE',  ( -1.000000000000000000, -1.092739197465705287E-15, 0.000000000000000000 ) ) ;
#12145 = CARTESIAN_POINT ( 'NONE',  ( -6.580517660824093636E-14, 85.69146620154573668, -4.881702850681514412E-18 ) ) ;
#12146 = CARTESIAN_POINT ( 'NONE',  ( 3.475384634610537038, -12.95405113104661154, 1.817132104271814264 ) ) ;
#12147 = CARTESIAN_POINT ( 'NONE',  ( 4.802295984089199443, 116.4582014290525507, -0.9960034115346418915 ) ) ;
#12148 = CARTESIAN_POINT ( 'NONE',  ( -9.709460118793561634, 122.6450757329969434, -1.337221984871323599 ) ) ;
#12149 = CARTESIAN_POINT ( 'NONE',  ( 5.586884702347365561, 66.64146620154573952, 0.1116392523995368286 ) ) ;
#12150 = CARTESIAN_POINT ( 'NONE',  ( 0.4719448309135433339, 39.20946620154573026, 1.279684108228161143 ) ) ;
#12151 = CARTESIAN_POINT ( 'NONE',  ( -1.114995187443168945, 115.7029400263136125, 1.703459770062234702 ) ) ;
#12152 = CARTESIAN_POINT ( 'NONE',  ( -3.366035089439492811, 13.68705809737886447, 3.178168622443589886 ) ) ;
#12154 = ORIENTED_EDGE ( 'NONE', *, *, #32338, .F. ) ;
#12153 = CARTESIAN_POINT ( 'NONE',  ( 4.790162199822003863, 116.9482543694763166, 0.4383784235352166658 ) ) ;
#12155 = CARTESIAN_POINT ( 'NONE',  ( 4.373232311943012540, 105.1218443201365602, -3.060007391163885870 ) ) ;
#12156 = CARTESIAN_POINT ( 'NONE',  ( 2.350550293776238586, -15.63281720864678803, 5.143235457246400522 ) ) ;
#12157 = CARTESIAN_POINT ( 'NONE',  ( -15.27645447632550280, 153.0676604005411434, 1.747501773188613994 ) ) ;
#12158 = CIRCLE ( 'NONE', #35968, 0.6350000000000014522 ) ;
#12159 = CARTESIAN_POINT ( 'NONE',  ( 0.3717569628964236816, 23.89034148085472964, -0.9007439114964531646 ) ) ;
#12160 = CARTESIAN_POINT ( 'NONE',  ( 0.6184700321857297123, 7.203955656377674543, 0.7581051976356608657 ) ) ;
#12161 = ORIENTED_EDGE ( 'NONE', *, *, #9005, .F. ) ;
#12162 = VERTEX_POINT ( 'NONE', #2824 ) ;
#12163 = CARTESIAN_POINT ( 'NONE',  ( -5.580495364573205386, 77.10007210032874525, 1.270000000000004237 ) ) ;
#12164 = CARTESIAN_POINT ( 'NONE',  ( 2.331513492273026511, 111.1666841684333633, 3.236375129800146411 ) ) ;
#12165 = CARTESIAN_POINT ( 'NONE',  ( -11.07452758269552895, 153.1537610418535849, 0.9542791616922486897 ) ) ;
#12166 = CARTESIAN_POINT ( 'NONE',  ( -30.44847906516384128, 70.61110078258337808, -1.270000000000007345 ) ) ;
#12167 = CARTESIAN_POINT ( 'NONE',  ( 3.815374714676033729, -13.42234902974577615, 3.291045305163978085 ) ) ;
#12168 = CARTESIAN_POINT ( 'NONE',  ( 2.509025565091295373, 119.7126118883416410, -0.5998098196673841143 ) ) ;
#12169 = CARTESIAN_POINT ( 'NONE',  ( -20.22212501804825635, 145.4934252350392114, -2.489959791085248231 ) ) ;
#12170 = CARTESIAN_POINT ( 'NONE',  ( -5.809227842914839179, 77.60418761620948658, 1.524000000000003352 ) ) ;
#12171 = ADVANCED_FACE ( 'NONE', ( #2406 ), #11737, .T. ) ;
#12172 = CARTESIAN_POINT ( 'NONE',  ( 7.849374513171908596, 122.2536118085260171, 0.7624099742200379781 ) ) ;
#12173 = CARTESIAN_POINT ( 'NONE',  ( 4.074910602682932925, 118.2429491485453354, -0.1454311599470142491 ) ) ;
#12174 = CARTESIAN_POINT ( 'NONE',  ( 12.04197430995775164, 130.4833683797432684, -0.05493623226408298615 ) ) ;
#12175 = ORIENTED_EDGE ( 'NONE', *, *, #790, .F. ) ;
#12176 = CARTESIAN_POINT ( 'NONE',  ( -1.248055628918211646, 106.2083702520889119, -5.188232620816602747 ) ) ;
#12177 = DIRECTION ( 'NONE',  ( -0.8745520943968243532, 0.4849315768086547296, -5.361993529360573944E-16 ) ) ;
#12178 = VECTOR ( 'NONE', #1833, 1000.000000000000000 ) ;
#12179 = AXIS2_PLACEMENT_3D ( 'NONE', #19196, #6225, #12604 ) ;
#12180 = FACE_OUTER_BOUND ( 'NONE', #37503, .T. ) ;
#12181 = B_SPLINE_CURVE_WITH_KNOTS ( 'NONE', 3,
 ( #24971, #4981, #30941, #8366 ),
 .UNSPECIFIED., .F., .F.,
 ( 4, 4 ),
 ( 0.000000000000000000, 0.9716004430332778607 ),
 .UNSPECIFIED. ) ;
#12182 = CARTESIAN_POINT ( 'NONE',  ( -55.57144106516901161, 6.156191000065342145, 3.024401744045409401 ) ) ;
#12183 = CARTESIAN_POINT ( 'NONE',  ( 8.093748642744952093, 23.43776531741863423, -2.407353130276413733 ) ) ;
#12184 = CARTESIAN_POINT ( 'NONE',  ( 9.904299505090465416, 154.0333045108203009, 1.503511620041811936 ) ) ;
#12185 = DIRECTION ( 'NONE',  ( 0.8745520943968235761, -0.4849315768086558398, 4.268512490100410909E-16 ) ) ;
#12186 = CARTESIAN_POINT ( 'NONE',  ( 20.47124607682627584, 129.0748834149669904, 0.3487454591146179061 ) ) ;
#12187 = CARTESIAN_POINT ( 'NONE',  ( -5.326805317745573198, 116.9650601603920279, 0.7421267338694930160 ) ) ;
#12188 = CARTESIAN_POINT ( 'NONE',  ( -4.157303687089163979, 2.242350289152962528, -2.029258473605290103 ) ) ;
#12189 = CARTESIAN_POINT ( 'NONE',  ( 11.83539255247743149, 152.0195595274622349, 0.2364993098673506822 ) ) ;
#12190 = CARTESIAN_POINT ( 'NONE',  ( 2.407351327831447119, 1.847773219181642057, 8.093752867084216263 ) ) ;
#12191 = CARTESIAN_POINT ( 'NONE',  ( -5.736468567008435215, 78.90050738914777639, -5.037638016205330693 ) ) ;
#12192 = CARTESIAN_POINT ( 'NONE',  ( -8.737319200505471173, 117.9293801533141419, -0.7003869330726086861 ) ) ;
#12193 = CARTESIAN_POINT ( 'NONE',  ( -1.032349031751560231, 124.2655319029901335, -0.08020592950830171541 ) ) ;
#12194 = FACE_OUTER_BOUND ( 'NONE', #24191, .T. ) ;
#12195 = CARTESIAN_POINT ( 'NONE',  ( -6.618965589514436111E-14, 97.88346620154572975, 1.207165459396359365E-19 ) ) ;
#12196 = CARTESIAN_POINT ( 'NONE',  ( -4.349660437102230048, 31.17966527223318707, -1.615541842050199461 ) ) ;
#12197 = CARTESIAN_POINT ( 'NONE',  ( 0.4921998799175691941, 117.3993826277446146, 1.493758782920931338 ) ) ;
#12198 = CARTESIAN_POINT ( 'NONE',  ( 13.46199999999999797, 17.14499999999999957, 1.648619521012166368E-15 ) ) ;
#12199 = DIRECTION ( 'NONE',  ( -5.206863593109713661E-17, 1.000000000000000000, -1.077750396879097183E-30 ) ) ;
#12200 = CARTESIAN_POINT ( 'NONE',  ( 0.2185697341916492398, 107.6766875080336376, -4.612355970162428598 ) ) ;
#12201 = CARTESIAN_POINT ( 'NONE',  ( -10.65151157945287785, 157.9324367681937815, 0.3596066298475820155 ) ) ;
#12202 = EDGE_LOOP ( 'NONE', ( #34123, #40570, #31134, #6447 ) ) ;
#12203 = CARTESIAN_POINT ( 'NONE',  ( -58.83227707057488232, -0.08366279997998327111, -5.792906548978703126E-15 ) ) ;
#12204 = AXIS2_PLACEMENT_3D ( 'NONE', #40342, #37542, #17724 ) ;
#12205 = AXIS2_PLACEMENT_3D ( 'NONE', #27288, #36890, #7708 ) ;
#12206 = ORIENTED_EDGE ( 'NONE', *, *, #19359, .F. ) ;
#12207 = DIRECTION ( 'NONE',  ( -0.8745520943968250194, 0.4849315768086532863, -5.361993529360574930E-16 ) ) ;
#12208 = CARTESIAN_POINT ( 'NONE',  ( -15.20382161411771271, 143.4031467678206297, -0.1686640459771217015 ) ) ;
#12209 = CARTESIAN_POINT ( 'NONE',  ( 6.238852630440780977, -14.32403127715267743, 0.8647906437036265714 ) ) ;
#12210 = CARTESIAN_POINT ( 'NONE',  ( -20.61281631175405238, 145.6130255286810495, 1.629730044589046578 ) ) ;
#12211 = CARTESIAN_POINT ( 'NONE',  ( 7.538779372106241716, 158.4854300789945398, -0.9926846707982194262 ) ) ;
#12212 = CARTESIAN_POINT ( 'NONE',  ( -3.562413952978887632, 23.18266144714348798, 2.948169924785601470 ) ) ;
#12213 = CARTESIAN_POINT ( 'NONE',  ( -22.49834027909124501, 137.1624432810789358, -0.8864494676080413305 ) ) ;
#12214 = CARTESIAN_POINT ( 'NONE',  ( -57.57892384836331701, 1.967499851525790211, -1.750299182700436162 ) ) ;
#12215 = VERTEX_POINT ( 'NONE', #15366 ) ;
#12216 = CARTESIAN_POINT ( 'NONE',  ( -0.004379098345612333562, 122.8649044353672934, 0.2191479880733796237 ) ) ;
#12217 = CARTESIAN_POINT ( 'NONE',  ( -11.24191166894635430, 82.34025985790688651, 1.270000000000000240 ) ) ;
#12218 = CARTESIAN_POINT ( 'NONE',  ( -12.55519531044868486, 126.0212559692275249, 1.204658208757142468 ) ) ;
#12219 = CARTESIAN_POINT ( 'NONE',  ( -56.17894221855530645, 4.386908320153513507, -2.354358595961671519 ) ) ;
#12220 = CARTESIAN_POINT ( 'NONE',  ( 10.61219202124994609, 121.9340018749941663, -1.210411277014657561 ) ) ;
#12221 = CARTESIAN_POINT ( 'NONE',  ( -18.79035964875408382, 131.8417273817641444, -2.102833481017198025 ) ) ;
#12222 = CARTESIAN_POINT ( 'NONE',  ( -49.72660956849071567, 16.83360665160238412, -5.072308565479707099 ) ) ;
#12223 = EDGE_CURVE ( 'NONE', #41093, #9715, #35552, .T. ) ;
#12224 = CARTESIAN_POINT ( 'NONE',  ( 2.706440023329436340, 120.6505882111413683, -0.2907491850344327555 ) ) ;
#12225 = ORIENTED_EDGE ( 'NONE', *, *, #6639, .T. ) ;
#12226 = CARTESIAN_POINT ( 'NONE',  ( -17.60198365394341735, 148.3509993576462307, -2.281626375285575214 ) ) ;
#12227 = CARTESIAN_POINT ( 'NONE',  ( 3.555176734920527437, -15.70662665601262020, 4.164229356387482817 ) ) ;
#12228 = CARTESIAN_POINT ( 'NONE',  ( -6.540217103314379345E-14, 82.64346620154573486, 2.383338306179204368E-29 ) ) ;
#12229 = CARTESIAN_POINT ( 'NONE',  ( -57.07867440696631434, 2.606095844753547830, -1.988717289889820661 ) ) ;
#12230 = AXIS2_PLACEMENT_3D ( 'NONE', #33776, #1400, #14356 ) ;
#12231 = CARTESIAN_POINT ( 'NONE',  ( -4.899759748343297083, 117.5479811350548829, 0.9251532171549939898 ) ) ;
#12232 = CARTESIAN_POINT ( 'NONE',  ( 16.68865417205000767, 140.0893442862094673, 2.224985475129671819 ) ) ;
#12233 = CARTESIAN_POINT ( 'NONE',  ( -46.38316532014823679, 26.05065462784537900, 1.523999999999991140 ) ) ;
#12234 = CARTESIAN_POINT ( 'NONE',  ( 1.223683442775902463, 5.461509463947571419, 8.358860550006438572 ) ) ;
#12235 = CARTESIAN_POINT ( 'NONE',  ( 6.485149764178022913, 121.7431354732680973, 0.3115821950655747186 ) ) ;
#12236 = CARTESIAN_POINT ( 'NONE',  ( -5.809227842914839179, 77.60418761620948658, -1.523999999999996025 ) ) ;
#12238 = ORIENTED_EDGE ( 'NONE', *, *, #30280, .T. ) ;
#12237 = CARTESIAN_POINT ( 'NONE',  ( -41.41491986784952672, 22.70581808553410497, -0.08466666666667260754 ) ) ;
#12239 = CARTESIAN_POINT ( 'NONE',  ( -0.1178540848408428932, 118.1588900175827774, 0.9046132285812910068 ) ) ;
#12240 = CARTESIAN_POINT ( 'NONE',  ( -58.30521585032268206, -0.1116666926106041347, 0.6575736669891736330 ) ) ;
#12241 = CARTESIAN_POINT ( 'NONE',  ( -51.09578318342275338, 14.49152418417465960, 4.666602106937938643 ) ) ;
#12242 = CARTESIAN_POINT ( 'NONE',  ( -7.920550782940143364, 121.8828277235336657, -1.006747304157872502 ) ) ;
#12243 = DIRECTION ( 'NONE',  ( -5.188838149069472160E-16, 1.699382548006136559E-16, 1.000000000000000000 ) ) ;
#12244 = CARTESIAN_POINT ( 'NONE',  ( -50.78366386294959511, 19.84645248585079003, 1.614153572948400672 ) ) ;
#12245 = CARTESIAN_POINT ( 'NONE',  ( -18.62524206359434231, 154.1412379532633850, -0.2279367985168733735 ) ) ;
#12246 = ORIENTED_EDGE ( 'NONE', *, *, #5103, .T. ) ;
#12247 = CARTESIAN_POINT ( 'NONE',  ( -49.65811535071824778, 19.11229591699006036, -3.935810587595368837 ) ) ;
#12248 = CARTESIAN_POINT ( 'NONE',  ( -7.794982761785219871, 122.5553005452032664, -0.3869435098480608626 ) ) ;
#12249 = FACE_OUTER_BOUND ( 'NONE', #9315, .T. ) ;
#12250 = VERTEX_POINT ( 'NONE', #12601 ) ;
#12251 = CARTESIAN_POINT ( 'NONE',  ( 2.010736835508156961, 115.7029473884088446, -1.638949895126919687 ) ) ;
#12252 = CARTESIAN_POINT ( 'NONE',  ( -15.80103543825248025, 146.2514283349100594, -0.5462135236119773918 ) ) ;
#12253 = CARTESIAN_POINT ( 'NONE',  ( 2.063686733023943898, -15.30319371230426384, 5.972472134935498111 ) ) ;
#12254 = CARTESIAN_POINT ( 'NONE',  ( -2.888962495635027050, 158.8946464937287999, 1.317949658345222153 ) ) ;
#12255 = CARTESIAN_POINT ( 'NONE',  ( -8.473844426907703564, 67.77203500197072117, -1.269999999999995799 ) ) ;
#12256 = CARTESIAN_POINT ( 'NONE',  ( 6.905720769004601856, 117.2044255678715814, 0.3198409844323961138 ) ) ;
#12257 = CARTESIAN_POINT ( 'NONE',  ( 10.94874868616072305, 127.9616117985000443, 0.3245695131468429584 ) ) ;
#12258 = DIRECTION ( 'NONE',  ( -0.8745520943968013716, 0.4849315768086958633, -4.268512490100402527E-16 ) ) ;
#12259 = CARTESIAN_POINT ( 'NONE',  ( -0.2871545817224689379, 15.30011720780053430, 0.9385489134671207712 ) ) ;
#12260 = CARTESIAN_POINT ( 'NONE',  ( -5.786284826928912217, 116.9447284183608389, -0.1988161383433786344 ) ) ;
#12261 = DIRECTION ( 'NONE',  ( 0.9454731675810336133, -0.3256999990547843615, 5.459396135145337199E-16 ) ) ;
#12262 = EDGE_CURVE ( 'NONE', #38547, #1745, #28055, .T. ) ;
#12263 = AXIS2_PLACEMENT_3D ( 'NONE', #32826, #22361, #32192 ) ;
#12264 = DIRECTION ( 'NONE',  ( -0.000000000000000000, 1.000000000000000000, -0.000000000000000000 ) ) ;
#12265 = ORIENTED_EDGE ( 'NONE', *, *, #5278, .F. ) ;
#12266 = B_SPLINE_CURVE_WITH_KNOTS ( 'NONE', 3,
 ( #39141, #9529, #32751, #10374, #9946, #600, #22709, #35738, #32114, #3585, #13573, #13357, #29556, #26346, #19105, #29117, #10156, #22497 ),
 .UNSPECIFIED., .F., .F.,
 ( 4, 2, 2, 2, 2, 2, 2, 2, 4 ),
 ( 0.0003740220254444729222, 0.003617377532827396533, 0.006860733040210320252, 0.008482410793901782112, 0.009293249670747497429, 0.01010408854759321275, 0.01172576630128463991, 0.01253660517813036390, 0.01334744405497608789 ),
 .UNSPECIFIED. ) ;
#12267 = CARTESIAN_POINT ( 'NONE',  ( 3.447093754558173462, 117.7853021311141930, 0.8661349407177386661 ) ) ;
#12268 = CARTESIAN_POINT ( 'NONE',  ( 1.818839793882075506, -13.69063247836898434, -4.255424433905749204 ) ) ;
#12269 = CARTESIAN_POINT ( 'NONE',  ( 0.3947855200658545449, 117.7785671674745771, 0.5311790665990140381 ) ) ;
#12270 = CARTESIAN_POINT ( 'NONE',  ( 5.883382875664553424, 118.7305451321402501, -0.9239882381799516819 ) ) ;
#12271 = CARTESIAN_POINT ( 'NONE',  ( 4.581790953832888924, -15.30257397518579232, -0.5115867857466148694 ) ) ;
#12272 = CARTESIAN_POINT ( 'NONE',  ( -15.97393847379854215, 155.1095016151506911, -1.658827062323852575 ) ) ;
#12273 = CARTESIAN_POINT ( 'NONE',  ( 4.809314660303178890, 117.8761932044920684, -0.6706302678270985584 ) ) ;
#12274 = EDGE_CURVE ( 'NONE', #6241, #22953, #13805, .T. ) ;
#12275 = CARTESIAN_POINT ( 'NONE',  ( -0.1065646865916381608, 105.8844662015456777, 5.332932678536313809 ) ) ;
#12276 = CARTESIAN_POINT ( 'NONE',  ( -7.567922279963403831, 122.4257779438054285, -0.07478732235760089664 ) ) ;
#12277 = CARTESIAN_POINT ( 'NONE',  ( -11.88796246241990673, 122.6721150436042223, -1.770419579776735697 ) ) ;
#12278 = CARTESIAN_POINT ( 'NONE',  ( 5.567940837815767097, -14.86657585147074734, 2.969021103613282531 ) ) ;
#12279 = CARTESIAN_POINT ( 'NONE',  ( 5.239656519176586258, 115.6909491485453145, 1.022206641662168236 ) ) ;
#12280 = CIRCLE ( 'NONE', #10235, 0.5080000000000000071 ) ;
#12281 = CARTESIAN_POINT ( 'NONE',  ( -0.7927369056973760930, 117.9496054624362245, -1.398781258546966555 ) ) ;
#12282 = EDGE_CURVE ( 'NONE', #5065, #1213, #38289, .T. ) ;
#12283 = VERTEX_POINT ( 'NONE', #10815 ) ;
#12284 = CARTESIAN_POINT ( 'NONE',  ( 18.87709319873806990, 147.8663216482595146, 2.479723349601893112 ) ) ;
#12285 = CARTESIAN_POINT ( 'NONE',  ( 5.237379388564934679, 115.7029491485453292, 1.024072862575109655 ) ) ;
#12286 = TOROIDAL_SURFACE ( 'NONE', #33365, 3.683000000000000718, 0.5080000000000000071 ) ;
#12287 = DIRECTION ( 'NONE',  ( 0.9454731675810359448, -0.3256999990547780333, 5.459396135145339171E-16 ) ) ;
#12288 = CARTESIAN_POINT ( 'NONE',  ( -1.642663419667714564, 119.5945091202099348, 0.5769171603192790876 ) ) ;
#12289 = CARTESIAN_POINT ( 'NONE',  ( -4.020893062959163267, -8.947226795047690473, 7.425401991387179379 ) ) ;
#12290 = CARTESIAN_POINT ( 'NONE',  ( 9.732298487430668388, 124.2227999206177032, 0.8093454005834664899 ) ) ;
#12291 = CARTESIAN_POINT ( 'NONE',  ( 14.92885934485193289, 156.1361208441215922, -0.4494106821051803702 ) ) ;
#12292 = FACE_OUTER_BOUND ( 'NONE', #31169, .T. ) ;
#12293 = CARTESIAN_POINT ( 'NONE',  ( -58.34308235763123918, -0.2355438472691235297, 0.2038357956814182415 ) ) ;
#12294 = CARTESIAN_POINT ( 'NONE',  ( -5.560415744471473687, 116.7072868167284980, -0.2237494900823625843 ) ) ;
#12295 = EDGE_CURVE ( 'NONE', #26813, #28177, #20384, .T. ) ;
#12296 = CARTESIAN_POINT ( 'NONE',  ( -4.074955089416341991, 118.2429491485453354, 0.1454234154749719787 ) ) ;
#12297 = CARTESIAN_POINT ( 'NONE',  ( -22.83540780336928577, 150.4058779721138421, -0.4563057931615319140 ) ) ;
#12298 = EDGE_LOOP ( 'NONE', ( #24982, #32957, #25320, #17657 ) ) ;
#12299 = CARTESIAN_POINT ( 'NONE',  ( 8.251510532373199425, 120.4738826143435944, -1.099784515884263403 ) ) ;
#12300 = CARTESIAN_POINT ( 'NONE',  ( 5.329260751456349254, 104.6144662015457527, 0.2904590649852882289 ) ) ;
#12301 = CARTESIAN_POINT ( 'NONE',  ( -10.03827118703590848, 124.8772485319846055, -0.7459150106818384085 ) ) ;
#12302 = CARTESIAN_POINT ( 'NONE',  ( 10.28897677580358305, 57.14999999999999858, -5.016499999999999737 ) ) ;
#12303 = AXIS2_PLACEMENT_3D ( 'NONE', #21613, #31435, #15241 ) ;
#12304 = CARTESIAN_POINT ( 'NONE',  ( 1.797937260761245382, 116.4670535197835051, 0.04904229828524086371 ) ) ;
#12305 = EDGE_CURVE ( 'NONE', #29332, #26682, #13007, .T. ) ;
#12306 = ORIENTED_EDGE ( 'NONE', *, *, #26450, .T. ) ;
#12307 = CARTESIAN_POINT ( 'NONE',  ( -2.029258473809828711, 23.83235028914373288, 4.157303687431403993 ) ) ;
#12308 = CARTESIAN_POINT ( 'NONE',  ( -29.81772749291372904, 58.81923324269567388, 1.523999999999992916 ) ) ;
#12309 = CARTESIAN_POINT ( 'NONE',  ( -4.999995268433905515, 117.4036871737256007, 0.8306561334194828561 ) ) ;
#12310 = CARTESIAN_POINT ( 'NONE',  ( 6.756648348127327175, 78.81597664337223819, -3.183520453979959086 ) ) ;
#12311 = DIRECTION ( 'NONE',  ( -5.188838149069471174E-16, 1.699382548006136313E-16, 1.000000000000000000 ) ) ;
#12312 = CARTESIAN_POINT ( 'NONE',  ( -7.796775163588184121, 122.5850086010226363, 0.007623726692081094630 ) ) ;
#12313 = CARTESIAN_POINT ( 'NONE',  ( -0.8806307086779237014, 20.21867702141905099, 4.540528814573361771 ) ) ;
#12314 = CARTESIAN_POINT ( 'NONE',  ( -0.006370369177400351211, 117.0014201992989058, 0.3187993231787207837 ) ) ;
#12315 = CARTESIAN_POINT ( 'NONE',  ( -1.644049521069662845, 104.6144662015457243, -4.546677564578934572 ) ) ;
#12317 = CARTESIAN_POINT ( 'NONE',  ( 14.20167894085449944, 122.0820592118662091, -1.087754808798858219 ) ) ;
#12316 = CARTESIAN_POINT ( 'NONE',  ( 4.799643950526473191, 115.7029491485453292, 1.472414092453835588 ) ) ;
#12318 = AXIS2_PLACEMENT_3D ( 'NONE', #21528, #34767, #35188 ) ;
#12319 = CARTESIAN_POINT ( 'NONE',  ( -0.01051219832188539718, 119.4384375980492194, 0.5260733902271050866 ) ) ;
#12320 = CARTESIAN_POINT ( 'NONE',  ( -3.618988008572157522, 19.14412854911201123, 2.900346660497036044 ) ) ;
#12321 = CARTESIAN_POINT ( 'NONE',  ( -22.80589948333492600, 149.4631731099488832, -1.425235564609340422 ) ) ;
#12322 = CARTESIAN_POINT ( 'NONE',  ( 0.8777592251401162837, 3.590160258842859164, -0.4283581310676968790 ) ) ;
#12323 = EDGE_LOOP ( 'NONE', ( #8223, #11606, #31756, #26983 ) ) ;
#12324 = CARTESIAN_POINT ( 'NONE',  ( -54.07635852566403400, 7.689673991023174615, 1.154061576158796454 ) ) ;
#12325 = CARTESIAN_POINT ( 'NONE',  ( -13.80952258003161148, 150.2278160098252329, 0.4282869786672489076 ) ) ;
#12326 = CARTESIAN_POINT ( 'NONE',  ( 5.856266048228023990, -12.49204451700697227, 1.108958003446382845 ) ) ;
#12327 = CARTESIAN_POINT ( 'NONE',  ( 4.935370518415115981, 156.1188696671683260, -1.185051001079852062 ) ) ;
#12328 = ORIENTED_EDGE ( 'NONE', *, *, #16742, .T. ) ;
#12329 = DIRECTION ( 'NONE',  ( -0.7770581983690852956, 0.6294287539884014793, -5.101669463485840682E-16 ) ) ;
#12330 = CARTESIAN_POINT ( 'NONE',  ( -4.773031995702506691, 117.8805138891626427, -0.8734539205960981656 ) ) ;
#12331 = ADVANCED_FACE ( 'NONE', ( #20806 ), #4660, .F. ) ;
#12332 = CARTESIAN_POINT ( 'NONE',  ( 9.538359384048550993, 124.8019839352694476, 0.1905991205270209932 ) ) ;
#12333 = ORIENTED_EDGE ( 'NONE', *, *, #32173, .T. ) ;
#12334 = CARTESIAN_POINT ( 'NONE',  ( 19.70389350229440595, 149.1964539096042870, 2.489783701940901928 ) ) ;
#12335 = FACE_OUTER_BOUND ( 'NONE', #20507, .T. ) ;
#12336 = FACE_OUTER_BOUND ( 'NONE', #27193, .T. ) ;
#12337 = AXIS2_PLACEMENT_3D ( 'NONE', #16874, #26676, #7099 ) ;
#12338 = CARTESIAN_POINT ( 'NONE',  ( 4.879798404911957377, 117.5475425101833196, -0.9415396859558378129 ) ) ;
#12339 = CARTESIAN_POINT ( 'NONE',  ( 22.60023854264588294, 150.6256779753201158, 0.001684207673827021372 ) ) ;
#12340 = EDGE_CURVE ( 'NONE', #35654, #28485, #33410, .T. ) ;
#12341 = LINE ( 'NONE', #8727, #41091 ) ;
#12342 = VECTOR ( 'NONE', #10600, 1000.000000000000000 ) ;
#12343 = CARTESIAN_POINT ( 'NONE',  ( -46.88219813129796165, 25.44970738892517659, 1.667955656040396750 ) ) ;
#12344 = CARTESIAN_POINT ( 'NONE',  ( 5.506767014370323565, 78.91949168437542994, 5.113098386149627750 ) ) ;
#12345 = CARTESIAN_POINT ( 'NONE',  ( 1.926753168619404377, -15.13879046584015775, 5.903414407318583024 ) ) ;
#12346 = CARTESIAN_POINT ( 'NONE',  ( -45.82931853585290582, 22.14969803457954356, 3.600065900675641029 ) ) ;
#12347 = CARTESIAN_POINT ( 'NONE',  ( -6.059261036834473479, 56.81853847168529370, -4.948064083792231393 ) ) ;
#12348 = CARTESIAN_POINT ( 'NONE',  ( -4.732736203862330626, 117.9644780015066914, 0.6133938389771328437 ) ) ;
#12349 = EDGE_LOOP ( 'NONE', ( #8010, #26597, #34834, #30368 ) ) ;
#12350 = EDGE_LOOP ( 'NONE', ( #9077, #33131, #20604, #23519 ) ) ;
#12351 = CYLINDRICAL_SURFACE ( 'NONE', #17975, 6.350000000000004974 ) ;
#12352 = EDGE_CURVE ( 'NONE', #24559, #29906, #27426, .T. ) ;
#12353 = CARTESIAN_POINT ( 'NONE',  ( 3.478480445305584645, 118.6155477304225343, -0.7926535167593043996 ) ) ;
#12354 = CARTESIAN_POINT ( 'NONE',  ( -0.1274156416095612032, 105.9117620634264370, -5.326488824310051662 ) ) ;
#12355 = CARTESIAN_POINT ( 'NONE',  ( 4.659798553400928078, 118.0075236409115149, 0.7771128701194636168 ) ) ;
#12356 = AXIS2_PLACEMENT_3D ( 'NONE', #29646, #26445, #3250 ) ;
#12357 = CARTESIAN_POINT ( 'NONE',  ( -6.654617103318593247E-14, 104.6144662015457243, 1.534725424433578570E-31 ) ) ;
#12358 = CARTESIAN_POINT ( 'NONE',  ( -0.09221630143787259981, 107.6766875080336376, 4.614880812453306724 ) ) ;
#12359 = CARTESIAN_POINT ( 'NONE',  ( -2.070226828232369254, -8.352695179381779411, -4.151654383260235726 ) ) ;
#12360 = ADVANCED_FACE ( 'NONE', ( #19601 ), #40439, .T. ) ;
#12361 = CARTESIAN_POINT ( 'NONE',  ( -49.59816314059868603, 17.91649583374772092, 5.069000701391646935 ) ) ;
#12362 = CARTESIAN_POINT ( 'NONE',  ( 4.842864477130134127, 117.0601473006971105, -0.7870117353683143691 ) ) ;
#12363 = CARTESIAN_POINT ( 'NONE',  ( -0.8144440842626328170, 156.8926940187749324, -1.343054762528749890 ) ) ;
#12364 = CARTESIAN_POINT ( 'NONE',  ( 5.035933200060415338, 117.3993844219003648, -0.5513780243448201945 ) ) ;
#12365 = CARTESIAN_POINT ( 'NONE',  ( -5.997746767061387985, 28.36824686342176349, 0.3198938015187350881 ) ) ;
#12366 = CYLINDRICAL_SURFACE ( 'NONE', #37841, 0.6349999999999998979 ) ;
#12367 = CARTESIAN_POINT ( 'NONE',  ( -3.640175008984333882, 11.51306413504884318, -2.862805987297033727 ) ) ;
#12369 = EDGE_LOOP ( 'NONE', ( #37068, #4093, #15904, #5156, #29309, #26333, #22301, #2934 ) ) ;
#12368 = CARTESIAN_POINT ( 'NONE',  ( 5.820459347748528245, 117.1115750087645608, 0.4818200784724925301 ) ) ;
#12370 = CARTESIAN_POINT ( 'NONE',  ( -2.149574005142933508, 105.1243567940866654, -4.891951615042300361 ) ) ;
#12371 = CARTESIAN_POINT ( 'NONE',  ( 3.885732391871624447, -15.29168275415018741, 1.106840230638412192 ) ) ;
#12372 = CARTESIAN_POINT ( 'NONE',  ( -1.284628845569858679, 118.8689652838214244, 0.6394392525890020273 ) ) ;
#12373 = AXIS2_PLACEMENT_3D ( 'NONE', #2776, #14893, #15732 ) ;
#12374 = CARTESIAN_POINT ( 'NONE',  ( -0.3421040304481134942, 19.14286131909006272, 0.9136164113388466346 ) ) ;
#12375 = VECTOR ( 'NONE', #1581, 1000.000000000000114 ) ;
#12376 = CARTESIAN_POINT ( 'NONE',  ( -0.8667032531718782407, 4.505117207799016477, 0.4606053492026337959 ) ) ;
#12377 = ORIENTED_EDGE ( 'NONE', *, *, #35598, .T. ) ;
#12378 = CIRCLE ( 'NONE', #8875, 0.2539999999999989488 ) ;
#12379 = ORIENTED_EDGE ( 'NONE', *, *, #26485, .T. ) ;
#12380 = FACE_OUTER_BOUND ( 'NONE', #17626, .T. ) ;
#12381 = CARTESIAN_POINT ( 'NONE',  ( 1.464138133146175580, 108.1711930243730109, 4.389422119207357476 ) ) ;
#12382 = CARTESIAN_POINT ( 'NONE',  ( -9.755760200704729712, 153.9716628027005925, 0.9476658408544212930 ) ) ;
#12383 = CARTESIAN_POINT ( 'NONE',  ( -58.83227707057486811, -0.08366279997995551554, -1.529465441686574059E-14 ) ) ;
#12384 = CARTESIAN_POINT ( 'NONE',  ( 3.509037099356659084, -13.47856448578629873, 2.732507022889707038 ) ) ;
#12385 = CARTESIAN_POINT ( 'NONE',  ( 17.80491421350291503, 148.0643276405518804, -1.576192721057972923 ) ) ;
#12386 = CARTESIAN_POINT ( 'NONE',  ( -17.92333008985184506, 151.7072807693909340, -2.394054079121861633 ) ) ;
#12387 = DIRECTION ( 'NONE',  ( 0.1565721916418051640, 0.9876665170007951078, -6.504343050004418945E-15 ) ) ;
#12388 = CARTESIAN_POINT ( 'NONE',  ( 8.517627334839968256, 118.9460427874306703, 1.261003614275605367 ) ) ;
#12389 = CARTESIAN_POINT ( 'NONE',  ( -4.128276239086840604, 33.50807246189903310, 3.501313855992088442 ) ) ;
#12390 = CARTESIAN_POINT ( 'NONE',  ( 0.004910621514677531059, 156.3161161488371533, -0.2457475809811480449 ) ) ;
#12391 = ORIENTED_EDGE ( 'NONE', *, *, #5865, .T. ) ;
#12392 = CARTESIAN_POINT ( 'NONE',  ( 4.973152232786927307, 117.3993868326352015, 0.9753084504214339923 ) ) ;
#12393 = LINE ( 'NONE', #6012, #34668 ) ;
#12394 = CARTESIAN_POINT ( 'NONE',  ( 2.958531772299236362, 39.20946620154573736, 1.329372033065076231 ) ) ;
#12395 = EDGE_CURVE ( 'NONE', #28559, #19659, #30143, .T. ) ;
#12396 = CARTESIAN_POINT ( 'NONE',  ( -13.85159022459153988, 16.51000000000000156, 5.016499999999999737 ) ) ;
#12397 = CARTESIAN_POINT ( 'NONE',  ( -8.202033116754899211, 17.84503447943221843, -1.958624548878737492 ) ) ;
#12398 = CARTESIAN_POINT ( 'NONE',  ( 7.898163624196731902, 121.8456834504061845, 1.011533665549599226 ) ) ;
#12399 = CYLINDRICAL_SURFACE ( 'NONE', #23265, 6.350000000000004974 ) ;
#12400 = CARTESIAN_POINT ( 'NONE',  ( 23.29167281398205347, 149.3519930085110161, 0.4396919384238295314 ) ) ;
#12401 = CARTESIAN_POINT ( 'NONE',  ( -5.380575101947485450, 117.2069880336854197, 0.6820287515226023389 ) ) ;
#12402 = AXIS2_PLACEMENT_3D ( 'NONE', #42022, #10044, #23225 ) ;
#12403 = DIRECTION ( 'NONE',  ( -0.4849315768086535083, -0.8745520943968250194, -1.030032898892974695E-16 ) ) ;
#12404 = CARTESIAN_POINT ( 'NONE',  ( 2.887663853482148824, 156.0927491134738716, 0.09102753749515629655 ) ) ;
#12405 = CARTESIAN_POINT ( 'NONE',  ( 7.819746389599702141, 118.9574329095587757, 1.279815391681077497 ) ) ;
#12406 = CARTESIAN_POINT ( 'NONE',  ( -0.5966991250155297966, -8.296908750894687046, 8.413794654835093922 ) ) ;
#12407 = CARTESIAN_POINT ( 'NONE',  ( 5.509056870513385995, 117.3456113441247766, -0.6578241769142348927 ) ) ;
#12408 = CARTESIAN_POINT ( 'NONE',  ( -0.4230288213599560088, 124.8375573595198063, -0.01946820596077788318 ) ) ;
#12409 = CARTESIAN_POINT ( 'NONE',  ( 6.465544251997671132, -12.29036122045927470, 0.5318397859568593233 ) ) ;
#12410 = LINE ( 'NONE', #2628, #26319 ) ;
#12411 = CARTESIAN_POINT ( 'NONE',  ( -3.210878647048973189, -8.553304832117262890, -7.794174491370510438 ) ) ;
#12412 = ADVANCED_FACE ( 'NONE', ( #4453 ), #3445, .F. ) ;
#12413 = CARTESIAN_POINT ( 'NONE',  ( 1.567127437766292486, 117.9394488752349588, 1.376223268243407682 ) ) ;
#12414 = CARTESIAN_POINT ( 'NONE',  ( -15.02280320640473121, 73.03244360434628391, 1.523999999999999577 ) ) ;
#12415 = CARTESIAN_POINT ( 'NONE',  ( 3.047145566129288330, -14.72663143740328806, 3.823360744794035870 ) ) ;
#12416 = CARTESIAN_POINT ( 'NONE',  ( 0.3827772581120965079, 119.9741034315941732, -0.6590906510345961866 ) ) ;
#12417 = CARTESIAN_POINT ( 'NONE',  ( -15.42235106321975735, 121.0727120035890323, 0.2994195231956990888 ) ) ;
#12418 = AXIS2_PLACEMENT_3D ( 'NONE', #31986, #35608, #19397 ) ;
#12419 = VERTEX_POINT ( 'NONE', #21018 ) ;
#12420 = CARTESIAN_POINT ( 'NONE',  ( 5.018852221467176022, 117.3993836729720073, -0.7012530358412483178 ) ) ;
#12421 = ORIENTED_EDGE ( 'NONE', *, *, #41542, .T. ) ;
#12422 = CARTESIAN_POINT ( 'NONE',  ( -6.060001926025549144E-14, 82.13546620154573930, 9.542986963510498366E-17 ) ) ;
#12423 = CARTESIAN_POINT ( 'NONE',  ( 4.954452526664399059, -15.13560178954495505, 4.019779494548574306 ) ) ;
#12424 = CARTESIAN_POINT ( 'NONE',  ( -20.18437654629515166, 141.3454246894093274, 1.633934361538418312 ) ) ;
#12425 = CARTESIAN_POINT ( 'NONE',  ( 22.09732278473114420, 146.2042277794223537, -1.157738048209832948 ) ) ;
#12426 = CARTESIAN_POINT ( 'NONE',  ( 3.263621351691376571, 8.939281053574255509, -3.290156819607050753 ) ) ;
#12427 = CARTESIAN_POINT ( 'NONE',  ( -58.37309112374112630, 0.2537668557392232516, -0.9020876489291813627 ) ) ;
#12428 = EDGE_LOOP ( 'NONE', ( #16088, #33322, #4572, #4154 ) ) ;
#12429 = DIRECTION ( 'NONE',  ( 0.8745520943968243532, -0.4849315768086547296, 6.829619984160642269E-16 ) ) ;
#12430 = FACE_OUTER_BOUND ( 'NONE', #25610, .T. ) ;
#12431 = CARTESIAN_POINT ( 'NONE',  ( -10.90507628433470622, 123.7747955097422476, 1.016219593014794143 ) ) ;
#12432 = CYLINDRICAL_SURFACE ( 'NONE', #8254, 0.6350000000000006750 ) ;
#12433 = CARTESIAN_POINT ( 'NONE',  ( 12.09213366837439629, 122.8144071692085504, -1.302296015248258110 ) ) ;
#12434 = CARTESIAN_POINT ( 'NONE',  ( -17.69400247866234466, 128.5843929717815115, -1.987683303373968480 ) ) ;
#12435 = CARTESIAN_POINT ( 'NONE',  ( -56.04137470801128273, 5.508142037592367757, -2.879222540163135058 ) ) ;
#12436 = VECTOR ( 'NONE', #17168, 1000.000000000000227 ) ;
#12437 = CARTESIAN_POINT ( 'NONE',  ( 11.01086703061197447, 126.1652090859982707, -0.5547642914263288816 ) ) ;
#12438 = ORIENTED_EDGE ( 'NONE', *, *, #7655, .F. ) ;
#12439 = CARTESIAN_POINT ( 'NONE',  ( -11.36144155339852446, 123.3954635094115702, -1.633191427152098196 ) ) ;
#12440 = CARTESIAN_POINT ( 'NONE',  ( 3.184821769958268600, -15.26663968290864482, 3.758507235160873261 ) ) ;
#12441 = CARTESIAN_POINT ( 'NONE',  ( -4.262962905417929882, 118.2124953749421081, -0.5347562978372674136 ) ) ;
#12442 = AXIS2_PLACEMENT_3D ( 'NONE', #38705, #32305, #23112 ) ;
#12443 = CARTESIAN_POINT ( 'NONE',  ( -47.44699234454018466, 15.94620872345373108, -7.864955498886620583E-15 ) ) ;
#12444 = CIRCLE ( 'NONE', #7007, 0.2540000000000051106 ) ;
#12445 = CARTESIAN_POINT ( 'NONE',  ( -4.877607691258805112, 117.6444329028332021, 0.8850603751916138462 ) ) ;
#12446 = CARTESIAN_POINT ( 'NONE',  ( 17.14693169618184854, 148.7218176724978775, 2.218585656167708198 ) ) ;
#12447 = DIRECTION ( 'NONE',  ( -0.7770581983690878491, 0.6294287539883980376, -5.101669463485847584E-16 ) ) ;
#12448 = CARTESIAN_POINT ( 'NONE',  ( -0.8828713250188725548, -8.991384785216279596, -8.412059017423759499 ) ) ;
#12449 = CARTESIAN_POINT ( 'NONE',  ( 15.80537369954022608, 146.5893318786020814, 0.6464893008334199331 ) ) ;
#12450 = DIRECTION ( 'NONE',  ( 9.627370216492862708E-17, 1.000000000000000000, -0.000000000000000000 ) ) ;
#12451 = CARTESIAN_POINT ( 'NONE',  ( -49.53550897992070645, 16.97828837979668748, -4.976283659310176688 ) ) ;
#12452 = DIRECTION ( 'NONE',  ( -0.8745520943968240202, 0.4849315768086553402, -6.829619984160650158E-16 ) ) ;
#12453 = AXIS2_PLACEMENT_3D ( 'NONE', #34677, #28279, #38084 ) ;
#12454 = CARTESIAN_POINT ( 'NONE',  ( -57.26626398570029863, 3.526386058942967860, 2.205039086913747948 ) ) ;
#12455 = CARTESIAN_POINT ( 'NONE',  ( -53.85529552446512724, 9.524763104166618533, 3.781023158207285295 ) ) ;
#12456 = CARTESIAN_POINT ( 'NONE',  ( -4.416771755448872128, 71.99420641645033925, 1.270000000000004903 ) ) ;
#12457 = VECTOR ( 'NONE', #6399, 999.9999999999998863 ) ;
#12458 = CARTESIAN_POINT ( 'NONE',  ( -5.664977208693889210, 65.30181249999998272, -5.033228321271210781 ) ) ;
#12459 = CARTESIAN_POINT ( 'NONE',  ( -49.01671973967525275, 18.67808020721671625, 5.174630477995037836 ) ) ;
#12460 = CARTESIAN_POINT ( 'NONE',  ( -21.90070483041515814, 151.4392833230981239, -0.2858324510978370037 ) ) ;
#12461 = ORIENTED_EDGE ( 'NONE', *, *, #4804, .F. ) ;
#12462 = CARTESIAN_POINT ( 'NONE',  ( -49.70354155341430413, 23.42381788805148091, -1.038162449038428732E-14 ) ) ;
#12463 = CARTESIAN_POINT ( 'NONE',  ( 6.931668681496168105, 121.8844402723393188, -0.1473822194997169155 ) ) ;
#12464 = CARTESIAN_POINT ( 'NONE',  ( 4.922683227735471512, 117.4111498278341799, -0.9488309096965314993 ) ) ;
#12465 = ORIENTED_EDGE ( 'NONE', *, *, #16784, .T. ) ;
#12466 = CARTESIAN_POINT ( 'NONE',  ( 2.103206696568210354, 115.7026987777287417, -1.632043270026867221 ) ) ;
#12467 = CARTESIAN_POINT ( 'NONE',  ( -9.231158399652327873, 124.2544328994657405, -0.2701740761454695661 ) ) ;
#12468 = CARTESIAN_POINT ( 'NONE',  ( 4.651167782940357931, -13.82644354294225408, 4.017274338905189701 ) ) ;
#12469 = CARTESIAN_POINT ( 'NONE',  ( -9.191685830660496492, 119.1751624949753534, 0.9473905404949719555 ) ) ;
#12470 = CARTESIAN_POINT ( 'NONE',  ( 5.749535644242491195, 78.89971493812817016, -5.036102041843245836 ) ) ;
#12471 = CIRCLE ( 'NONE', #41053, 0.6350000000000001199 ) ;
#12472 = CARTESIAN_POINT ( 'NONE',  ( 8.204617290884259617, 117.5299140688306352, 0.3545595769132393049 ) ) ;
#12473 = CARTESIAN_POINT ( 'NONE',  ( 15.76801079384962101, 146.5674410900921885, 0.4492571464743756460 ) ) ;
#12474 = CARTESIAN_POINT ( 'NONE',  ( 4.789005780339384621, 118.5266822147775940, -0.8321226176749365600 ) ) ;
#12475 = CARTESIAN_POINT ( 'NONE',  ( 0.9479787518424646064, 8.937585264489511516, -0.2400550011337005962 ) ) ;
#12476 = CARTESIAN_POINT ( 'NONE',  ( -0.8970928355478778871, 116.4604358222411236, -0.08699291512134188498 ) ) ;
#12477 = DIRECTION ( 'NONE',  ( -4.017660918040594346E-17, 1.000000000000000000, 2.376309959284834438E-19 ) ) ;
#12478 = CARTESIAN_POINT ( 'NONE',  ( -5.266289895157169814E-14, 83.56599999999998829, 1.904999999999999805 ) ) ;
#12479 = ORIENTED_EDGE ( 'NONE', *, *, #41725, .T. ) ;
#12480 = CARTESIAN_POINT ( 'NONE',  ( -8.748663343918041235, 117.9815668471614600, 0.4028670228981990342 ) ) ;
#12481 = CARTESIAN_POINT ( 'NONE',  ( -58.36978701179569384, -0.2915170370950972978, -0.01128054769438853119 ) ) ;
#12482 = CARTESIAN_POINT ( 'NONE',  ( 16.48954130525386574, 125.2933801378020888, 1.785035858276809106 ) ) ;
#12483 = CARTESIAN_POINT ( 'NONE',  ( 6.760483308329369834, 119.1290971219625021, -1.000752511853992832 ) ) ;
#12484 = CARTESIAN_POINT ( 'NONE',  ( 7.384888961195664514, 14.16877864132934839, -4.050812539764339526 ) ) ;
#12485 = CARTESIAN_POINT ( 'NONE',  ( -14.34385702226365922, 155.9958976045614349, -1.592240502911361766 ) ) ;
#12486 = CARTESIAN_POINT ( 'NONE',  ( 4.843100780571696795, 117.8277630096203836, -0.6985884806925111157 ) ) ;
#12487 = CARTESIAN_POINT ( 'NONE',  ( 5.262805716459999950, 116.4520502601644409, 1.094458988799881682 ) ) ;
#12488 = CARTESIAN_POINT ( 'NONE',  ( -14.68196552534010912, 148.8424012017631242, -0.1663232928928549959 ) ) ;
#12489 = CARTESIAN_POINT ( 'NONE',  ( -19.20654067994522762, 147.6776069388173767, -2.506343067704080774 ) ) ;
#12490 = CARTESIAN_POINT ( 'NONE',  ( 2.438853454531733966, -15.63545089637397112, 5.735818209389550226 ) ) ;
#12491 = AXIS2_PLACEMENT_3D ( 'NONE', #17584, #33592, #4425 ) ;
#12492 = CARTESIAN_POINT ( 'NONE',  ( -4.689789358878839742, 118.1651005001179158, -0.6093517961627712420 ) ) ;
#12493 = AXIS2_PLACEMENT_3D ( 'NONE', #15038, #24625, #37839 ) ;
#12494 = VERTEX_POINT ( 'NONE', #34041 ) ;
#12495 = CARTESIAN_POINT ( 'NONE',  ( 18.52244049926375880, 148.0519089404264150, 2.440181727699358927 ) ) ;
#12496 = CARTESIAN_POINT ( 'NONE',  ( -15.78437780952707215, 146.2378312303354448, -0.3154094333657934679 ) ) ;
#12497 =( BOUNDED_SURFACE ( )  B_SPLINE_SURFACE ( 3, 2, ( 
 ( #14535, #4359, #20923 ),
 ( #1362, #27544, #1153 ),
 ( #11138, #36930, #7749 ),
 ( #24334, #33946, #20715 ),
 ( #30522, #8157, #40550 ),
 ( #33739, #11348, #4563 ),
 ( #17522, #14320, #1578 ),
 ( #36654, #33040, #40068 ),
 ( #7055, #3868, #17255 ),
 ( #39857, #23635, #36235 ),
 ( #26850, #4083, #20022 ),
 ( #29627, #7265, #10861 ),
 ( #7477, #26210, #673 ),
 ( #13437, #10446, #13851 ),
 ( #463, #23850, #30247 ),
 ( #32825, #39214, #13642 ),
 ( #16834, #3439, #249 ),
 ( #20226, #6835, #29835 ),
 ( #26634, #30041, #10653 ),
 ( #36870, #23200, #26422 ) ),
 .UNSPECIFIED., .F., .F., .F. ) 
 B_SPLINE_SURFACE_WITH_KNOTS ( ( 4, 2, 2, 2, 2, 2, 2, 2, 2, 4 ),
 ( 3, 3 ),
 ( -7.203168183450570083E-17, 0.0008043714308976360541, 0.001608742861795344099, 0.002413114292693052144, 0.003217485723590760190, 0.004021857154488468235, 0.004826228585386176280, 0.006434971447181592370, 0.009652457170772425418, 0.01286994289436325760 ),
 ( 0.000000000000000000, 1.000000000000000000 ),
 .UNSPECIFIED. ) 
 GEOMETRIC_REPRESENTATION_ITEM ( )  RATIONAL_B_SPLINE_SURFACE ( (
 ( 1.000000000000000000, 0.9815197824473234078, 1.000000000000000000),
 ( 1.000000000000000000, 0.9811723635260756193, 1.000000000000000000),
 ( 1.000000000000000000, 0.9803956462535394767, 1.000000000000000000),
 ( 1.000000000000000000, 0.9775604298910611778, 1.000000000000000000),
 ( 1.000000000000000000, 0.9755054586171506559, 1.000000000000000000),
 ( 1.000000000000000000, 0.9704993482276272898, 1.000000000000000000),
 ( 1.000000000000000000, 0.9675447666325507345, 1.000000000000000000),
 ( 1.000000000000000000, 0.9610561756478790407, 1.000000000000000000),
 ( 1.000000000000000000, 0.9575813355048414799, 1.000000000000000000),
 ( 1.000000000000000000, 0.9503236772853900227, 1.000000000000000000),
 ( 1.000000000000000000, 0.9465499958463368113, 1.000000000000000000),
 ( 1.000000000000000000, 0.9387344193236741852, 1.000000000000000000),
 ( 1.000000000000000000, 0.9346745718249651613, 1.000000000000000000),
 ( 1.000000000000000000, 0.9222609948217221909, 1.000000000000000000),
 ( 1.000000000000000000, 0.9134583146195013326, 1.000000000000000000),
 ( 1.000000000000000000, 0.8860507374704946759, 1.000000000000000000),
 ( 1.000000000000000000, 0.8669451626883383222, 1.000000000000000000),
 ( 1.000000000000000000, 0.8330907799442855977, 1.000000000000000000),
 ( 1.000000000000000000, 0.8189901318545821374, 1.000000000000000000),
 ( 1.000000000000000000, 0.8121911378917013868, 1.000000000000000000) ) ) 
 REPRESENTATION_ITEM ( '' )  SURFACE ( )  );
#12498 = CARTESIAN_POINT ( 'NONE',  ( 5.237379388564934679, 115.7029491485453292, 1.024072862575109655 ) ) ;
#12499 = AXIS2_PLACEMENT_3D ( 'NONE', #40631, #40429, #21010 ) ;
#12500 = CARTESIAN_POINT ( 'NONE',  ( -1.638321535317357025, 108.1711930243730109, 4.327427591587794886 ) ) ;
#12501 = CARTESIAN_POINT ( 'NONE',  ( -8.302162399154521921, -10.86525386290528594, -1.555404731216454284 ) ) ;
#12502 = CARTESIAN_POINT ( 'NONE',  ( 8.892178686619965688, 123.2307073318660855, 0.7481024605839379227 ) ) ;
#12503 = CARTESIAN_POINT ( 'NONE',  ( 22.95957815304923599, 148.8788797244430384, -0.5134943257494377633 ) ) ;
#12504 = DIRECTION ( 'NONE',  ( -5.188838149069471174E-16, 1.699382548006136313E-16, 1.000000000000000000 ) ) ;
#12505 = AXIS2_PLACEMENT_3D ( 'NONE', #6173, #25742, #3394 ) ;
#12506 = CARTESIAN_POINT ( 'NONE',  ( -58.33175842519683840, -0.2116331208230537997, 0.2444927590478287449 ) ) ;
#12507 = EDGE_CURVE ( 'NONE', #35669, #10570, #37614, .T. ) ;
#12508 = CARTESIAN_POINT ( 'NONE',  ( -20.69909148798433662, 152.5508394022679113, -0.4136171090298727537 ) ) ;
#12509 = ORIENTED_EDGE ( 'NONE', *, *, #7121, .F. ) ;
#12510 = CARTESIAN_POINT ( 'NONE',  ( 6.495737268896391470, 120.2913924786790147, -0.9109853078430656392 ) ) ;
#12511 = CARTESIAN_POINT ( 'NONE',  ( 6.420735782905913958, -13.61083692044810434, 0.4627584258721888499 ) ) ;
#12512 = CARTESIAN_POINT ( 'NONE',  ( -6.141611553833193682, 155.3548635187015350, -0.6951709773850850427 ) ) ;
#12513 = CARTESIAN_POINT ( 'NONE',  ( 23.21309708346254652, 149.6303025714371131, 0.4895544115752262782 ) ) ;
#12514 = ORIENTED_EDGE ( 'NONE', *, *, #20230, .T. ) ;
#12515 = CARTESIAN_POINT ( 'NONE',  ( -3.426874451426485724, 1.805113900313119357, -3.130497002818263930 ) ) ;
#12516 = CARTESIAN_POINT ( 'NONE',  ( -33.20758249455312239, 49.81222039523557044, 1.523999999999994026 ) ) ;
#12517 = CARTESIAN_POINT ( 'NONE',  ( -4.801729350823258358, 117.4006813127757027, 1.015859690946131932 ) ) ;
#12518 = CARTESIAN_POINT ( 'NONE',  ( 15.21260244842765808, -1.539204351005524363E-15, 1.863006489516811765E-15 ) ) ;
#12519 = CARTESIAN_POINT ( 'NONE',  ( -14.39766717389552575, 60.87500489999897013, 1.905000000000008464 ) ) ;
#12520 = CARTESIAN_POINT ( 'NONE',  ( 6.083635286984732993, 120.8261725085448717, 0.8936664544520765974 ) ) ;
#12521 = CARTESIAN_POINT ( 'NONE',  ( 0.3943543298815788134, 25.17882533764851871, -4.623353113333005915 ) ) ;
#12522 = CARTESIAN_POINT ( 'NONE',  ( 20.09973570640914176, 152.4688535085772685, 1.548630484586873246 ) ) ;
#12523 = DIRECTION ( 'NONE',  ( -0.8745520943968245753, 0.4849315768086539524, -5.691349986800526185E-16 ) ) ;
#12525 = CARTESIAN_POINT ( 'NONE',  ( 4.984194916311421863, 158.4862278396301178, -1.425929471103634327 ) ) ;
#12524 = CARTESIAN_POINT ( 'NONE',  ( 2.274844673354063040, 107.2461735399431717, 4.729530331960789979 ) ) ;
#12526 = CARTESIAN_POINT ( 'NONE',  ( -14.27712035414131897, 128.5469532985352714, 1.439506347022430299 ) ) ;
#12527 = CARTESIAN_POINT ( 'NONE',  ( 2.854375549615681962, 5.100648791940559867, -3.633247542873777380 ) ) ;
#12528 = CARTESIAN_POINT ( 'NONE',  ( -11.39485104697116569, 118.9229013597968247, -0.8408094927682291386 ) ) ;
#12529 = CIRCLE ( 'NONE', #35650, 5.588000000000006295 ) ;
#12530 = ORIENTED_EDGE ( 'NONE', *, *, #14350, .T. ) ;
#12531 = CARTESIAN_POINT ( 'NONE',  ( -55.69906247323991266, 5.207560852731635492, 2.143283491784331307 ) ) ;
#12532 = CARTESIAN_POINT ( 'NONE',  ( -9.417214020844317801, 124.0858766813489780, 0.2349654282845520803 ) ) ;
#12533 = CARTESIAN_POINT ( 'NONE',  ( 5.593658044048013700, -13.59245692957503060, 2.833247147397068399 ) ) ;
#12534 = VECTOR ( 'NONE', #25991, 1000.000000000000227 ) ;
#12535 = DIRECTION ( 'NONE',  ( -0.8745520943968251304, 0.4849315768086532863, -5.424246918827961050E-16 ) ) ;
#12536 = CARTESIAN_POINT ( 'NONE',  ( -4.605880960340654973, 117.9546811930534744, -0.9428398339839773046 ) ) ;
#12537 = ADVANCED_FACE ( 'NONE', ( #29990 ), #23584, .T. ) ;
#12538 = CARTESIAN_POINT ( 'NONE',  ( 4.224755116449876446, 155.8535809751167562, 0.04780361979672674566 ) ) ;
#12539 = ORIENTED_EDGE ( 'NONE', *, *, #18005, .T. ) ;
#12540 = CARTESIAN_POINT ( 'NONE',  ( 12.94126367519703535, 122.7019651155717384, 1.840448779276435909 ) ) ;
#12541 = DIRECTION ( 'NONE',  ( 0.9816537812491077375, 0.1906721105965137331, 4.769617732184457412E-16 ) ) ;
#12542 = CARTESIAN_POINT ( 'NONE',  ( 20.83467972660109169, 65.95194780259438971, 5.016499999999999737 ) ) ;
#12543 = CARTESIAN_POINT ( 'NONE',  ( -13.02773564672695095, 156.9259531928012734, 0.6619068571425155145 ) ) ;
#12544 = CARTESIAN_POINT ( 'NONE',  ( 4.980372089298493954, 117.4083386159582005, -0.8694277117261164367 ) ) ;
#12545 = CARTESIAN_POINT ( 'NONE',  ( 8.030623918766011116, 158.6806155330135084, -0.07574440115180935962 ) ) ;
#12546 = CYLINDRICAL_SURFACE ( 'NONE', #26819, 0.2539999999999999480 ) ;
#12547 = CARTESIAN_POINT ( 'NONE',  ( 5.275990361836080389, 115.6909491485453145, -0.8142983086532559200 ) ) ;
#12548 = CARTESIAN_POINT ( 'NONE',  ( -46.60530155212499892, 26.17382724835484709, 0.6632222222222139418 ) ) ;
#12549 = CARTESIAN_POINT ( 'NONE',  ( 1.853238020027676125, -15.15240415584193023, 5.472168462869254846 ) ) ;
#12550 = CARTESIAN_POINT ( 'NONE',  ( -47.02779878473986486, 24.11651466984139702, 2.637840241488476511 ) ) ;
#12551 = DIRECTION ( 'NONE',  ( -0.8745520943968241312, 0.4849315768086548406, -5.691349986800536046E-16 ) ) ;
#12552 = EDGE_CURVE ( 'NONE', #32933, #18166, #30201, .T. ) ;
#12553 = CARTESIAN_POINT ( 'NONE',  ( -4.515249553929252535, 118.0822497875658712, 0.6203405485297761590 ) ) ;
#12554 = ORIENTED_EDGE ( 'NONE', *, *, #15522, .T. ) ;
#12555 = ORIENTED_EDGE ( 'NONE', *, *, #19378, .F. ) ;
#12556 = CARTESIAN_POINT ( 'NONE',  ( -23.91048590848665967, 81.84235438443283783, 1.523999999999993138 ) ) ;
#12557 = CARTESIAN_POINT ( 'NONE',  ( 3.435244954865206868, 118.5730363814739690, -0.7907002124901647555 ) ) ;
#12558 = CARTESIAN_POINT ( 'NONE',  ( -4.902456202886120273, 117.5302216577071874, -0.8631654989601054151 ) ) ;
#12559 = CARTESIAN_POINT ( 'NONE',  ( 4.605563930170307962, 117.9546322641617309, 0.9429387650545777433 ) ) ;
#12560 = CARTESIAN_POINT ( 'NONE',  ( -46.60530155212502024, 26.17382724835479735, -8.515758108943001820E-15 ) ) ;
#12561 = CARTESIAN_POINT ( 'NONE',  ( -0.7201697038422463226, 156.4767055779393559, -0.8425024029193185493 ) ) ;
#12562 = CARTESIAN_POINT ( 'NONE',  ( -2.609347773700347872, 115.7032548454379253, -1.690797176400070212 ) ) ;
#12563 = DIRECTION ( 'NONE',  ( 0.7548010569845218232, 0.6559537821943318692, 2.801824109679581255E-16 ) ) ;
#12564 = FACE_OUTER_BOUND ( 'NONE', #33881, .T. ) ;
#12565 = CARTESIAN_POINT ( 'NONE',  ( 5.344534118436166992, 116.9519127983885340, -0.7428430495679890777 ) ) ;
#12566 = CARTESIAN_POINT ( 'NONE',  ( -4.298694136813268507, 120.0471566133196291, -0.8457497992440219381 ) ) ;
#12567 = ADVANCED_FACE ( 'NONE', ( #26802 ), #14006, .F. ) ;
#12568 = CARTESIAN_POINT ( 'NONE',  ( 23.36555825341164550, 148.7788340588663800, 0.4668994608413311043 ) ) ;
#12569 = FACE_OUTER_BOUND ( 'NONE', #7299, .T. ) ;
#12570 = CARTESIAN_POINT ( 'NONE',  ( 5.938360781727902271, 56.51500000000000057, -4.381499999999999062 ) ) ;
#12571 = CARTESIAN_POINT ( 'NONE',  ( -4.274281473441157608, 3.541781053574249327, 1.790774723582081451 ) ) ;
#12573 = ORIENTED_EDGE ( 'NONE', *, *, #2230, .T. ) ;
#12572 = CARTESIAN_POINT ( 'NONE',  ( 21.60506836338281644, 151.3813297165527274, 1.270904734852022600 ) ) ;
#12574 = CARTESIAN_POINT ( 'NONE',  ( -1.039979636890616455, 104.6144662015457527, -4.722350110998245754 ) ) ;
#12575 = CARTESIAN_POINT ( 'NONE',  ( 2.733372102295486439, -15.34075898222114809, 4.536119796583970576 ) ) ;
#12576 = CARTESIAN_POINT ( 'NONE',  ( -10.65007529713519929, 155.7851685111067184, 1.746298732392691511 ) ) ;
#12577 = CARTESIAN_POINT ( 'NONE',  ( -0.5432096421966324806, 25.39095905668347797, -0.8082079942862561150 ) ) ;
#12578 = CARTESIAN_POINT ( 'NONE',  ( 0.8800754956866637668, -0.3565347152210476267, -0.4212773433312864690 ) ) ;
#12579 = ORIENTED_EDGE ( 'NONE', *, *, #39208, .T. ) ;
#12580 = VERTEX_POINT ( 'NONE', #17411 ) ;
#12581 = CARTESIAN_POINT ( 'NONE',  ( 3.333432127168501680, 112.1633951907056996, 2.855042910325920946 ) ) ;
#12582 = CARTESIAN_POINT ( 'NONE',  ( 0.000000000000000000, 0.000000000000000000, 0.000000000000000000 ) ) ;
#12583 = CARTESIAN_POINT ( 'NONE',  ( -12.52894620082573773, 152.0704867801853766, 0.9584603128924423787 ) ) ;
#12584 = CARTESIAN_POINT ( 'NONE',  ( 3.174366308151880922, 91.02546620154572565, 0.06343139340882768262 ) ) ;
#12585 = CARTESIAN_POINT ( 'NONE',  ( 3.093634585129180881, -14.37226628243755400, 4.703574289890697813 ) ) ;
#12586 = CARTESIAN_POINT ( 'NONE',  ( 8.228482648312512637, 121.2453320564195280, -0.9666412201339348309 ) ) ;
#12587 = CARTESIAN_POINT ( 'NONE',  ( -19.79373099999713403, 147.4002846799066333, -2.520905760949471386 ) ) ;
#12588 = CARTESIAN_POINT ( 'NONE',  ( -48.12298631510321201, 19.54404807545288847, -5.380074092861952373 ) ) ;
#12589 = CARTESIAN_POINT ( 'NONE',  ( 7.967454197907589908, 121.6427856937929022, 1.120273065806566271 ) ) ;
#12590 = CARTESIAN_POINT ( 'NONE',  ( -5.095652749712312080, 31.83908346630384756, 0.3959475160674749139 ) ) ;
#12591 = EDGE_CURVE ( 'NONE', #1811, #20091, #12444, .T. ) ;
#12592 = CARTESIAN_POINT ( 'NONE',  ( 14.72002613302106866, 148.8393470518043955, -0.03138755845351924589 ) ) ;
#12593 = ORIENTED_EDGE ( 'NONE', *, *, #12597, .T. ) ;
#12594 = DIRECTION ( 'NONE',  ( 6.353134868986659519E-16, -1.000000000000000000, 0.000000000000000000 ) ) ;
#12595 = ADVANCED_FACE ( 'NONE', ( #14211 ), #34222, .F. ) ;
#12596 = CYLINDRICAL_SURFACE ( 'NONE', #11639, 6.350000000000004974 ) ;
#12597 = EDGE_CURVE ( 'NONE', #7919, #20294, #37029, .T. ) ;
#12598 = CARTESIAN_POINT ( 'NONE',  ( -58.71347258051977036, -0.3150591082031195533, 0.2754856216383245182 ) ) ;
#12599 = CARTESIAN_POINT ( 'NONE',  ( -1.011143250135940530, 20.41458852336931074, 8.389224627043086358 ) ) ;
#12600 = CARTESIAN_POINT ( 'NONE',  ( 0.7201697038421175368, 156.4767055779393559, 0.8425024029193187713 ) ) ;
#12601 = CARTESIAN_POINT ( 'NONE',  ( 3.174366308151880478, 104.1064662015457287, 0.06343139340882768262 ) ) ;
#12602 = CARTESIAN_POINT ( 'NONE',  ( 23.21350185287833767, 149.6290410902582551, 0.3868015801638794993 ) ) ;
#12603 = CARTESIAN_POINT ( 'NONE',  ( -5.344534118436294889, 116.9519127983885340, 0.7428430495679891887 ) ) ;
#12604 = DIRECTION ( 'NONE',  ( -1.000000000000000000, 1.288607544181256449E-16, 0.000000000000000000 ) ) ;
#12605 = CARTESIAN_POINT ( 'NONE',  ( 7.552512487614144732, 122.4261604937442485, 0.1509171734833088807 ) ) ;
#12606 = CARTESIAN_POINT ( 'NONE',  ( 16.61465421735657699, 153.6190162071354735, 2.198628343207905900 ) ) ;
#12607 = AXIS2_PLACEMENT_3D ( 'NONE', #17620, #15050, #30829 ) ;
#12608 = CARTESIAN_POINT ( 'NONE',  ( -8.215080244096204964, -10.21703095211954704, 2.011605797521776928 ) ) ;
#12609 = CARTESIAN_POINT ( 'NONE',  ( -5.487573023729679811, 117.1580262016726692, -0.7772556852123772009 ) ) ;
#12610 = CARTESIAN_POINT ( 'NONE',  ( -0.9570916872346277859, 123.2612876230388395, -0.1732974146428331030 ) ) ;
#12611 = CARTESIAN_POINT ( 'NONE',  ( 19.68500000000000227, 71.11999999999999034, 5.016499999999999737 ) ) ;
#12612 = DIRECTION ( 'NONE',  ( -0.8745520943968240202, 0.4849315768086551737, -5.361993529360572958E-16 ) ) ;
#12613 = CARTESIAN_POINT ( 'NONE',  ( 3.486869749996455603, 104.6144662015456674, 3.351517260060684844 ) ) ;
#12614 = CARTESIAN_POINT ( 'NONE',  ( -2.857158067608712493, -4.877720491018326499, 7.942258620001617864 ) ) ;
#12615 = DIRECTION ( 'NONE',  ( -0.9998004120163608288, -4.016384292689131511E-17, -0.01997839162482749342 ) ) ;
#12616 = DIRECTION ( 'NONE',  ( 5.188838149069472160E-16, -1.699382548006136559E-16, -1.000000000000000000 ) ) ;
#12617 = CARTESIAN_POINT ( 'NONE',  ( 2.829627719599027369, -13.65247383265987757, 0.5238048331051645690 ) ) ;
#12618 = CARTESIAN_POINT ( 'NONE',  ( 0.5876368209472652149, 111.1955024190080223, -3.248215591009249170 ) ) ;
#12619 = CARTESIAN_POINT ( 'NONE',  ( -7.877688851764539812, 158.6543443936584481, 0.4710593659051899307 ) ) ;
#12620 = ORIENTED_EDGE ( 'NONE', *, *, #10423, .T. ) ;
#12621 = CARTESIAN_POINT ( 'NONE',  ( 5.965356522962838248, 77.01756249999996840, 5.016499999999999737 ) ) ;
#12622 = VERTEX_POINT ( 'NONE', #24423 ) ;
#12623 = CARTESIAN_POINT ( 'NONE',  ( -6.135835944515187101, 77.40800365160224317, -1.523999999999996247 ) ) ;
#12624 = CARTESIAN_POINT ( 'NONE',  ( 2.911953930276938607, -15.74143402046077078, 5.333341296191352221 ) ) ;
#12625 = CARTESIAN_POINT ( 'NONE',  ( -7.786520497867201129, 119.2688035297948659, 1.033142384104571265 ) ) ;
#12626 = CARTESIAN_POINT ( 'NONE',  ( 0.008945125900376662068, 117.5133074443058945, -0.4476506782301716836 ) ) ;
#12627 = CARTESIAN_POINT ( 'NONE',  ( 0.7336086519982951692, 0.2932837538699786251, -4.563195415240439701 ) ) ;
#12628 = CARTESIAN_POINT ( 'NONE',  ( -53.78496643398889177, 9.658663915604030592, -3.808424989279795003 ) ) ;
#12629 = ADVANCED_FACE ( 'NONE', ( #31239 ), #37777, .F. ) ;
#12630 = ORIENTED_EDGE ( 'NONE', *, *, #6783, .F. ) ;
#12631 = CARTESIAN_POINT ( 'NONE',  ( -58.34169784303185224, -0.2326338189567039860, -0.2089577666115286780 ) ) ;
#12632 = CARTESIAN_POINT ( 'NONE',  ( 0.4230288213598272229, 124.8375573595198063, 0.01946820596077801155 ) ) ;
#12633 = DIRECTION ( 'NONE',  ( 0.9997969816188602143, 0.0004114442613071361528, 0.02014512991857449892 ) ) ;
#12634 = B_SPLINE_SURFACE_WITH_KNOTS ( 'NONE', 3, 3, ( 
 ( #20874, #24081, #33481, #1106, #10465, #27077, #13662, #33898, #11301, #30682, #17477, #23434, #40085, #7282, #36887, #21083, #7705, #27286, #20668, #40300, #1530, #27499, #24285, #37290, #34108, #20244, #41123, #8742, #1943, #21703, #12358, #34318, #8952, #14694 ),
 ( #21918, #15110, #38137, #34948, #18101, #14902, #27905, #31307, #41550, #28113, #5772, #2579, #28542, #15541, #18726, #40707, #27699, #34728, #25345, #31736, #5559, #25134, #40912, #38348, #1736, #11503, #2151, #12142, #24489, #9166, #31521, #22122, #37494, #8318 ),
 ( #18515, #4934, #24704, #31104, #34525, #17893, #11929, #11717, #24921, #28331, #37710, #30896, #8533, #2365, #21289, #21493, #41339, #5351, #15324, #5147, #18305, #37918, #8246, #11864, #24852, #37642, #34451, #17823, #2297, #2079, #24420, #21633, #25275, #15043 ),
 ( #11647, #1871, #5284, #31669, #31453, #18447, #5487, #34659, #15257, #1668, #28476, #28045, #5706, #30822, #41480, #12288, #14623, #25060, #34038, #18234, #31236, #8467, #40638, #41054, #38280, #27626, #37849, #11432, #37425, #31030, #21845, #8672, #28260, #41267 ),
 ( #21218, #12073, #34247, #38064, #8881, #34873, #18663, #40845, #21423, #2510, #15473, #9098, #14833, #4866, #5078, #18028, #27837, #24632, #32514, #12910, #9308, #3345, #369, #19087, #3131, #13335, #6744, #9926, #22270, #15677, #35090, #16092, #26324, #35294 ),
 ( #35505, #29315, #13126, #25695, #25492, #16311, #35719, #38701, #38489, #2925, #32090, #19712, #22895, #22476, #32732, #3563, #41690, #26117, #32301, #39120, #35932, #6121, #15887, #28891, #6324, #16524, #41905, #29532, #12500, #5913, #12705, #39330, #9508, #22064 ),
 ( #25902, #18875, #31882, #38907, #157, #19295, #2720, #28681, #29098, #42117, #9720, #22685, #6527, #19503, #37532, #3775, #16734, #1773, #21118, #29738, #14309, #14733, #27945, #27735, #14943, #33731, #40746, #24527, #1981, #10136, #24325, #33938, #19930, #40542 ),
 ( #7946, #4971, #7739, #1352, #34353, #27109, #30717, #1569, #27322, #11129, #36144, #34144, #20915, #579, #11337, #23108, #4766, #8357, #40335, #24116, #6959, #14525, #21325, #37124, #17718, #32947, #14111, #18137, #5185, #30512, #11543, #23904, #27535, #40121 ),
 ( #31142, #10915, #37331, #8147, #17929, #36921, #30934, #20705, #4554, #17514, #24746, #2196, #37963, #28793, #41381, #12401, #12187, #25392, #25180, #2826, #18984, #38181, #25590, #8995, #6021, #31988, #2408, #15154, #35194, #38394, #15369, #28158, #21746, #8788 ),
 ( #41164, #15785, #8572, #9206, #31780, #11970, #22164, #19193, #34772, #21963, #32200, #38597, #41806, #24962, #34565, #34993, #12603, #9404, #22370, #35394, #6223, #5392, #21533, #2620, #3034, #15990, #15580, #40953, #5605, #11758, #37748, #18347, #5814, #31353 ),
 ( #18561, #31567, #28374, #18770, #28585, #41593, #32830, #33045, #6637, #43, #16410, #13649, #36030, #13009, #10029, #10238, #19603, #20027, #26002, #29632, #38799, #39012, #23207, #9821, #470, #26640, #26430, #33258, #39647, #36242, #20233, #6426, #22787, #35611 ),
 ( #32406, #35823, #7062, #28991, #3236, #32615, #3447, #29416, #256, #10452, #39434, #13442, #3876, #16625, #16840, #9611, #23423, #39221, #679, #12803, #36451, #7271, #25794, #29840, #42006, #13232, #26215, #23001, #19399, #6842, #4088, #22579, #19813, #16195 ) ),
 .UNSPECIFIED., .F., .F., .F.,
 ( 4, 1, 1, 1, 1, 1, 3, 4 ),
 ( 4, 1, 1, 1, 1, 1, 1, 1, 1, 1, 1, 1, 1, 1, 1, 1, 1, 1, 1, 2, 1, 1, 1, 1, 1, 1, 1, 1, 1, 1, 4 ),
 ( 0.000000000000000000, 0.1666666666666666574, 0.2500000000000000000, 0.5000000000000000000, 0.5555555555555555802, 0.7500000000000000000, 1.000000000000000000, 1.010000000000000009 ),
 ( 0.000000000000000000, 0.02126250000000000015, 0.04252500000000000030, 0.06378749999999999698, 0.08505000000000000060, 0.1063125000000000042, 0.1275749999999999940, 0.1488374999999999837, 0.1701000000000000012, 0.1913624999999999909, 0.2126250000000000084, 0.2338874999999999704, 0.2551500000000000434, 0.2764124999999999499, 0.2870437499999999864, 0.2976749999999999674, 0.3083062500000000039, 0.3189375000000000404, 0.3295687499999999659, 0.3402000000000000024, 0.4226750000000000229, 0.5051499999999999879, 0.5876249999999998419, 0.6700999999999999179, 0.7525749999999999940, 0.7938125000000000320, 0.8350499999999999590, 0.8762874999999994419, 0.9175249999999994799, 0.9587624999999999620, 1.000000000000000000 ),
 .UNSPECIFIED. ) ;
#12635 = CARTESIAN_POINT ( 'NONE',  ( -4.353257824593281811, 120.2039194668847699, 0.6262808803686856773 ) ) ;
#12636 = CARTESIAN_POINT ( 'NONE',  ( -4.466782427718574588, 71.06098887363195615, -1.269999999999994245 ) ) ;
#12637 = CARTESIAN_POINT ( 'NONE',  ( 4.214263934994704641, 119.2415290214368042, -0.8241011934941718797 ) ) ;
#12638 = CARTESIAN_POINT ( 'NONE',  ( 0.01051220311279016210, 117.9844940561907265, -0.5260736299896250356 ) ) ;
#12639 = CARTESIAN_POINT ( 'NONE',  ( -57.26626398570029863, 3.526386058942967860, -2.205039086913768820 ) ) ;
#12640 = VERTEX_POINT ( 'NONE', #27840 ) ;
#12641 = CARTESIAN_POINT ( 'NONE',  ( 16.04013775433281097, 147.3640369757652877, -0.6457813799431216806 ) ) ;
#12642 = TOROIDAL_SURFACE ( 'NONE', #33727, 3.683000000000000718, 0.5080000000000000071 ) ;
#12643 = ORIENTED_EDGE ( 'NONE', *, *, #5652, .F. ) ;
#12644 = CARTESIAN_POINT ( 'NONE',  ( -17.32761985034188967, 148.7932787949812905, -2.272318092294528746 ) ) ;
#12645 = CARTESIAN_POINT ( 'NONE',  ( 3.509229686425914707, -14.99732357267335914, 1.369000748440630799 ) ) ;
#12646 = FACE_OUTER_BOUND ( 'NONE', #24442, .T. ) ;
#12647 = EDGE_CURVE ( 'NONE', #34334, #27898, #27401, .T. ) ;
#12648 = CARTESIAN_POINT ( 'NONE',  ( -57.72731561024293967, 0.8685078910841970146, -1.009486960136972124E-14 ) ) ;
#12649 = EDGE_CURVE ( 'NONE', #32069, #3009, #36262, .T. ) ;
#12650 = CARTESIAN_POINT ( 'NONE',  ( -4.946322907344598896, 117.6258885912828447, 0.7621993455528004446 ) ) ;
#12651 = CARTESIAN_POINT ( 'NONE',  ( 15.64494829320024749, 134.9797526104055123, 2.135645317121837916 ) ) ;
#12652 = CARTESIAN_POINT ( 'NONE',  ( 0.4746723515649934888, 24.68197512780947278, 4.609222710213416896 ) ) ;
#12653 = CARTESIAN_POINT ( 'NONE',  ( 9.153275543502777722, 153.8946005065304803, 0.4698995960908564640 ) ) ;
#12654 = FACE_OUTER_BOUND ( 'NONE', #7762, .T. ) ;
#12656 = EDGE_LOOP ( 'NONE', ( #24279, #36913 ) ) ;
#12655 = CARTESIAN_POINT ( 'NONE',  ( -49.74050263075070433, 15.22813595918496432, -2.996737790144743840 ) ) ;
#12657 = DIRECTION ( 'NONE',  ( 0.8745520943968235761, -0.4849315768086558398, 0.000000000000000000 ) ) ;
#12658 = CARTESIAN_POINT ( 'NONE',  ( -15.27962295839633811, 80.49293118800726177, -1.270000000000001350 ) ) ;
#12659 = CARTESIAN_POINT ( 'NONE',  ( -49.54931586048707715, 17.00517315445653210, 5.017750506970054758 ) ) ;
#12660 = CARTESIAN_POINT ( 'NONE',  ( -23.75665686005077504, 76.91945007112674659, -1.524000000000005128 ) ) ;
#12661 = DIRECTION ( 'NONE',  ( 9.627370216492862708E-17, 1.000000000000000000, -0.000000000000000000 ) ) ;
#12662 = CARTESIAN_POINT ( 'NONE',  ( -57.76461416131697746, 2.594137363129217277, 1.330350326707359754 ) ) ;
#12663 = AXIS2_PLACEMENT_3D ( 'NONE', #6865, #22182, #3257 ) ;
#12664 = CARTESIAN_POINT ( 'NONE',  ( -10.78032506485383735, 157.9328640892066460, 0.04097195671286549268 ) ) ;
#12665 = AXIS2_PLACEMENT_3D ( 'NONE', #31757, #41144, #38370 ) ;
#12666 = ORIENTED_EDGE ( 'NONE', *, *, #2385, .F. ) ;
#12667 = CARTESIAN_POINT ( 'NONE',  ( -55.24575511360199442, 11.19612964283759560, -1.091162240856589107E-14 ) ) ;
#12668 = CARTESIAN_POINT ( 'NONE',  ( -6.001478514085576421, 121.4367562474741504, -0.1909425338979525433 ) ) ;
#12669 = DIRECTION ( 'NONE',  ( -0.6559537821943318692, 0.7548010569845216011, -4.686333752532438436E-16 ) ) ;
#12670 = EDGE_LOOP ( 'NONE', ( #35770, #6614, #12379 ) ) ;
#12671 = CARTESIAN_POINT ( 'NONE',  ( 2.827719281018770126, 115.7033332903982199, -1.571166250493931216 ) ) ;
#12672 = CARTESIAN_POINT ( 'NONE',  ( -8.534567384671404966, 123.3353292868209365, -0.2519373819028135619 ) ) ;
#12673 = CARTESIAN_POINT ( 'NONE',  ( 6.341500637990160172, -13.03620802017263536, 0.6512942508830525945 ) ) ;
#12674 = CARTESIAN_POINT ( 'NONE',  ( -21.17434475962611629, 141.7209635633906259, 1.395834004474946877 ) ) ;
#12675 = CARTESIAN_POINT ( 'NONE',  ( 5.787341484272322312, 78.89667267365581438, -5.030122981225435552 ) ) ;
#12676 = CARTESIAN_POINT ( 'NONE',  ( 22.64163882069503231, 150.6401102206664291, 0.6810593374908546771 ) ) ;
#12677 = CARTESIAN_POINT ( 'NONE',  ( 6.510425706326285145, 121.7797257153627015, 0.2058816303559638794 ) ) ;
#12678 = CARTESIAN_POINT ( 'NONE',  ( -3.174366308152012373, 71.97546620154574271, -0.06343139340882732180 ) ) ;
#12679 = CARTESIAN_POINT ( 'NONE',  ( 0.5714185265493636479, 16.70905722793067838, 0.7929698740637279863 ) ) ;
#12680 = CARTESIAN_POINT ( 'NONE',  ( -16.05840932322207948, 121.2308719818149712, -0.4813400273897940895 ) ) ;
#12681 = CARTESIAN_POINT ( 'NONE',  ( -22.98045850745952023, 78.35500052582088415, -1.524000000000005128 ) ) ;
#12682 = DIRECTION ( 'NONE',  ( -0.000000000000000000, -1.000000000000000000, -0.000000000000000000 ) ) ;
#12683 = ORIENTED_EDGE ( 'NONE', *, *, #22948, .F. ) ;
#12684 = CARTESIAN_POINT ( 'NONE',  ( -8.664938106414361130, 118.4189509008067205, 0.7014074343780984933 ) ) ;
#12685 = ORIENTED_EDGE ( 'NONE', *, *, #23345, .T. ) ;
#12686 = CARTESIAN_POINT ( 'NONE',  ( -16.46263872254443683, 83.91929436251373886, -1.270000000000002460 ) ) ;
#12687 = CARTESIAN_POINT ( 'NONE',  ( 3.992970410919064683, 117.9114980025989752, 0.8736511219775318082 ) ) ;
#12688 = CARTESIAN_POINT ( 'NONE',  ( 8.870548826841499590, 119.8693228481767932, -1.115469810106635373 ) ) ;
#12689 = CARTESIAN_POINT ( 'NONE',  ( 6.778223571145144177, 14.38247674671404752, -5.057098040585858989 ) ) ;
#12690 = CARTESIAN_POINT ( 'NONE',  ( -13.61640385012406718, 120.8017016962898396, -1.366196570323218173 ) ) ;
#12691 = CARTESIAN_POINT ( 'NONE',  ( 4.640660607179467156, 117.9806668035938486, -0.7264285073009650873 ) ) ;
#12692 = DIRECTION ( 'NONE',  ( 5.188838149069472160E-16, -1.699382548006136559E-16, -1.000000000000000000 ) ) ;
#12693 = CARTESIAN_POINT ( 'NONE',  ( -15.26897697690612077, 148.0131224598485744, -0.1773810520481277353 ) ) ;
#12694 = CARTESIAN_POINT ( 'NONE',  ( -16.55752258724323056, 151.1890201267100906, -2.396410905537823766 ) ) ;
#12695 = ADVANCED_FACE ( 'NONE', ( #25063 ), #8675, .T. ) ;
#12696 = CARTESIAN_POINT ( 'NONE',  ( 6.000997576644805598, -14.76005184138509740, 0.6970346396957283197 ) ) ;
#12697 = CARTESIAN_POINT ( 'NONE',  ( 4.973583767373020770, 117.3966162183443203, 0.9753880922370259388 ) ) ;
#12698 = EDGE_CURVE ( 'NONE', #4024, #35923, #37428, .T. ) ;
#12699 = CARTESIAN_POINT ( 'NONE',  ( -45.91718695868514288, 25.22619731686664224, -1.578102078770073469 ) ) ;
#12701 = ORIENTED_EDGE ( 'NONE', *, *, #41794, .T. ) ;
#12700 = CIRCLE ( 'NONE', #14725, 0.2540000000000010583 ) ;
#12702 = CARTESIAN_POINT ( 'NONE',  ( 17.69102400252380392, 149.9241642446907292, 2.437100891716216022 ) ) ;
#12703 = CARTESIAN_POINT ( 'NONE',  ( -12.69999999999999574, 14.60500000000000398, 1.601960477964652499E-15 ) ) ;
#12704 = DIRECTION ( 'NONE',  ( -0.4849315768086535638, -0.8745520943968251304, 5.189481155063205320E-13 ) ) ;
#12705 = CARTESIAN_POINT ( 'NONE',  ( -0.9873284109327559177, 106.8474934270474392, 4.901623504225490535 ) ) ;
#12706 = CARTESIAN_POINT ( 'NONE',  ( -5.323917895073306816, 23.39377214425099893, 6.572471397932490689 ) ) ;
#12707 = CARTESIAN_POINT ( 'NONE',  ( 15.03094698176517063, 148.9283877096812034, 1.255086756411656346 ) ) ;
#12708 = B_SPLINE_CURVE_WITH_KNOTS ( 'NONE', 3,
 ( #41243, #12048, #2057, #8649, #21610, #40823 ),
 .UNSPECIFIED., .F., .F.,
 ( 4, 2, 4 ),
 ( 0.000000000000000000, 0.0003611586812565052425, 0.0007223173625130104849 ),
 .UNSPECIFIED. ) ;
#12709 = CARTESIAN_POINT ( 'NONE',  ( 20.24728863611164442, 152.4988772720997190, -0.6427007754482428892 ) ) ;
#12710 = CARTESIAN_POINT ( 'NONE',  ( -4.981086618571428204, 117.5220611846079919, -0.8176168157337386777 ) ) ;
#12711 = CARTESIAN_POINT ( 'NONE',  ( 1.167505706004672243E-15, 11.53894877578617084, 0.000000000000000000 ) ) ;
#12712 = CARTESIAN_POINT ( 'NONE',  ( -6.900242392319385409, 117.1694300671557727, -0.09431812980450667017 ) ) ;
#12713 = ORIENTED_EDGE ( 'NONE', *, *, #7093, .T. ) ;
#12714 = CARTESIAN_POINT ( 'NONE',  ( 8.255333662909492887, 120.4554161523990103, -1.101604304946436352 ) ) ;
#12715 = CARTESIAN_POINT ( 'NONE',  ( 5.122005163076088330, -14.79606521185782420, 3.940588708504694004 ) ) ;
#12716 = CARTESIAN_POINT ( 'NONE',  ( -9.525206088249191794, 124.2661852542617709, -0.6183897905712307796 ) ) ;
#12717 = CARTESIAN_POINT ( 'NONE',  ( -20.21600168833980149, 80.16988503754176065, -1.524000000000003796 ) ) ;
#12718 = CARTESIAN_POINT ( 'NONE',  ( 22.83540780336915432, 150.4058779721138421, 0.4563057931615321361 ) ) ;
#12719 = ORIENTED_EDGE ( 'NONE', *, *, #8174, .T. ) ;
#12720 = CARTESIAN_POINT ( 'NONE',  ( 0.3994026957563919789, 5.465888722076803319, 4.619092260001838923 ) ) ;
#12721 = CARTESIAN_POINT ( 'NONE',  ( -29.82321757229076908, 71.17901112636586447, 1.523999999999992250 ) ) ;
#12722 = CARTESIAN_POINT ( 'NONE',  ( -5.000152259933599019, 117.4026936823171354, 0.8307266032655276078 ) ) ;
#12723 = CARTESIAN_POINT ( 'NONE',  ( -6.057513928997640740, 57.78499999999998948, 1.905000000000003579 ) ) ;
#12724 = AXIS2_PLACEMENT_3D ( 'NONE', #110, #35886, #6696 ) ;
#12725 = CARTESIAN_POINT ( 'NONE',  ( -4.580899860306842264, 27.87760619330545708, 0.5121266511161914892 ) ) ;
#12726 = CARTESIAN_POINT ( 'NONE',  ( -6.910925206761728390, 120.7147707202812938, 0.8460832644243309053 ) ) ;
#12727 = CARTESIAN_POINT ( 'NONE',  ( -0.5165578309945342284, 6.287656885725535716, -4.620190224396742984 ) ) ;
#12728 = CARTESIAN_POINT ( 'NONE',  ( 0.3562832388056000332, 117.2097358735305050, 0.4069867078728328091 ) ) ;
#12729 = CARTESIAN_POINT ( 'NONE',  ( -54.71920516550231639, 7.857264873378122516, -3.427457936772596803 ) ) ;
#12731 = CARTESIAN_POINT ( 'NONE',  ( 3.126689565637636115, 118.0390668470448929, -0.7034308075613265876 ) ) ;
#12730 = CARTESIAN_POINT ( 'NONE',  ( -9.925711944554160837, 78.55658865046541450, 5.016499999999999737 ) ) ;
#12732 = CARTESIAN_POINT ( 'NONE',  ( 0.02375515148176195884, 10.92298121479113426, 4.626086752085273979 ) ) ;
#12733 = CARTESIAN_POINT ( 'NONE',  ( -0.9824256172936188802, 116.9078805053781025, -0.3575799159885130196 ) ) ;
#12734 = ORIENTED_EDGE ( 'NONE', *, *, #32894, .F. ) ;
#12735 = CARTESIAN_POINT ( 'NONE',  ( -14.56142545302310332, 139.1552669279217298, 0.4455586761712632127 ) ) ;
#12736 = CARTESIAN_POINT ( 'NONE',  ( 3.788645186935202691, -14.89109417362534415, 5.282457547420531974 ) ) ;
#12737 = B_SPLINE_CURVE_WITH_KNOTS ( 'NONE', 3,
 ( #12922, #9520, #25913, #168, #3141, #23117, #15898, #19514, #6753, #3786, #22698 ),
 .UNSPECIFIED., .F., .F.,
 ( 4, 1, 1, 1, 1, 1, 1, 1, 4 ),
 ( 0.000000000000000000, 0.1249999999999979600, 0.2500000000000013878, 0.3749999999999938383, 0.4999999999999972800, 0.6249999999999980016, 0.7499999999999986677, 0.8749999999999993339, 1.000000000000000000 ),
 .UNSPECIFIED. ) ;
#12738 = CARTESIAN_POINT ( 'NONE',  ( -4.825036788391023457, 62.83146620154573014, -0.09641571798141691796 ) ) ;
#12739 = AXIS2_PLACEMENT_3D ( 'NONE', #41882, #19058, #22448 ) ;
#12740 = CARTESIAN_POINT ( 'NONE',  ( -4.603470251916389699, 118.0397685500664977, -0.8063307618835234836 ) ) ;
#12741 = CARTESIAN_POINT ( 'NONE',  ( 15.76285804746341235, 145.9067145067653541, 0.3149794173055769919 ) ) ;
#12742 = ADVANCED_FACE ( 'NONE', ( #14626 ), #31298, .T. ) ;
#12743 = VERTEX_POINT ( 'NONE', #36282 ) ;
#12744 = CARTESIAN_POINT ( 'NONE',  ( 17.39176377602785095, 131.6241255656270255, 2.296140998891703866 ) ) ;
#12745 = CARTESIAN_POINT ( 'NONE',  ( 3.009276887026297587, 50.13146620154573441, -1.210121013456480599 ) ) ;
#12746 = DIRECTION ( 'NONE',  ( 0.000000000000000000, -1.000000000000000000, 0.000000000000000000 ) ) ;
#12747 = CARTESIAN_POINT ( 'NONE',  ( -21.72212103179845855, 136.7703657609320658, 0.7093728523935391994 ) ) ;
#12748 = CARTESIAN_POINT ( 'NONE',  ( 4.791775023904364161, 117.5371554061328396, -0.9879116434822770021 ) ) ;
#12749 = AXIS2_PLACEMENT_3D ( 'NONE', #7503, #13464, #16861 ) ;
#12750 = CARTESIAN_POINT ( 'NONE',  ( 0.003746264460233156724, 116.6481217037470373, -0.1874783927187336774 ) ) ;
#12751 = FACE_OUTER_BOUND ( 'NONE', #4755, .T. ) ;
#12752 = CARTESIAN_POINT ( 'NONE',  ( -46.70260003083688360, 25.98261893038500148, 1.346190830585627607 ) ) ;
#12753 = CARTESIAN_POINT ( 'NONE',  ( -46.71787546252079437, 26.08696747599453047, 0.2117558669993397091 ) ) ;
#12754 = CARTESIAN_POINT ( 'NONE',  ( 1.846504947182619372, -15.27658449339085145, 5.385181725049428714 ) ) ;
#12755 = CARTESIAN_POINT ( 'NONE',  ( -48.04822308881583126, 19.89521662531995005, 5.294633059834397137 ) ) ;
#12756 = CARTESIAN_POINT ( 'NONE',  ( -58.68548670125471745, -0.3142138667033253507, 0.3043876634576400675 ) ) ;
#12757 = CARTESIAN_POINT ( 'NONE',  ( -4.532961034026489422, 118.0666435962141776, 0.6407912481266496707 ) ) ;
#12758 = ORIENTED_EDGE ( 'NONE', *, *, #27726, .T. ) ;
#12759 = CARTESIAN_POINT ( 'NONE',  ( -5.177913976931290740, 64.41499993257282597, 5.372100000000001430 ) ) ;
#12760 = CARTESIAN_POINT ( 'NONE',  ( 5.988741557545202987, 119.1892980795774122, -1.027262291578486808 ) ) ;
#12761 = CARTESIAN_POINT ( 'NONE',  ( -5.366896802164640157, 117.1940586887245388, -0.8977625253398613392 ) ) ;
#12762 = CARTESIAN_POINT ( 'NONE',  ( 4.700517274211256868, 117.9669807353441229, 0.8083373127690804960 ) ) ;
#12763 = CARTESIAN_POINT ( 'NONE',  ( 3.162461164278121739, -14.57801340048104777, 3.369881103115548893 ) ) ;
#12764 = CARTESIAN_POINT ( 'NONE',  ( -8.359771539777545613, 154.6912814427390970, -1.273680951853116916 ) ) ;
#12765 = AXIS2_PLACEMENT_3D ( 'NONE', #11788, #15607, #27976 ) ;
#12766 = CARTESIAN_POINT ( 'NONE',  ( -5.580495364573204498, 77.10007210032874525, -1.523999999999995802 ) ) ;
#12767 = CARTESIAN_POINT ( 'NONE',  ( -30.28638171898572651, 70.19821000523995735, -1.270000000000007345 ) ) ;
#12768 = CARTESIAN_POINT ( 'NONE',  ( 3.079207415998468811, 107.8364052097302306, -4.350788137014372836 ) ) ;
#12769 = CARTESIAN_POINT ( 'NONE',  ( -11.62460634082118283, 124.4569610989641859, -1.598101315089358154 ) ) ;
#12770 = CARTESIAN_POINT ( 'NONE',  ( 15.56076557484939116, 120.7233670659557419, 0.3109411287493940024 ) ) ;
#12771 = CARTESIAN_POINT ( 'NONE',  ( -0.004910662370487326248, 159.5928157220454295, 0.2457496255665023166 ) ) ;
#12772 = CARTESIAN_POINT ( 'NONE',  ( 12.21488373879589240, 55.24500000000000455, -5.016499999999999737 ) ) ;
#12773 = CARTESIAN_POINT ( 'NONE',  ( -4.609222696788063622, 3.091975128091568159, 0.4746723485708761459 ) ) ;
#12775 = ORIENTED_EDGE ( 'NONE', *, *, #25053, .F. ) ;
#12774 = CARTESIAN_POINT ( 'NONE',  ( 22.89058624538201059, 149.8162411397050278, 1.183733681586531139 ) ) ;
#12776 = CARTESIAN_POINT ( 'NONE',  ( 5.314256983242547250, 105.1224655745845524, -0.4585143439917250818 ) ) ;
#12777 = CARTESIAN_POINT ( 'NONE',  ( 3.848634119772940565, -15.36481979860233871, 1.996958912074897396 ) ) ;
#12778 = CARTESIAN_POINT ( 'NONE',  ( -5.879203592408529744, 119.4106843418347950, 0.9594678464101260573 ) ) ;
#12779 = CARTESIAN_POINT ( 'NONE',  ( 0.5559618826558695437, 1.427253112428326753, 0.7990736944121461516 ) ) ;
#12780 = CARTESIAN_POINT ( 'NONE',  ( 0.6613080194379835630, -2.301230296243127693, 0.7179688673762391060 ) ) ;
#12781 = ORIENTED_EDGE ( 'NONE', *, *, #2707, .F. ) ;
#12782 = EDGE_CURVE ( 'NONE', #35912, #19939, #18764, .T. ) ;
#12783 = ORIENTED_EDGE ( 'NONE', *, *, #8517, .F. ) ;
#12784 = CARTESIAN_POINT ( 'NONE',  ( -41.05189575270517111, 23.09451173561986792, 0.08466666666666186614 ) ) ;
#12785 = CARTESIAN_POINT ( 'NONE',  ( 4.012272795662530811, 117.4230540797109938, 0.9751040681224721896 ) ) ;
#12786 = CARTESIAN_POINT ( 'NONE',  ( -14.10444703556382784, 134.4521314832425389, 0.9547003412267364153 ) ) ;
#12787 = CARTESIAN_POINT ( 'NONE',  ( 3.944052607038018632, -12.86033490357471543, 2.408110524499547100 ) ) ;
#12788 = CARTESIAN_POINT ( 'NONE',  ( 11.89126842552443719, 124.3826620800890339, -1.187748846906861777 ) ) ;
#12789 = CARTESIAN_POINT ( 'NONE',  ( -18.52749500581566622, 150.2488615152233820, -2.471439233876493002 ) ) ;
#12790 = CARTESIAN_POINT ( 'NONE',  ( -47.98478927898735691, 19.46741901348697468, -5.364673458605423662 ) ) ;
#12791 = ADVANCED_FACE ( 'NONE', ( #28492 ), #15831, .T. ) ;
#12792 = CARTESIAN_POINT ( 'NONE',  ( 8.264950646253613087, 120.1599520239500549, 1.449220757049815678 ) ) ;
#12793 = CARTESIAN_POINT ( 'NONE',  ( -5.333451871256411181, 31.98409668703959596, 0.9349438309233621958 ) ) ;
#12794 = CARTESIAN_POINT ( 'NONE',  ( 7.056912283644645179, 122.0434499869739540, -0.04958421841494434906 ) ) ;
#12795 = ORIENTED_EDGE ( 'NONE', *, *, #21417, .F. ) ;
#12796 = DIRECTION ( 'NONE',  ( 0.9998004120163609398, 0.000000000000000000, 0.01997839162482749342 ) ) ;
#12797 = CARTESIAN_POINT ( 'NONE',  ( -6.437058721807690810E-14, 62.83146620154573014, 4.519164521849267879E-29 ) ) ;
#12798 = CARTESIAN_POINT ( 'NONE',  ( -58.08606908514041578, 0.8771027734568864753, 1.270208019422672807 ) ) ;
#12799 = ADVANCED_FACE ( 'NONE', ( #28906 ), #35387, .T. ) ;
#12800 = CARTESIAN_POINT ( 'NONE',  ( 9.631798221454305420, 123.4354624054469980, 1.070950170652381406 ) ) ;
#12801 = CARTESIAN_POINT ( 'NONE',  ( -6.682056005205734733E-14, 110.9644662015457328, 1.123945309419055369E-18 ) ) ;
#12802 = CARTESIAN_POINT ( 'NONE',  ( 23.41930689910511276, 142.8308675865925181, 0.4425677471174261357 ) ) ;
#12803 = CARTESIAN_POINT ( 'NONE',  ( -5.287753629968840130, 116.2229785614576798, 0.9666386099593878845 ) ) ;
#12804 = DIRECTION ( 'NONE',  ( 5.188838149069472160E-16, -1.699382548006136559E-16, -1.000000000000000000 ) ) ;
#12805 = LINE ( 'NONE', #6428, #37325 ) ;
#12806 = CARTESIAN_POINT ( 'NONE',  ( -1.409143871925768288, 33.49361554382132766, 0.6725023500899659501 ) ) ;
#12807 = CARTESIAN_POINT ( 'NONE',  ( 13.72122979561076228, 121.8522644830672590, 1.670245716993636664 ) ) ;
#12808 = EDGE_CURVE ( 'NONE', #909, #14618, #25858, .T. ) ;
#12809 = CARTESIAN_POINT ( 'NONE',  ( -0.5507456681092424144, 15.89564879194059799, -4.587442282481805300 ) ) ;
#12810 = CARTESIAN_POINT ( 'NONE',  ( 2.619848522501802446, -13.46771402114085703, -8.002427727062926266 ) ) ;
#12811 = CARTESIAN_POINT ( 'NONE',  ( -8.726771976265984776, 117.9763464038613279, -0.7462392337901883055 ) ) ;
#12812 = CARTESIAN_POINT ( 'NONE',  ( -0.7402556297412126174, 119.5055576915191580, -0.7321893670752777084 ) ) ;
#12813 = DIRECTION ( 'NONE',  ( -5.188838149069472160E-16, 1.699382548006136559E-16, 1.000000000000000000 ) ) ;
#12814 = VECTOR ( 'NONE', #7908, 1000.000000000000000 ) ;
#12815 = DIRECTION ( 'NONE',  ( 5.188838149069472160E-16, -1.699382548006136559E-16, -1.000000000000000000 ) ) ;
#12816 = CARTESIAN_POINT ( 'NONE',  ( -2.261344858989663642, 104.6144662015478701, 4.834083701540023092 ) ) ;
#12817 = CARTESIAN_POINT ( 'NONE',  ( 0.1710433496020407063, 14.98650505531991506, 4.637963194678765610 ) ) ;
#12818 = CARTESIAN_POINT ( 'NONE',  ( 4.771326357444911181, 117.9394488565474859, 1.118182396071486506 ) ) ;
#12819 = CARTESIAN_POINT ( 'NONE',  ( -14.80692295515835255, 78.04183178746349370, -5.016499999999999737 ) ) ;
#12820 = CARTESIAN_POINT ( 'NONE',  ( 2.906309357581933650, -13.72804873580029472, 0.7610837935892840189 ) ) ;
#12821 = EDGE_CURVE ( 'NONE', #30637, #31609, #28830, .T. ) ;
#12822 = CARTESIAN_POINT ( 'NONE',  ( 0.8718816746734422418, 108.7514562038770976, -4.146788293844217321 ) ) ;
#12823 = CARTESIAN_POINT ( 'NONE',  ( -1.919474982883727199, 116.7789519286944966, 0.2705014076049042648 ) ) ;
#12824 = ORIENTED_EDGE ( 'NONE', *, *, #14746, .T. ) ;
#12825 = CARTESIAN_POINT ( 'NONE',  ( 5.871452009091292723, 77.01756249999996840, 5.016499999999999737 ) ) ;
#12826 = ORIENTED_EDGE ( 'NONE', *, *, #27964, .T. ) ;
#12827 = CARTESIAN_POINT ( 'NONE',  ( -42.03620417734866521, 22.24401450883890519, -1.718184518067733979 ) ) ;
#12828 = CARTESIAN_POINT ( 'NONE',  ( 5.825557336981400880, -14.92341722037543406, 1.564612827344095569 ) ) ;
#12829 = CARTESIAN_POINT ( 'NONE',  ( -13.44120003175033595, 122.0388263298542739, 1.206224284286116832 ) ) ;
#12830 = CARTESIAN_POINT ( 'NONE',  ( 4.918710253154888967, 117.7409041207840090, -0.6764595669667287092 ) ) ;
#12831 = ADVANCED_FACE ( 'NONE', ( #29760 ), #25207, .F. ) ;
#12832 = CARTESIAN_POINT ( 'NONE',  ( 4.224370802630715183, -2.505441902618962935, 1.893578447770203566 ) ) ;
#12833 = CARTESIAN_POINT ( 'NONE',  ( -56.39031313087512132, 4.472451144598750261, -2.570725850350818131 ) ) ;
#12834 = EDGE_LOOP ( 'NONE', ( #29289, #39672, #27833, #41076 ) ) ;
#12835 = CARTESIAN_POINT ( 'NONE',  ( -58.60151899684548482, -0.7129426177418396460, -0.1461293658723255284 ) ) ;
#12836 = CARTESIAN_POINT ( 'NONE',  ( 0.3568539549765675778, 120.5507043431651510, 0.5637235919965009057 ) ) ;
#12837 = CARTESIAN_POINT ( 'NONE',  ( -4.647465358394767598, 117.9312056069267669, 0.7793557571712189658 ) ) ;
#12838 = CARTESIAN_POINT ( 'NONE',  ( -0.5597765207468382576, 119.9180165495073283, 0.4599786748625145361 ) ) ;
#12839 = DIRECTION ( 'NONE',  ( -4.017660918040594346E-17, 1.000000000000000000, 2.376309959284834438E-19 ) ) ;
#12840 = AXIS2_PLACEMENT_3D ( 'NONE', #29096, #38906, #19086 ) ;
#12841 = CARTESIAN_POINT ( 'NONE',  ( 11.72911894083922668, 122.8035986606355152, -1.269020613264101982 ) ) ;
#12842 = AXIS2_PLACEMENT_3D ( 'NONE', #9613, #2622, #41809 ) ;
#12843 = CARTESIAN_POINT ( 'NONE',  ( -5.843718602766688086, 118.4234969239897453, -1.100938688348692018 ) ) ;
#12844 = CARTESIAN_POINT ( 'NONE',  ( -58.09657527255103560, 0.9821181129459344294, -1.359330230256445393 ) ) ;
#12845 = ORIENTED_EDGE ( 'NONE', *, *, #7939, .F. ) ;
#12846 = CARTESIAN_POINT ( 'NONE',  ( 4.596726809479003251, 118.0790520653858806, -0.5325700990769507426 ) ) ;
#12847 = CARTESIAN_POINT ( 'NONE',  ( 2.723409340394662870, 120.7183352303693340, -0.2545450062501626309 ) ) ;
#12848 = ORIENTED_EDGE ( 'NONE', *, *, #20710, .F. ) ;
#12849 = CARTESIAN_POINT ( 'NONE',  ( -11.09706570755290578, 123.3376105302527037, -1.576947150105312279 ) ) ;
#12850 = CARTESIAN_POINT ( 'NONE',  ( 2.381491173306826248, -15.37068253093559811, 4.932168965620852497 ) ) ;
#12851 = CARTESIAN_POINT ( 'NONE',  ( -2.738177118692914025, 105.1243822654267177, -4.587785415214179707 ) ) ;
#12852 = CARTESIAN_POINT ( 'NONE',  ( -8.480639930781094904, 68.51064353654967931, 1.270000000000002460 ) ) ;
#12853 = CARTESIAN_POINT ( 'NONE',  ( -4.841216625639615856, 117.7365175972573610, 0.8492818512291455679 ) ) ;
#12854 = CARTESIAN_POINT ( 'NONE',  ( 8.045112435069260215, 121.5393406094847819, 1.176871282714906375 ) ) ;
#12855 = CARTESIAN_POINT ( 'NONE',  ( -14.39766717389551687, 57.78499999999998948, -1.905000000000000027 ) ) ;
#12856 = CARTESIAN_POINT ( 'NONE',  ( -1.648064503646425649, 29.87956589480163316, -4.325937074807028715 ) ) ;
#12857 = CARTESIAN_POINT ( 'NONE',  ( 1.577167647222550650, 156.2580631240469415, 0.1709568888171393575 ) ) ;
#12858 = DIRECTION ( 'NONE',  ( 0.5149185422762164732, -0.8572391118119474518, -5.501763788286270478E-15 ) ) ;
#12859 = ADVANCED_FACE ( 'NONE', ( #4266 ), #24847, .T. ) ;
#12860 = CIRCLE ( 'NONE', #10134, 0.7620000000000015650 ) ;
#12861 = CARTESIAN_POINT ( 'NONE',  ( -47.89521659674720411, 15.90546175020217312, -0.7967971578063902660 ) ) ;
#12862 = AXIS2_PLACEMENT_3D ( 'NONE', #30267, #1108, #692 ) ;
#12863 = CARTESIAN_POINT ( 'NONE',  ( -0.7152400940742318358, 118.1588900943969520, 0.8748708461251418766 ) ) ;
#12864 = CARTESIAN_POINT ( 'NONE',  ( -46.75005564411527104, 25.87286441723897568, -1.401665496903889085 ) ) ;
#12865 = CARTESIAN_POINT ( 'NONE',  ( -51.05584078844552920, 14.55899147689505391, 4.676820903699452359 ) ) ;
#12866 = CARTESIAN_POINT ( 'NONE',  ( -11.34554992887676406, 77.73165686004495001, 1.524000000000000687 ) ) ;
#12867 = CARTESIAN_POINT ( 'NONE',  ( 3.456281358658134906, 50.63946620154572997, 1.847419665314800064 ) ) ;
#12868 = CARTESIAN_POINT ( 'NONE',  ( -56.03617394834085985, 6.499552843647532718, 2.676235688315251604 ) ) ;
#12869 = CARTESIAN_POINT ( 'NONE',  ( -57.83637253161431602, 2.237724655402451024, 1.757929103219288747 ) ) ;
#12870 = CARTESIAN_POINT ( 'NONE',  ( -0.9174821693852864835, 116.5216256635990391, 0.1124321123350598417 ) ) ;
#12871 = ORIENTED_EDGE ( 'NONE', *, *, #17483, .T. ) ;
#12872 = CARTESIAN_POINT ( 'NONE',  ( -53.84631020977099780, 15.55534180641097386, -0.3033304672099482735 ) ) ;
#12873 = CARTESIAN_POINT ( 'NONE',  ( 6.033788598149758542, 121.4449637489673677, 0.07283107479205253032 ) ) ;
#12874 = EDGE_CURVE ( 'NONE', #12419, #41231, #16192, .T. ) ;
#12875 = ORIENTED_EDGE ( 'NONE', *, *, #2142, .F. ) ;
#12876 = CARTESIAN_POINT ( 'NONE',  ( 2.277049499775069652, 115.7026830795285690, -1.618583747791560778 ) ) ;
#12877 = CARTESIAN_POINT ( 'NONE',  ( -15.52804360843209253, 147.5314071815517138, -0.4383331365498628340 ) ) ;
#12878 = CARTESIAN_POINT ( 'NONE',  ( 3.788645186935202691, -14.89109417362534415, 5.282457547420531974 ) ) ;
#12879 = CARTESIAN_POINT ( 'NONE',  ( -5.881556420379579819, 118.2031694463412634, 0.8113220510518369677 ) ) ;
#12880 = DIRECTION ( 'NONE',  ( 0.8745520943968240202, -0.4849315768086553402, 6.829619984160650158E-16 ) ) ;
#12881 = CARTESIAN_POINT ( 'NONE',  ( 16.82892344227259329, 155.2408147041404050, 0.5439083615366223645 ) ) ;
#12882 = ADVANCED_FACE ( 'NONE', ( #37360 ), #8180, .T. ) ;
#12883 = CARTESIAN_POINT ( 'NONE',  ( 15.71945467201891766, 145.6824202290839025, 0.4486337225308515975 ) ) ;
#12884 = CARTESIAN_POINT ( 'NONE',  ( 5.276629905794020026, 115.6909491485453145, -0.8098420342951175854 ) ) ;
#12885 = CARTESIAN_POINT ( 'NONE',  ( 0.4552753346810295421, 10.21665217803766268, -0.8656630863528285147 ) ) ;
#12886 = CARTESIAN_POINT ( 'NONE',  ( -13.41573142586496559, 156.9389434127184018, -0.3962193537810600463 ) ) ;
#12887 = CARTESIAN_POINT ( 'NONE',  ( -29.91360363449004822, 70.04874496952839991, -1.270000000000007123 ) ) ;
#12888 = PLANE ( 'NONE',  #18647 ) ;
#12889 = ORIENTED_EDGE ( 'NONE', *, *, #25006, .T. ) ;
#12890 = CARTESIAN_POINT ( 'NONE',  ( 8.615066246506550840, 118.4883731374293916, 1.081964075605263975 ) ) ;
#12891 = ORIENTED_EDGE ( 'NONE', *, *, #8373, .T. ) ;
#12892 = CARTESIAN_POINT ( 'NONE',  ( -58.36458372496356617, -0.2806544840891243009, -0.08969953854032418350 ) ) ;
#12893 = CARTESIAN_POINT ( 'NONE',  ( 15.28824200187825788, 154.8698957928756954, 2.015933685939941267 ) ) ;
#12894 = CARTESIAN_POINT ( 'NONE',  ( 5.881924083617287913, 119.0696708348911699, -0.9594134845634215703 ) ) ;
#12895 = CARTESIAN_POINT ( 'NONE',  ( -6.994280559954464849, 7.701067304790329082, -4.726517096957497444 ) ) ;
#12896 = CARTESIAN_POINT ( 'NONE',  ( -21.80715381475374315, 148.2155681941778482, -2.148825447453798443 ) ) ;
#12897 = CARTESIAN_POINT ( 'NONE',  ( 4.801507292439965546, 117.8464550438453529, -0.7717428139693086608 ) ) ;
#12898 = CARTESIAN_POINT ( 'NONE',  ( -8.305181614181256222, 72.61062586887042869, 1.270000000000002682 ) ) ;
#12899 = AXIS2_PLACEMENT_3D ( 'NONE', #32295, #16085, #29937 ) ;
#12900 = CARTESIAN_POINT ( 'NONE',  ( -13.59242215834144751, 150.2357272821285221, -0.2218801189746051894 ) ) ;
#12901 = CARTESIAN_POINT ( 'NONE',  ( -17.74096168611294289, 140.4837523222294351, -2.437162785362842143 ) ) ;
#12903 = CARTESIAN_POINT ( 'NONE',  ( 4.157678856868515460, -15.71065181052187754, 4.128466586810772831 ) ) ;
#12902 = AXIS2_PLACEMENT_3D ( 'NONE', #19730, #25922, #38719 ) ;
#12904 = LINE ( 'NONE', #13118, #16557 ) ;
#12905 = CARTESIAN_POINT ( 'NONE',  ( -44.90991502375803890, 23.16658271142636139, -2.247441098035906748 ) ) ;
#12906 = VERTEX_POINT ( 'NONE', #18799 ) ;
#12907 = CARTESIAN_POINT ( 'NONE',  ( 12.38071862475238660, 124.1810962131942517, 1.797420231217670139 ) ) ;
#12908 = CARTESIAN_POINT ( 'NONE',  ( -4.897655256226316034, 56.53910281269282478, 5.081330806033710346 ) ) ;
#12909 = DIRECTION ( 'NONE',  ( 5.188838149069472160E-16, -1.699382548006136559E-16, -1.000000000000000000 ) ) ;
#12910 = CARTESIAN_POINT ( 'NONE',  ( -2.292460607442647014, 118.3648483361698851, 0.7949187631362103490 ) ) ;
#12911 = CARTESIAN_POINT ( 'NONE',  ( 4.673167956146812685, 25.32871407960522347, 7.020956665532097851 ) ) ;
#12912 = CARTESIAN_POINT ( 'NONE',  ( 5.875838086862335885, 121.3091694753028520, 0.5415667612380998808 ) ) ;
#12913 = CARTESIAN_POINT ( 'NONE',  ( 18.18789719519565296, 154.1160801429439857, -0.6523539814353513933 ) ) ;
#12914 = LINE ( 'NONE', #13131, #41023 ) ;
#12915 = B_SPLINE_CURVE_WITH_KNOTS ( 'NONE', 3,
 ( #18992, #31996, #40084, #3886, #23012, #20453, #897, #4310, #27076, #30060, #36040, #39445, #26652, #13454, #3671, #17057, #23867, #7493, #17476, #33480 ),
 .UNSPECIFIED., .F., .F.,
 ( 4, 2, 2, 2, 2, 2, 2, 2, 2, 4 ),
 ( -5.999999999764871059E-08, 0.0007881984188580538637, 0.001576456837716104986, 0.002364715256574156325, 0.003152973675432207881, 0.003941232094290259003, 0.004729490513148310558, 0.006306007350864415405, 0.009459041026296625965, 0.01261207470172883739 ),
 .UNSPECIFIED. ) ;
#12916 = CYLINDRICAL_SURFACE ( 'NONE', #1822, 0.2539999999999962288 ) ;
#12917 = PRODUCT_DEFINITION_CONTEXT ( 'detailed design', #1237, 'design' ) ;
#12918 = CIRCLE ( 'NONE', #23797, 2.540000000000002256 ) ;
#12919 = CARTESIAN_POINT ( 'NONE',  ( -22.75657594704724929, 137.3797884758947703, -0.4311216471409407558 ) ) ;
#12920 = VERTEX_POINT ( 'NONE', #19430 ) ;
#12921 = CARTESIAN_POINT ( 'NONE',  ( 6.528646965957701553, 120.3692086654437361, -0.8958864263995045540 ) ) ;
#12922 = CARTESIAN_POINT ( 'NONE',  ( 23.36555825341164550, 148.7788340588663800, 0.4668994608413311043 ) ) ;
#12923 = CARTESIAN_POINT ( 'NONE',  ( -15.47370139510886666, 143.5853813351167219, -1.046079274478293852 ) ) ;
#12924 = CARTESIAN_POINT ( 'NONE',  ( 3.965039388734942882, -13.93407386435618989, 4.333124597978631698 ) ) ;
#12925 = CARTESIAN_POINT ( 'NONE',  ( 13.17422243436029916, 17.14500000000093394, 5.016499999999999737 ) ) ;
#12926 = CARTESIAN_POINT ( 'NONE',  ( 23.11127252101355722, 149.9001116002701224, 0.4618182267416076070 ) ) ;
#12927 = EDGE_CURVE ( 'NONE', #11069, #11444, #25206, .T. ) ;
#12928 = EDGE_LOOP ( 'NONE', ( #35022, #28610, #1608 ) ) ;
#12929 = CARTESIAN_POINT ( 'NONE',  ( -2.707926769430928804, 11.08828375386998033, -3.745406074561137721 ) ) ;
#12930 = CARTESIAN_POINT ( 'NONE',  ( 3.301553950842845531, 105.1237708183731172, 4.201341878287736087 ) ) ;
#12931 = LINE ( 'NONE', #32113, #39157 ) ;
#12932 = CARTESIAN_POINT ( 'NONE',  ( -4.466782427718574588, 71.06098887363195615, -1.269999999999994245 ) ) ;
#12933 = CARTESIAN_POINT ( 'NONE',  ( -7.864245281215539229, 122.2955428227499937, 0.4135678702982136246 ) ) ;
#12934 = CARTESIAN_POINT ( 'NONE',  ( -2.426139246716550346, 10.07336736126799437, 3.943011612146583023 ) ) ;
#12935 = CARTESIAN_POINT ( 'NONE',  ( 14.92386488306798675, 121.2513550155162960, 1.224273950129214805 ) ) ;
#12936 = CARTESIAN_POINT ( 'NONE',  ( -0.07157677170311223247, 110.3683645023726569, 3.581994345755902032 ) ) ;
#12938 = CARTESIAN_POINT ( 'NONE',  ( 2.167900391131057702, 117.8876587302075194, -0.6265904732959521883 ) ) ;
#12937 = CARTESIAN_POINT ( 'NONE',  ( 3.177488185987922709, -14.13217061847354472, 2.003775387181677026 ) ) ;
#12939 = CARTESIAN_POINT ( 'NONE',  ( -1.889208318266999198, 10.27326514537015534, 4.227218769941996968 ) ) ;
#12940 = CARTESIAN_POINT ( 'NONE',  ( -22.60558431049205197, 149.7032342875954498, -1.528355188309250323 ) ) ;
#12941 = ORIENTED_EDGE ( 'NONE', *, *, #1190, .T. ) ;
#12942 = CARTESIAN_POINT ( 'NONE',  ( -7.056912283644773964, 122.0434499869739540, 0.04958421841494448784 ) ) ;
#12943 = CARTESIAN_POINT ( 'NONE',  ( 6.101987814473650573, -12.39306998090061640, 0.4902605208062851827 ) ) ;
#12944 = CIRCLE ( 'NONE', #14303, 0.2539999999999981162 ) ;
#12945 = CARTESIAN_POINT ( 'NONE',  ( -23.49500000000000455, 71.11999999999999034, 5.016499999999999737 ) ) ;
#12946 = ORIENTED_EDGE ( 'NONE', *, *, #25522, .T. ) ;
#12947 = CARTESIAN_POINT ( 'NONE',  ( 19.66043293732242603, 148.5147687316951135, 2.511426770373371031 ) ) ;
#12948 = CARTESIAN_POINT ( 'NONE',  ( 3.527324519276021420, 50.63946620154572997, -1.707870599815379586 ) ) ;
#12949 = FACE_OUTER_BOUND ( 'NONE', #28274, .T. ) ;
#12950 = CARTESIAN_POINT ( 'NONE',  ( -3.161282452094362316, 159.3671203531505114, 0.6484678655804385627 ) ) ;
#12951 = CIRCLE ( 'NONE', #3465, 0.7619999999999976792 ) ;
#12952 = CARTESIAN_POINT ( 'NONE',  ( 3.792432603185356133, 116.7736770086926867, -0.1904249565637310959 ) ) ;
#12953 = CARTESIAN_POINT ( 'NONE',  ( -5.011781081284850003, 115.7029491485453576, -1.398622308649235979 ) ) ;
#12954 = CARTESIAN_POINT ( 'NONE',  ( -50.93622740537085747, 14.57546966384534848, 4.560176109731806982 ) ) ;
#12955 = CARTESIAN_POINT ( 'NONE',  ( -46.93283292234357162, 25.30718002661817323, 1.635697237164823514 ) ) ;
#12956 = AXIS2_PLACEMENT_3D ( 'NONE', #10632, #14033, #10839 ) ;
#12957 = CARTESIAN_POINT ( 'NONE',  ( -4.973857814267949706, 117.3975374627346326, -0.9751189716041865907 ) ) ;
#12958 = CARTESIAN_POINT ( 'NONE',  ( -43.10982161678889213, 22.52422253607401359, 1.888110242252979631 ) ) ;
#12959 = CARTESIAN_POINT ( 'NONE',  ( -7.994219716368544226, 68.36415334912796027, -1.269999999999995577 ) ) ;
#12960 = CARTESIAN_POINT ( 'NONE',  ( -4.537430495507082107, 118.0683159900091539, 0.6374709560671608655 ) ) ;
#12961 = CARTESIAN_POINT ( 'NONE',  ( -58.28497307353763546, -0.1385909279409125450, -0.01567725181050762251 ) ) ;
#12962 = B_SPLINE_SURFACE_WITH_KNOTS ( 'NONE', 3, 3, ( 
 ( #4287, #34087, #13638, #24056, #17455, #30454, #4707, #876, #14053, #30036, #7262, #39637 ),
 ( #1298, #14254, #37071, #13848, #26847, #23414, #10650, #26630, #20851, #21061, #23846, #27057 ),
 ( #20641, #40065, #4916, #20432, #29832, #1508, #670, #4495, #20222, #33249, #4078, #36867 ),
 ( #39854, #7682, #27263, #40279, #11072, #23631, #33460, #14463, #17251, #7889, #8718, #28091 ),
 ( #38323, #14880, #41102, #1715, #34704, #21680, #9142, #11478, #11908, #5750, #15516, #41525 ),
 ( #21893, #24467, #40686, #5533, #22099, #34922, #37471, #28307, #2555, #31496, #40891, #28518 ),
 ( #38111, #18491, #8298, #25318, #21267, #24897, #35128, #14671, #2344, #18702, #17870, #34296 ),
 ( #15301, #41314, #8926, #12119, #5126, #30871, #18077, #37896, #27675, #31080, #25108, #31713 ),
 ( #1919, #5328, #12330, #27882, #11695, #24681, #37689, #8511, #21470, #34500, #18282, #31283 ),
 ( #2126, #15090, #20125, #4185, #3978, #10757, #33355, #29938, #16726, #23739, #12536, #32130 ),
 ( #16939, #9342, #15924, #776, #5955, #22305, #2961, #25728, #28922, #19922, #17148, #13753 ),
 ( #18914, #31924, #26748, #36353, #7167, #10554, #19124, #6953, #35329, #25525, #15716, #3767 ),
 ( #33151, #39759, #6156, #41940, #28720, #12740, #2761, #23523, #30149, #571, #29730, #38735 ),
 ( #13545, #990, #9543, #41731, #36550, #38525, #10345, #22513, #35544, #13955, #26536, #32938 ),
 ( #39539, #23316, #7370, #20328, #26953, #39966, #40788, #11801, #30562, #27574, #4810, #5016 ),
 ( #33777, #17761, #20539, #11379, #40582, #27988, #30347, #30761, #24571, #34391, #18179, #5225 ),
 ( #1196, #17359, #24366, #14986, #11589, #14156, #17976, #21365, #31181, #33569, #7792, #27159 ),
 ( #21159, #2022, #14777, #23952, #37373, #40173, #10965, #40380, #27777, #36759, #37577, #40996 ),
 ( #8404, #7578, #4403, #36970, #8190, #1611, #20753, #34190, #1401, #30974, #33982, #1814 ),
 ( #27369, #4605, #17561, #14569, #14357, #11175, #24160, #37169, #7991, #20961, #15199, #12441 ),
 ( #41209, #8827, #2451, #34814, #38223, #22414, #22206, #9250, #38434, #25435, #28202, #35237 ),
 ( #28836, #38006, #25219, #12011, #2240, #34603, #22004, #6062, #19022, #32029, #25004, #21787 ),
 ( #5648, #21576, #15828, #6266, #18812, #35036, #18606, #15617, #5856, #35441, #15411, #24790 ),
 ( #29035, #28622, #5431, #8612, #19236, #31821, #31612, #28416, #9039, #2659, #41634, #2868 ) ),
 .UNSPECIFIED., .F., .F., .F.,
 ( 4, 2, 2, 2, 2, 2, 2, 2, 2, 2, 2, 4 ),
 ( 4, 2, 1, 2, 1, 2, 4 ),
 ( 0.000000000000000000, 0.1320131134996915812, 0.1980196702495373717, 0.2640262269993831623, 0.3918780277393359990, 0.4558039281093124173, 0.5197298284792888357, 0.5807783984393792842, 0.6418269683994697328, 0.7639241083196507409, 0.8819620541598254260, 1.000000000000000000 ),
 ( 0.000000000000000000, 0.1250000000000000000, 0.2500000000000000000, 0.5000000000000000000, 0.7500000000000000000, 0.8750000000000000000, 1.000000000000000000 ),
 .UNSPECIFIED. ) ;
#12963 = ORIENTED_EDGE ( 'NONE', *, *, #7169, .F. ) ;
#12964 = DIRECTION ( 'NONE',  ( -1.000000000000000000, 0.000000000000000000, 0.000000000000000000 ) ) ;
#12965 = CARTESIAN_POINT ( 'NONE',  ( -5.985785924374277478, 119.2914591321808189, -1.266711398467851746 ) ) ;
#12966 = CARTESIAN_POINT ( 'NONE',  ( -5.733418603097514499, 118.4539739381501988, -0.6622650514401647870 ) ) ;
#12968 = CARTESIAN_POINT ( 'NONE',  ( 4.815183644347338365, 117.8246314654618345, 0.8831286348090380267 ) ) ;
#12967 = VECTOR ( 'NONE', #1091, 1000.000000000000000 ) ;
#12969 = DIRECTION ( 'NONE',  ( -5.463695987328526437E-16, -1.000000000000000000, -1.672774450599033775E-31 ) ) ;
#12970 = CARTESIAN_POINT ( 'NONE',  ( -4.434842451389515716, 120.7762672505206041, -0.5587804529453966884 ) ) ;
#12971 = CARTESIAN_POINT ( 'NONE',  ( -1.943362973813288486, 115.7022440231138063, -1.718213888689203772 ) ) ;
#12972 = DIRECTION ( 'NONE',  ( -1.000000000000000000, 0.000000000000000000, 0.000000000000000000 ) ) ;
#12973 = CARTESIAN_POINT ( 'NONE',  ( 14.39766717389552042, 60.02151067229126369, -1.904999999999999583 ) ) ;
#12974 = CARTESIAN_POINT ( 'NONE',  ( 7.117363349590072552, 122.4243137415680280, 0.03262055675632266616 ) ) ;
#12975 = CARTESIAN_POINT ( 'NONE',  ( -2.572680461994368173, 120.1437993944865354, -0.5932419562244880540 ) ) ;
#12976 = SURFACE_STYLE_FILL_AREA ( #19158 ) ;
#12977 = CARTESIAN_POINT ( 'NONE',  ( -0.02400040557479403425, 156.7459281804771365, 1.201078436782489822 ) ) ;
#12978 = CARTESIAN_POINT ( 'NONE',  ( -2.448307479368688977, 115.7029487053374623, 1.604658189596191109 ) ) ;
#12979 = CARTESIAN_POINT ( 'NONE',  ( -0.0007138457988933175546, 156.3034662015457741, 0.03572376281290677580 ) ) ;
#12980 = CARTESIAN_POINT ( 'NONE',  ( -2.646443841375008432, -8.127818987380491578, -3.789199236247322133 ) ) ;
#12982 = VERTEX_POINT ( 'NONE', #28823 ) ;
#12981 = CARTESIAN_POINT ( 'NONE',  ( 15.39807837497266618, 121.0727120035890323, 0.9152850519163395759 ) ) ;
#12983 = CARTESIAN_POINT ( 'NONE',  ( 4.546337323837841282, 104.6144662015457527, -1.651695662123250807 ) ) ;
#12984 = CARTESIAN_POINT ( 'NONE',  ( 2.120377039319510715, -15.39027815159008128, 5.169171589912422426 ) ) ;
#12985 = CARTESIAN_POINT ( 'NONE',  ( -18.94087081963961694, 148.8558894138562039, 1.735487911102015168 ) ) ;
#12986 = CARTESIAN_POINT ( 'NONE',  ( 0.2491751845298053603, 0.8914985761586250446, 0.9476022430964140542 ) ) ;
#12987 = CARTESIAN_POINT ( 'NONE',  ( -6.905604733424429931, 117.2797055272990292, -0.4577529590079176258 ) ) ;
#12988 = CARTESIAN_POINT ( 'NONE',  ( -0.4068859638909740339, 2.017459551269393359, -0.8868740919469698669 ) ) ;
#12989 = ORIENTED_EDGE ( 'NONE', *, *, #17360, .F. ) ;
#12990 = CARTESIAN_POINT ( 'NONE',  ( -46.53889185657398286, 18.10826295091780835, 1.459106928557426963 ) ) ;
#12991 = CARTESIAN_POINT ( 'NONE',  ( 3.839037681459631646, 115.3331674797404247, 1.733041430519539183 ) ) ;
#12992 = APPLICATION_PROTOCOL_DEFINITION ( 'draft international standard', 'automotive_design', 1998, #28694 ) ;
#12993 = CARTESIAN_POINT ( 'NONE',  ( -6.388910139315926884, 155.4084287100276072, 0.7748799927007739008 ) ) ;
#12994 = CARTESIAN_POINT ( 'NONE',  ( 2.004955844419833877, -15.09631637516548075, 5.820374350103214134 ) ) ;
#12995 = CARTESIAN_POINT ( 'NONE',  ( 15.71777585039850500, 134.9797526104055123, -1.508943449597504483 ) ) ;
#12996 = CARTESIAN_POINT ( 'NONE',  ( -15.71367270535934857, 153.2725199748809928, -2.344280857665636209 ) ) ;
#12997 = DIRECTION ( 'NONE',  ( 5.188838149069472160E-16, -1.699382548006136559E-16, -1.000000000000000000 ) ) ;
#12998 = CIRCLE ( 'NONE', #19131, 16.60960244842765832 ) ;
#12999 = CARTESIAN_POINT ( 'NONE',  ( 7.851578091136403259, 122.2417759690833066, 0.7721127453851787115 ) ) ;
#13000 = CARTESIAN_POINT ( 'NONE',  ( -0.9584988517251393780, 37.03984800159950908, 1.311833450704142034 ) ) ;
#13001 = CARTESIAN_POINT ( 'NONE',  ( 15.81858318527952179, 146.5893318786020814, -0.01456738144011935666 ) ) ;
#13002 = ORIENTED_EDGE ( 'NONE', *, *, #27922, .T. ) ;
#13003 = FACE_OUTER_BOUND ( 'NONE', #18932, .T. ) ;
#13004 = AXIS2_PLACEMENT_3D ( 'NONE', #9762, #3383, #1455 ) ;
#13005 = DIRECTION ( 'NONE',  ( 5.188838149069472160E-16, -1.699382548006136559E-16, -1.000000000000000000 ) ) ;
#13006 = CARTESIAN_POINT ( 'NONE',  ( -58.22785051087649322, 0.5684335961332193099, 1.101539904997213215 ) ) ;
#13007 = LINE ( 'NONE', #7636, #19239 ) ;
#13008 = CARTESIAN_POINT ( 'NONE',  ( 8.216694157412756994, 117.5064756823292385, 0.07510791844681398433 ) ) ;
#13009 = CARTESIAN_POINT ( 'NONE',  ( -5.615711437771641279, 117.9270669303711117, 0.5242027053071315335 ) ) ;
#13010 = AXIS2_PLACEMENT_3D ( 'NONE', #20718, #13714, #4147 ) ;
#13011 = CARTESIAN_POINT ( 'NONE',  ( -4.262945350134766720, 117.9852873898591952, 0.8017283871570700660 ) ) ;
#13012 = DIRECTION ( 'NONE',  ( -0.01997839162482761832, -1.040247600000950455E-18, 0.9998004120163610509 ) ) ;
#13013 = CARTESIAN_POINT ( 'NONE',  ( -3.549018488562215801, 31.67372709507380790, 0.4994073303616778925 ) ) ;
#13014 = CARTESIAN_POINT ( 'NONE',  ( 12.91357091396819357, 121.2479969211051127, 1.612259173617573316 ) ) ;
#13015 = CARTESIAN_POINT ( 'NONE',  ( -3.199182136055901626, 19.34408232073488065, 3.339653329369344004 ) ) ;
#13016 = CARTESIAN_POINT ( 'NONE',  ( -4.443900581410109574, 30.07671411637534931, -7.177485988639727310 ) ) ;
#13017 = CARTESIAN_POINT ( 'NONE',  ( -2.173371897564630117, 116.7870940319093620, -0.5153656708244387374 ) ) ;
#13018 = CARTESIAN_POINT ( 'NONE',  ( -2.096106201831416271, 122.9394440205640961, -0.1965313455681949872 ) ) ;
#13019 = DIRECTION ( 'NONE',  ( 0.4849315768086481238, 0.8745520943968281280, -3.311806702191031061E-15 ) ) ;
#13020 = CIRCLE ( 'NONE', #30718, 5.080000000000006288 ) ;
#13021 = CARTESIAN_POINT ( 'NONE',  ( -7.842268484490568348, 73.30875693322846587, -1.269999999999996243 ) ) ;
#13022 = CARTESIAN_POINT ( 'NONE',  ( 3.055547683721570262, 104.6144662015413047, 4.375596321116328014 ) ) ;
#13023 = CIRCLE ( 'NONE', #36865, 0.5079999999999946780 ) ;
#13024 = CARTESIAN_POINT ( 'NONE',  ( -0.5093740622119584671, 14.76157059199007016, 4.595130897425484306 ) ) ;
#13025 = CARTESIAN_POINT ( 'NONE',  ( -46.98348089488076340, 24.79145570443882463, -2.118842393845993044 ) ) ;
#13026 = CARTESIAN_POINT ( 'NONE',  ( -0.7702531061077007024, 117.3993836066117353, -1.486315056237274890 ) ) ;
#13027 = CARTESIAN_POINT ( 'NONE',  ( 3.025122737553283869, -13.62787997529110662, 1.286645544439679156 ) ) ;
#13028 = EDGE_CURVE ( 'NONE', #33162, #41686, #7767, .T. ) ;
#13029 = ADVANCED_FACE ( 'NONE', ( #9027 ), #19082, .F. ) ;
#13030 = CARTESIAN_POINT ( 'NONE',  ( 1.859996092182608640, 121.3688471916803451, -0.2894809034927952052 ) ) ;
#13031 = CARTESIAN_POINT ( 'NONE',  ( -21.63859276624145878, 151.3813297165527274, 0.4067934712883242709 ) ) ;
#13032 = ORIENTED_EDGE ( 'NONE', *, *, #2569, .T. ) ;
#13033 = CARTESIAN_POINT ( 'NONE',  ( 5.241362157049057835, 65.30181249999998272, 5.310945289804168468 ) ) ;
#13034 = EDGE_LOOP ( 'NONE', ( #6667, #14960, #21486, #34133 ) ) ;
#13035 = CARTESIAN_POINT ( 'NONE',  ( -2.880736501481947265, 31.22451072257329585, 0.7774695130801791976 ) ) ;
#13036 = AXIS2_PLACEMENT_3D ( 'NONE', #1092, #16623, #7481 ) ;
#13037 = CARTESIAN_POINT ( 'NONE',  ( 6.120062074970366695, -14.59381343598747982, -0.2446369611249375742 ) ) ;
#13038 = CARTESIAN_POINT ( 'NONE',  ( -19.84954981513673644, 141.2215177107240436, 1.686013488323441223 ) ) ;
#13039 = CARTESIAN_POINT ( 'NONE',  ( 13.66011217756154394, 120.8017016962898396, -0.8211468655896803082 ) ) ;
#13040 = CARTESIAN_POINT ( 'NONE',  ( 0.05711764529616595448, 0.5181683540770932739, -4.631227783250111862 ) ) ;
#13041 = CARTESIAN_POINT ( 'NONE',  ( -58.64992616607198528, -0.3153078225257616718, -0.3300484825081549944 ) ) ;
#13042 = EDGE_LOOP ( 'NONE', ( #12620, #31800, #23355, #14667 ) ) ;
#13043 = CARTESIAN_POINT ( 'NONE',  ( -58.36915991843427776, -0.2902476589034808097, -0.03232548579177411258 ) ) ;
#13044 = CARTESIAN_POINT ( 'NONE',  ( -0.002462548249366884514, 123.7646714092002611, 0.1232359841710926190 ) ) ;
#13045 =( NAMED_UNIT ( * ) PLANE_ANGLE_UNIT ( ) SI_UNIT ( $, .RADIAN. ) );
#13046 = CARTESIAN_POINT ( 'NONE',  ( -17.54876304911002194, 147.2926247242496345, 1.462364720961516040 ) ) ;
#13047 = CARTESIAN_POINT ( 'NONE',  ( 12.22472920326790558, 122.9664497093790629, -1.310580005724927499 ) ) ;
#13048 = CARTESIAN_POINT ( 'NONE',  ( -20.74782508767443900, 148.9555414352193168, -2.393722347598511657 ) ) ;
#13049 = CARTESIAN_POINT ( 'NONE',  ( -58.30521585032268206, -0.1116666926106041347, -0.6575736669891941721 ) ) ;
#13050 = VERTEX_POINT ( 'NONE', #16080 ) ;
#13051 = CARTESIAN_POINT ( 'NONE',  ( 4.556576186746449153, 118.1065164564682703, -0.4936797517044704819 ) ) ;
#13052 = CARTESIAN_POINT ( 'NONE',  ( 15.06908741399238849, 148.9283877096812034, -0.6536164350837784243 ) ) ;
#13053 = ORIENTED_EDGE ( 'NONE', *, *, #39249, .T. ) ;
#13054 = CARTESIAN_POINT ( 'NONE',  ( -17.14693169618197999, 148.7218176724978775, -2.218585656167707754 ) ) ;
#13055 = CARTESIAN_POINT ( 'NONE',  ( 3.847030120444227208, -15.22745156820166912, 0.3463556848800000143 ) ) ;
#13056 = CARTESIAN_POINT ( 'NONE',  ( -5.043483815839604922, 105.1217967216603029, -1.770462747484127242 ) ) ;
#13057 = B_SPLINE_CURVE_WITH_KNOTS ( 'NONE', 3,
 ( #38683, #29510, #19691, #32285, #12481, #23089, #22875, #3542, #42097, #13316, #26302, #41888, #9289, #6305, #39311, #32070, #6101, #31860, #22250, #28661, #12892, #25676, #38887, #3114, #25475, #19484, #2700, #41673, #16074, #9489, #9699, #39100, #22454, #35276, #19064, #22665, #135, #32493, #29292, #14144, #40159, #24148, #3754, #23725, #23939, #39741, #33134, #27147, #10951, #37157, #10540, #33555, #36743, #20314, #13941, #3964, #20525, #29715, #16925, #14345, #557, #33341, #4387, #23509, #1389, #36337, #39950, #36956, #19908, #30135, #26520, #29925, #36536, #4171, #7777, #27355, #16712, #763, #11163, #7355, #32923, #17549, #26733, #17345, #17133, #13532, #974, #4590, #26939, #10744, #33765, #39526, #40368, #10330, #13739, #23300, #30550, #7153, #7565, #30334, #20112, #1181, #20740, #41199, #18595, #34594, #2014, #5216, #8182, #40987, #30965, #24781, #8604, #1601, #12003, #12219, #11790, #4800, #33972, #31604, #18170, #5638, #17751, #41412, #37779, #5006, #2442, #2229, #24995, #21566, #31173, #14767, #40780, #8394, #11371, #30751, #11577, #15403, #14558, #25209, #5423, #18378, #28407, #37362, #37995, #7979, #1806, #31387, #14977, #15190, #20947, #17965, #27978, #27565, #28193, #8819, #40574, #24358 ),
 .UNSPECIFIED., .F., .F.,
 ( 4, 2, 2, 2, 2, 2, 2, 2, 2, 1, 2, 2, 2, 2, 1, 2, 2, 2, 1, 1, 1, 2, 2, 2, 2, 2, 2, 2, 2, 2, 1, 2, 2, 2, 2, 1, 1, 1, 2, 2, 2, 2, 2, 1, 2, 2, 2, 1, 2, 2, 2, 2, 2, 1, 1, 1, 2, 1, 2, 2, 2, 2, 2, 1, 1, 1, 1, 2, 2, 2, 2, 2, 1, 1, 1, 1, 2, 2, 2, 2, 1, 1, 1, 1, 2, 2, 2, 1, 2, 2, 2, 2, 4 ),
 ( 0.000000000000000000, 0.0004882812499988943306, 0.0007324218749983417128, 0.0008544921874980726138, 0.0009765624999978036232, 0.001464843749996776233, 0.001708984374996262538, 0.001953124999995749060, 0.002929687499993625325, 0.003417968749992564542, 0.003662109374992034583, 0.003906249999991504192, 0.005859374999987647901, 0.006835937499985785676, 0.007324218749984854129, 0.007568359374984387489, 0.007812499999983922583, 0.01171874999997702359, 0.01367187499997357149, 0.01464843749997184717, 0.01513671874997098328, 0.01538085937497043684, 0.01562499999996988867, 0.02343749999994880831, 0.02734374999993813282, 0.02929687499993280028, 0.03027343749993023289, 0.03124999999992766897, 0.03906249999990741434, 0.04296874999989729049, 0.04492187499989241245, 0.04589843749988977567, 0.04687499999988713195, 0.05468749999986757121, 0.05859374999985778737, 0.06054687499985289545, 0.06152343749985028643, 0.06201171874984880150, 0.06225585937484824639, 0.06249999999984768434, 0.07031249999985582366, 0.07128906249985692001, 0.07226562499985801635, 0.07421874999986018129, 0.07812499999986419197, 0.08007812499986623200, 0.08105468749986723120, 0.08203124999986824428, 0.08593749999987203292, 0.09374999999987990162, 0.09765624999988384292, 0.09814453124988455068, 0.09863281249988525845, 0.09960937499988636867, 0.1015624999998882283, 0.1093749999998950700, 0.1171874999999019257, 0.1210937499999053396, 0.1230468749999070605, 0.1249999999999087674, 0.1874999999999688860, 0.2187499999999987232, 0.2343750000000136835, 0.2421875000000211220, 0.2460937500000248412, 0.2480468750000264788, 0.2490234375000273670, 0.2495117187500278944, 0.2500000000000284217, 0.3750000000000308087, 0.4375000000000319744, 0.4687500000000323630, 0.4843750000000326961, 0.4921875000000331402, 0.4960937500000334732, 0.4980468750000338618, 0.4990234375000341394, 0.5000000000000344169, 0.6250000000000179856, 0.6875000000000095479, 0.7187500000000052180, 0.7343750000000032196, 0.7421875000000021094, 0.7460937500000018874, 0.7480468750000017764, 0.7500000000000016653, 0.8750000000000047740, 0.9062500000000055511, 0.9218750000000058842, 0.9257812500000057732, 0.9296875000000055511, 0.9375000000000052180, 1.000000000000000000 ),
 .UNSPECIFIED. ) ;
#13058 = VECTOR ( 'NONE', #38611, 1000.000000000000114 ) ;
#13059 = EDGE_CURVE ( 'NONE', #11474, #25, #23360, .T. ) ;
#13060 = CARTESIAN_POINT ( 'NONE',  ( -49.14072577824711630, 13.89916973120783972, -8.531461402113531655E-15 ) ) ;
#13061 = CARTESIAN_POINT ( 'NONE',  ( -4.784146136289919582, 117.6343108313606933, 0.9514533180737122509 ) ) ;
#13062 = CARTESIAN_POINT ( 'NONE',  ( 8.120140396194329924, 121.3802920439979118, 1.244985559442681078 ) ) ;
#13063 = CARTESIAN_POINT ( 'NONE',  ( -47.19079517381230460, 25.11791606914811936, 2.000773461933185171 ) ) ;
#13064 = CARTESIAN_POINT ( 'NONE',  ( 3.655561289726139140, 27.93047918286777076, -2.829280713513928180 ) ) ;
#13065 = CARTESIAN_POINT ( 'NONE',  ( 5.931002064882541447, 121.5392726388429168, 0.1896088198168330019 ) ) ;
#13066 = CARTESIAN_POINT ( 'NONE',  ( -8.270297712355500153, 69.35377921309405735, -1.523999999999995802 ) ) ;
#13067 = CIRCLE ( 'NONE', #11703, 0.6350000000000001199 ) ;
#13068 = CARTESIAN_POINT ( 'NONE',  ( -50.02669608763527265, 12.78473261814652773, -0.3947048150275272449 ) ) ;
#13069 = CARTESIAN_POINT ( 'NONE',  ( 8.798071512540863282, 117.6842349196870572, 0.1758064070670784795 ) ) ;
#13070 = CARTESIAN_POINT ( 'NONE',  ( -5.078986093043186045, 87.97746620154572383, -0.1014902294541231709 ) ) ;
#13071 = LINE ( 'NONE', #19036, #37014 ) ;
#13072 = CARTESIAN_POINT ( 'NONE',  ( -48.73363302905276129, 18.22424113963231207, 5.158540213015197828 ) ) ;
#13073 = CARTESIAN_POINT ( 'NONE',  ( -8.557937876389182463, 118.7559978815208552, -1.194452831535397719 ) ) ;
#13074 = CARTESIAN_POINT ( 'NONE',  ( -5.241362157049148429, 88.73331249999998249, 5.310945289804168468 ) ) ;
#13075 = DIRECTION ( 'NONE',  ( -0.8745520943968235761, 0.4849315768086558953, -5.361993529360570985E-16 ) ) ;
#13076 = CARTESIAN_POINT ( 'NONE',  ( 0.000000000000000000, 0.000000000000000000, 0.000000000000000000 ) ) ;
#13077 = CARTESIAN_POINT ( 'NONE',  ( -56.91719228404756592, 5.442273006173628858, 0.3640331681397596664 ) ) ;
#13078 = EDGE_CURVE ( 'NONE', #18488, #22953, #39050, .T. ) ;
#13079 = CARTESIAN_POINT ( 'NONE',  ( -57.29531047346088712, 2.067549486662559222, 1.749273462387482603 ) ) ;
#13080 = CARTESIAN_POINT ( 'NONE',  ( -0.002426349801212479562, 116.5266044092193880, 0.1214244658147705380 ) ) ;
#13081 = ORIENTED_EDGE ( 'NONE', *, *, #11560, .F. ) ;
#13082 = CARTESIAN_POINT ( 'NONE',  ( -52.06588384954375925, 19.72955628912294301, -0.3571238398875267728 ) ) ;
#13083 = CARTESIAN_POINT ( 'NONE',  ( -6.055293159970121408, 121.4335270663578683, -0.1273889451180159893 ) ) ;
#13084 = ORIENTED_EDGE ( 'NONE', *, *, #17244, .F. ) ;
#13085 = DIRECTION ( 'NONE',  ( 1.000000000000000000, -9.627370216492862708E-17, 0.000000000000000000 ) ) ;
#13086 = CARTESIAN_POINT ( 'NONE',  ( -0.6369907463662666247, 120.9735524437166561, -0.07606544612864242494 ) ) ;
#13087 = CARTESIAN_POINT ( 'NONE',  ( 2.850627862023833892, -15.32561772411503220, 5.765353718581858189 ) ) ;
#13088 = CARTESIAN_POINT ( 'NONE',  ( -13.73828690980685963, 121.6032371815301900, 1.070726600328922640 ) ) ;
#13089 = CARTESIAN_POINT ( 'NONE',  ( -5.112263072780976358, 116.9830771656617827, -0.4445654250014547948 ) ) ;
#13090 = VECTOR ( 'NONE', #9575, 1000.000000000000000 ) ;
#13091 = CARTESIAN_POINT ( 'NONE',  ( 14.74522353080544157, 120.3062992333385921, 0.5208356519839252297 ) ) ;
#13092 = CARTESIAN_POINT ( 'NONE',  ( 9.045801974870443019, 124.1535288145754237, 0.2702127546846336825 ) ) ;
#13093 = CARTESIAN_POINT ( 'NONE',  ( 5.276949677772993397, 115.6909491485453145, -0.8076138971160246038 ) ) ;
#13094 = CARTESIAN_POINT ( 'NONE',  ( -0.5978751570792395498, 11.96162690172616294, -0.7744233872902203109 ) ) ;
#13095 = CARTESIAN_POINT ( 'NONE',  ( -15.60991558517076605, 120.8175431576145940, -0.4704071646738434143 ) ) ;
#13096 = DIRECTION ( 'NONE',  ( -0.9998004120163608288, -5.205824365704081956E-17, -0.01997839162482748995 ) ) ;
#13097 = EDGE_CURVE ( 'NONE', #17493, #24980, #1661, .T. ) ;
#13098 = DIRECTION ( 'NONE',  ( 0.4849315768086480127, 0.8745520943968279060, 1.030032898892941415E-16 ) ) ;
#13099 = ORIENTED_EDGE ( 'NONE', *, *, #7427, .F. ) ;
#13100 = CARTESIAN_POINT ( 'NONE',  ( 5.660275087203261002, 117.9280556746221293, 1.049642431879043158 ) ) ;
#13101 = ORIENTED_EDGE ( 'NONE', *, *, #7093, .F. ) ;
#13102 = DIRECTION ( 'NONE',  ( 1.000000000000000000, 0.000000000000000000, 0.000000000000000000 ) ) ;
#13103 = CARTESIAN_POINT ( 'NONE',  ( 12.26619010297299717, 120.4651188882986759, 1.462776157934944310 ) ) ;
#13104 = CARTESIAN_POINT ( 'NONE',  ( 1.243168248768940831, 118.5604221528582372, -0.6402677339867957063 ) ) ;
#13105 = CARTESIAN_POINT ( 'NONE',  ( 0.3859925973045487679, 4.674766832570296238, -0.8944012262243137279 ) ) ;
#13106 = CARTESIAN_POINT ( 'NONE',  ( -3.896388542364412455, 10.26897056970580380, 7.485861278012786002 ) ) ;
#13107 = CARTESIAN_POINT ( 'NONE',  ( -9.779442063456469825, 157.5983698538113629, -1.672576317993901274 ) ) ;
#13108 = CARTESIAN_POINT ( 'NONE',  ( 4.803717081333231498, 117.8803964050671311, -0.6822223753014300396 ) ) ;
#13109 = CARTESIAN_POINT ( 'NONE',  ( 7.326027964657929381, 123.0350022594044219, 0.2150643116641768604 ) ) ;
#13110 = AXIS2_PLACEMENT_3D ( 'NONE', #20965, #34607, #21792 ) ;
#13111 = CARTESIAN_POINT ( 'NONE',  ( 7.221579903133987344, 121.4526873951801633, -0.6561908252823551724 ) ) ;
#13112 = CARTESIAN_POINT ( 'NONE',  ( -5.308493528853332144, 121.3525139070573147, -0.1060763342189516428 ) ) ;
#13113 = EDGE_CURVE ( 'NONE', #13951, #12049, #39730, .T. ) ;
#13114 = ORIENTED_EDGE ( 'NONE', *, *, #39889, .T. ) ;
#13115 = CARTESIAN_POINT ( 'NONE',  ( -10.15136974315543839, 155.5514087735115822, -2.139549497352468244 ) ) ;
#13116 = CARTESIAN_POINT ( 'NONE',  ( 5.552702978602249040, -15.16724029374752547, 2.010675452401557095 ) ) ;
#13117 =( BOUNDED_SURFACE ( )  B_SPLINE_SURFACE ( 3, 2, ( 
 ( #20771, #17377, #7187 ),
 ( #20146, #23757, #29751 ),
 ( #30367, #33795, #7386 ),
 ( #17166, #11192, #36779 ),
 ( #7595, #10988, #20346 ),
 ( #13769, #1216, #10363 ) ),
 .UNSPECIFIED., .F., .F., .T. ) 
 B_SPLINE_SURFACE_WITH_KNOTS ( ( 4, 2, 4 ),
 ( 3, 3 ),
 ( 0.000000000000000000, 0.0007381999790946869831, 0.001476399958189373966 ),
 ( 0.000000000000000000, 1.000000000000000000 ),
 .UNSPECIFIED. ) 
 GEOMETRIC_REPRESENTATION_ITEM ( )  RATIONAL_B_SPLINE_SURFACE ( (
 ( 1.000000000000000000, 0.7071067811865393571, 1.000000000000000000),
 ( 1.000000000000000000, 0.7071031648639772849, 1.000000000000000000),
 ( 1.000000000000000000, 0.7049885726714537615, 1.000000000000000000),
 ( 1.000000000000000000, 0.6987948356736179978, 1.000000000000000000),
 ( 1.000000000000000000, 0.6949210395568362619, 1.000000000000000000),
 ( 1.000000000000000000, 0.6916534930271285297, 1.000000000000000000) ) ) 
 REPRESENTATION_ITEM ( '' )  SURFACE ( )  );
#13118 = CARTESIAN_POINT ( 'NONE',  ( -11.58677707360137532, 12.96416000000000146, -4.474811398758259173 ) ) ;
#13119 = CARTESIAN_POINT ( 'NONE',  ( -45.39816439898302036, 21.06106408185672763, -4.080402960186392036 ) ) ;
#13120 = ORIENTED_EDGE ( 'NONE', *, *, #30501, .F. ) ;
#13121 = CARTESIAN_POINT ( 'NONE',  ( 0.4972808831007263231, 119.3183582894065893, 0.5800711753708563956 ) ) ;
#13122 = CARTESIAN_POINT ( 'NONE',  ( -15.26262975083406381, 148.0175730703489592, -0.3049836654617371079 ) ) ;
#13123 = EDGE_CURVE ( 'NONE', #34625, #37003, #25337, .T. ) ;
#13124 = DIRECTION ( 'NONE',  ( -0.8745520943968250194, 0.4849315768086532863, -5.361993529360574930E-16 ) ) ;
#13125 = AXIS2_PLACEMENT_3D ( 'NONE', #29441, #10476, #26237 ) ;
#13126 = CARTESIAN_POINT ( 'NONE',  ( -4.551932963793476006, 124.4408722044843927, -0.07212455616362435651 ) ) ;
#13127 = EDGE_CURVE ( 'NONE', #8502, #32851, #3702, .T. ) ;
#13128 = CARTESIAN_POINT ( 'NONE',  ( -6.340062920055459017, 30.52953040661039807, -5.581008500864042432 ) ) ;
#13129 = CARTESIAN_POINT ( 'NONE',  ( 9.927929498514727058, 124.8826105625126530, 0.6426615136408517781 ) ) ;
#13130 = CARTESIAN_POINT ( 'NONE',  ( 4.841477346015976124, 117.1414559920645644, -0.3963857013944135366 ) ) ;
#13131 = CARTESIAN_POINT ( 'NONE',  ( -13.85159022459153988, 71.11999999999999034, -5.016499999999999737 ) ) ;
#13132 = CYLINDRICAL_SURFACE ( 'NONE', #39931, 0.6349999999999984546 ) ;
#13133 = CONICAL_SURFACE ( 'NONE', #38322, 16.60960244842765476, 0.7853981633974488341 ) ;
#13134 = CARTESIAN_POINT ( 'NONE',  ( -21.90617686096483396, 151.4314113202728436, -0.4124301881307765316 ) ) ;
#13135 = ADVANCED_FACE ( 'NONE', ( #28882 ), #35490, .T. ) ;
#13136 = VERTEX_POINT ( 'NONE', #22672 ) ;
#13137 = CARTESIAN_POINT ( 'NONE',  ( 6.859376321155130185, 121.4516053872399226, -0.5286681357537772463 ) ) ;
#13138 = CARTESIAN_POINT ( 'NONE',  ( -10.32579803928178386, 77.06797118195436269, 1.270000000000000906 ) ) ;
#13139 = CARTESIAN_POINT ( 'NONE',  ( -13.22128265123331481, 134.0707761029912035, -0.8398552229569320460 ) ) ;
#13140 = CARTESIAN_POINT ( 'NONE',  ( 2.474817137005230983, -14.89163965485640340, 5.628581999208025266 ) ) ;
#13141 = DIRECTION ( 'NONE',  ( 0.9454731675810330582, -0.3256999990547864710, 5.459396135145336213E-16 ) ) ;
#13142 = CARTESIAN_POINT ( 'NONE',  ( 23.42514220146282966, 142.8382549601284097, 0.4680900899253090941 ) ) ;
#13143 = ORIENTED_EDGE ( 'NONE', *, *, #22178, .F. ) ;
#13144 = CARTESIAN_POINT ( 'NONE',  ( 4.087030650986479330, 6.990161447142720696, 2.163025551504125232 ) ) ;
#13145 = CARTESIAN_POINT ( 'NONE',  ( -0.2924095564369283418, 116.4254662015451913, -0.005843038833676759622 ) ) ;
#13146 = CARTESIAN_POINT ( 'NONE',  ( -13.43845804798116106, 156.9141898299356512, -0.2685323735513600041 ) ) ;
#13147 = CARTESIAN_POINT ( 'NONE',  ( 10.92199999999999704, 16.51000000000000156, 0.000000000000000000 ) ) ;
#13148 = CARTESIAN_POINT ( 'NONE',  ( -6.019795697468436124, 120.5055318871546461, 0.7549818993857987381 ) ) ;
#13149 = CARTESIAN_POINT ( 'NONE',  ( 4.577905313181523717, 13.52175256873284326, -0.6256056815880789435 ) ) ;
#13150 = CARTESIAN_POINT ( 'NONE',  ( 21.93197806114481807, 150.5960492154097778, 1.608405794939391731 ) ) ;
#13151 = CARTESIAN_POINT ( 'NONE',  ( -7.994219716368544226, 68.36415334912796027, 1.270000000000003570 ) ) ;
#13153 = CARTESIAN_POINT ( 'NONE',  ( 21.18042260023730705, 148.1333099715771766, -1.515480231459294114 ) ) ;
#13152 = CARTESIAN_POINT ( 'NONE',  ( 4.737240446979624764, 56.51500000000001478, 4.914899999999992275 ) ) ;
#13154 = AXIS2_PLACEMENT_3D ( 'NONE', #21441, #21238, #2098 ) ;
#13155 = CARTESIAN_POINT ( 'NONE',  ( -1.792273654952471595, 16.32048121479114045, -4.264856162967389785 ) ) ;
#13156 = CARTESIAN_POINT ( 'NONE',  ( -3.132853369507721197, 159.3671203531505114, -0.7742396785067983123 ) ) ;
#13157 = EDGE_LOOP ( 'NONE', ( #35853, #40144 ) ) ;
#13158 = VECTOR ( 'NONE', #10594, 1000.000000000000000 ) ;
#13159 = ADVANCED_FACE ( 'NONE', ( #36963 ), #26792, .F. ) ;
#13160 = B_SPLINE_CURVE_WITH_KNOTS ( 'NONE', 3,
 ( #15571, #32766, #41372, #12392 ),
 .UNSPECIFIED., .F., .F.,
 ( 4, 4 ),
 ( 0.001531465774898539082, 0.001759348651853699479 ),
 .UNSPECIFIED. ) ;
#13161 = CARTESIAN_POINT ( 'NONE',  ( -10.49519746661490593, 153.0637448873655728, 0.1985316654307170414 ) ) ;
#13162 = CARTESIAN_POINT ( 'NONE',  ( 5.767107246999573889, -13.94705323133380048, 2.761945726399152701 ) ) ;
#13163 = DIRECTION ( 'NONE',  ( 4.017660918040594346E-17, -1.000000000000000000, -2.376309959284834438E-19 ) ) ;
#13164 = AXIS2_PLACEMENT_3D ( 'NONE', #32664, #35660, #38436 ) ;
#13165 = CARTESIAN_POINT ( 'NONE',  ( -1.982805074603235296, 106.5591908312118221, -4.949216245379176371 ) ) ;
#13166 = ORIENTED_EDGE ( 'NONE', *, *, #7121, .T. ) ;
#13167 = CARTESIAN_POINT ( 'NONE',  ( 12.48017577322008442, 122.5542284311838870, 1.820249166172293265 ) ) ;
#13168 = CARTESIAN_POINT ( 'NONE',  ( 9.094996104468812348, 78.64197151092923832, 1.904999999999988258 ) ) ;
#13169 = DIRECTION ( 'NONE',  ( 0.3256999990547876367, 0.9454731675810326141, 8.328397965208553695E-18 ) ) ;
#13170 = CARTESIAN_POINT ( 'NONE',  ( -22.81445126409639812, 149.1304179266472261, 0.6239350898115072486 ) ) ;
#13171 = EDGE_CURVE ( 'NONE', #9260, #3899, #19556, .T. ) ;
#13172 = EDGE_CURVE ( 'NONE', #31070, #9063, #31560, .T. ) ;
#13173 = CARTESIAN_POINT ( 'NONE',  ( 15.22618061423887426, 120.7148350616293300, -0.1140551857323334473 ) ) ;
#13174 = FACE_OUTER_BOUND ( 'NONE', #6098, .T. ) ;
#13175 = CIRCLE ( 'NONE', #18611, 3.175000000000001155 ) ;
#13176 = CARTESIAN_POINT ( 'NONE',  ( -46.69404853191296212, 26.00096993889310681, 1.337746353888202622 ) ) ;
#13177 = CARTESIAN_POINT ( 'NONE',  ( -47.62967605938791849, 25.45029596856965171, -8.552750547210872508E-15 ) ) ;
#13178 = PLANE ( 'NONE',  #12137 ) ;
#13179 = CARTESIAN_POINT ( 'NONE',  ( -53.45432727069204759, 10.77832982246877691, 4.078803160923774485 ) ) ;
#13180 = CARTESIAN_POINT ( 'NONE',  ( 14.39766717389552220, 57.78500000000000369, 1.904999999999991367 ) ) ;
#13181 = CARTESIAN_POINT ( 'NONE',  ( -4.601497063313658487, 118.0406231673457853, 0.6544036431963192735 ) ) ;
#13182 = CARTESIAN_POINT ( 'NONE',  ( -58.37241122568488549, -0.2962816677227891882, -1.025775813386803588E-14 ) ) ;
#13183 = AXIS2_PLACEMENT_3D ( 'NONE', #5662, #38018, #34829 ) ;
#13184 = ORIENTED_EDGE ( 'NONE', *, *, #5549, .T. ) ;
#13185 = CARTESIAN_POINT ( 'NONE',  ( -0.1700182685997659593, 118.7629491485454025, -1.279869737540616059 ) ) ;
#13186 = CARTESIAN_POINT ( 'NONE',  ( 5.909374519815934867, 119.0059304655898131, -1.022020752696235935 ) ) ;
#13187 = CARTESIAN_POINT ( 'NONE',  ( -2.481140172163744495, 107.2306503360107541, -4.727365043318366489 ) ) ;
#13188 = CARTESIAN_POINT ( 'NONE',  ( 4.584301209864922733, 117.9735000374216440, 0.9263109292462509137 ) ) ;
#13189 = CARTESIAN_POINT ( 'NONE',  ( -46.79514595010191158, 25.77136020477034606, -0.9526608576032509212 ) ) ;
#13190 = CARTESIAN_POINT ( 'NONE',  ( -9.867978122178644895, 123.6875948057429895, -1.092113756099770017 ) ) ;
#13191 = AXIS2_PLACEMENT_3D ( 'NONE', #12721, #39351, #39567 ) ;
#13192 = CARTESIAN_POINT ( 'NONE',  ( -1.824499746566420999, 115.7028212133603802, -1.722090710131633173 ) ) ;
#13193 = CARTESIAN_POINT ( 'NONE',  ( -1.119363313351095846, 106.1653619527225629, 5.174161313809158891 ) ) ;
#13194 = CARTESIAN_POINT ( 'NONE',  ( 14.79536922792820697, 61.64024183321802042, -1.904999999999999583 ) ) ;
#13195 = CARTESIAN_POINT ( 'NONE',  ( 7.669269000495035904, 124.9344662015457317, 0.1532502464757267702 ) ) ;
#13196 = CARTESIAN_POINT ( 'NONE',  ( -17.14717842969347572, 147.4900653055648547, -2.050122926623737296 ) ) ;
#13197 = CARTESIAN_POINT ( 'NONE',  ( 15.97340373827820947, 121.0409387471171101, 0.3191866212789526425 ) ) ;
#13198 = CARTESIAN_POINT ( 'NONE',  ( -0.02615207601228260181, 159.0391464308674756, 1.308756824028193488 ) ) ;
#13199 = CYLINDRICAL_SURFACE ( 'NONE', #2502, 5.588000000000006295 ) ;
#13200 = CARTESIAN_POINT ( 'NONE',  ( -1.631653520256556744, 120.9961520629786094, 0.03448668289050316194 ) ) ;
#13201 = CARTESIAN_POINT ( 'NONE',  ( 0.6989348986720191892, -4.029744825116962303, 4.573446973323917142 ) ) ;
#13203 = EDGE_LOOP ( 'NONE', ( #27815, #18339, #10998, #3684, #7731 ) ) ;
#13202 = CARTESIAN_POINT ( 'NONE',  ( 8.152918552588246826, 117.7057695168643932, 0.6423243676978417360 ) ) ;
#13204 = DIRECTION ( 'NONE',  ( -5.188838149069471174E-16, 1.699382548006136313E-16, 1.000000000000000000 ) ) ;
#13205 = AXIS2_PLACEMENT_3D ( 'NONE', #33252, #14056, #27061 ) ;
#13206 = CARTESIAN_POINT ( 'NONE',  ( 3.434117431421463973, -14.91634622600368587, 0.6670077989445850619 ) ) ;
#13207 = AXIS2_PLACEMENT_3D ( 'NONE', #29622, #457, #19181 ) ;
#13208 = CARTESIAN_POINT ( 'NONE',  ( -16.12483552447403312, 131.4332636412663931, 1.626400019052950618 ) ) ;
#13209 = CARTESIAN_POINT ( 'NONE',  ( 0.9735350199255810022, 12.44701472381428609, 0.02964292050307446719 ) ) ;
#13210 = CARTESIAN_POINT ( 'NONE',  ( -22.61937536341561383, 150.3405807453409579, -1.175526429919688365 ) ) ;
#13211 = CARTESIAN_POINT ( 'NONE',  ( 0.9102147817015755482, -10.07290960004636737, -0.3509275504499672627 ) ) ;
#13212 = EDGE_LOOP ( 'NONE', ( #35863, #37765, #21282, #22552 ) ) ;
#13213 = ORIENTED_EDGE ( 'NONE', *, *, #6882, .F. ) ;
#13214 = CARTESIAN_POINT ( 'NONE',  ( -42.93826774478920072, 21.39662913260299959, 1.244340269653798181 ) ) ;
#13215 = CARTESIAN_POINT ( 'NONE',  ( 5.192700560040893976, 116.2637919873444190, 1.171650394069924994 ) ) ;
#13216 = CARTESIAN_POINT ( 'NONE',  ( 0.000000000000000000, 0.000000000000000000, 0.000000000000000000 ) ) ;
#13217 = CARTESIAN_POINT ( 'NONE',  ( -14.80764902091328317, 139.2804412874323248, 0.6846718672572660314 ) ) ;
#13218 = CARTESIAN_POINT ( 'NONE',  ( 3.936650548058306054, -12.34391569202568384, 1.586490187297609156 ) ) ;
#13219 = CARTESIAN_POINT ( 'NONE',  ( 10.96277846527056532, 123.4376579628654014, -1.079141073574104270 ) ) ;
#13220 = CIRCLE ( 'NONE', #4401, 8.794749999999995183 ) ;
#13221 = CARTESIAN_POINT ( 'NONE',  ( -6.391991208685121606, 157.5392376370035095, -1.942695856706931457 ) ) ;
#13222 = LINE ( 'NONE', #35381, #18813 ) ;
#13223 = CARTESIAN_POINT ( 'NONE',  ( 2.576299636888586875, -14.89815494326314571, 4.769281578164155100 ) ) ;
#13224 = CARTESIAN_POINT ( 'NONE',  ( -4.217721592883738602, 33.55733840984517968, 3.057578620386037116 ) ) ;
#13225 = CARTESIAN_POINT ( 'NONE',  ( 15.79579396213690679, 146.5797798787131399, 0.08547097745249054856 ) ) ;
#13226 = ORIENTED_EDGE ( 'NONE', *, *, #16245, .F. ) ;
#13227 = CARTESIAN_POINT ( 'NONE',  ( -6.059261036834476144, 57.14999999999999858, -5.016499999999999737 ) ) ;
#13228 = DIRECTION ( 'NONE',  ( 1.000000000000000000, 0.000000000000000000, 0.000000000000000000 ) ) ;
#13229 = CARTESIAN_POINT ( 'NONE',  ( 14.60500000000000043, 71.11999999999999034, 5.016499999999999737 ) ) ;
#13230 = CARTESIAN_POINT ( 'NONE',  ( -58.80981292533127203, -0.2807566353364293610, 0.1195710083426413800 ) ) ;
#13231 = CARTESIAN_POINT ( 'NONE',  ( 16.10770497005612611, 121.2391669109744186, 0.2160841345999988949 ) ) ;
#13232 = CARTESIAN_POINT ( 'NONE',  ( -4.074523107743509343, 109.7948460773305897, 3.525254900318187889 ) ) ;
#13233 = CARTESIAN_POINT ( 'NONE',  ( -0.2373459926208821014, 115.6909491485452435, 1.758351689424455966 ) ) ;
#13234 = CARTESIAN_POINT ( 'NONE',  ( 5.078986093043054595, 72.99146620154573384, 0.1014902294541243921 ) ) ;
#13235 = CARTESIAN_POINT ( 'NONE',  ( -4.449580246473387568, 31.68166237237402783, -0.1589607140948728348 ) ) ;
#13236 = CARTESIAN_POINT ( 'NONE',  ( 17.27141581160015349, 128.5728276651957742, 2.069917288257624666 ) ) ;
#13237 = CARTESIAN_POINT ( 'NONE',  ( -3.633452533992191036, 26.69063122243967712, -2.854640957048627747 ) ) ;
#13238 = CARTESIAN_POINT ( 'NONE',  ( 8.390987441844862005, -15.30508105673078667, -0.4368898320763015541 ) ) ;
#13239 = CARTESIAN_POINT ( 'NONE',  ( 5.512484162645947983, 117.2038984734866744, -0.5832805902496341899 ) ) ;
#13240 = CARTESIAN_POINT ( 'NONE',  ( -3.315491766441375443, 124.7872298565087021, -0.07248898146901441852 ) ) ;
#13241 = CARTESIAN_POINT ( 'NONE',  ( -28.42835727709238114, 77.69497285144578314, 1.269999999999991358 ) ) ;
#13242 = CARTESIAN_POINT ( 'NONE',  ( 4.660168586682497782, 113.7931333194828909, -2.025023631320468365 ) ) ;
#13243 = CARTESIAN_POINT ( 'NONE',  ( -2.605357904536034663, 104.6144662015456959, 4.072382053397732626 ) ) ;
#13244 = CARTESIAN_POINT ( 'NONE',  ( 4.585487687326599726, 17.13547844546973309, 0.5842699607688729424 ) ) ;
#13245 = CARTESIAN_POINT ( 'NONE',  ( -7.772068811996249771, 69.25462295839062676, -1.269999999999995577 ) ) ;
#13246 = CARTESIAN_POINT ( 'NONE',  ( -24.16603736854983708, 76.82831944025377879, -1.524000000000005350 ) ) ;
#13247 = CARTESIAN_POINT ( 'NONE',  ( 3.115274840615241292, -13.78277351762104175, 1.693892316854531455 ) ) ;
#13248 = CARTESIAN_POINT ( 'NONE',  ( 0.7241986523582714108, 107.9696733310005214, -4.463276061801070504 ) ) ;
#13249 = CARTESIAN_POINT ( 'NONE',  ( -13.30049347609366528, 119.7426348059052685, 0.3046699512218789541 ) ) ;
#13250 = ORIENTED_EDGE ( 'NONE', *, *, #5832, .T. ) ;
#13251 = LINE ( 'NONE', #6445, #28984 ) ;
#13252 = ORIENTED_EDGE ( 'NONE', *, *, #22183, .F. ) ;
#13253 = CARTESIAN_POINT ( 'NONE',  ( -18.58115504727956591, 80.30342350548193053, 1.269999999999996243 ) ) ;
#13254 = CARTESIAN_POINT ( 'NONE',  ( 3.081975983035755373, -15.74694164559999088, 5.217090789712465870 ) ) ;
#13255 = CARTESIAN_POINT ( 'NONE',  ( -15.12798499870471325, 125.5446871707752763, 1.421763802809897115 ) ) ;
#13256 = CARTESIAN_POINT ( 'NONE',  ( 15.47853073355907050, 123.0316835747794642, -0.9738675477772636979 ) ) ;
#13257 = CARTESIAN_POINT ( 'NONE',  ( 4.523211737919912601, 7.414965188139293950, 0.9565071382433593117 ) ) ;
#13258 = CARTESIAN_POINT ( 'NONE',  ( -58.64011137842675225, -0.3059599299333538580, -0.3495911961056130113 ) ) ;
#13259 = ORIENTED_EDGE ( 'NONE', *, *, #28787, .F. ) ;
#13260 = CARTESIAN_POINT ( 'NONE',  ( -17.14500000000466784, 71.11999999999886768, -1.270000000000000684 ) ) ;
#13261 = CARTESIAN_POINT ( 'NONE',  ( 2.216013192100191542, 123.7320667226965867, 0.1296889073052086561 ) ) ;
#13262 = DIRECTION ( 'NONE',  ( 9.627370216492862708E-17, 1.000000000000000000, -0.000000000000000000 ) ) ;
#13263 = CARTESIAN_POINT ( 'NONE',  ( -15.84185526851211634, 139.7295799824062499, 1.277977597745375782 ) ) ;
#13264 = CARTESIAN_POINT ( 'NONE',  ( -5.684927786827005392, 65.51297084251929448, -1.269999999999993801 ) ) ;
#13265 = CARTESIAN_POINT ( 'NONE',  ( 14.54156464587782871, 128.5519869857110393, -1.481139062272948115 ) ) ;
#13266 = CARTESIAN_POINT ( 'NONE',  ( -20.33492986670573188, 149.7738053052645171, -2.379138827545465684 ) ) ;
#13267 = CARTESIAN_POINT ( 'NONE',  ( -57.52317756609133426, 3.014644041894651405, -1.981665235817958948 ) ) ;
#13268 = ORIENTED_EDGE ( 'NONE', *, *, #32116, .F. ) ;
#13269 = CARTESIAN_POINT ( 'NONE',  ( 4.514839441275080745, 118.1273531810763018, -0.5014787992856909460 ) ) ;
#13270 = CARTESIAN_POINT ( 'NONE',  ( 6.293976855803866677, 155.3815620563194955, -0.6499927463934686012 ) ) ;
#13271 = ORIENTED_EDGE ( 'NONE', *, *, #35252, .T. ) ;
#13272 = CARTESIAN_POINT ( 'NONE',  ( -10.97746297113260994, 123.2082810311540300, -1.564610664257708894 ) ) ;
#13273 = CARTESIAN_POINT ( 'NONE',  ( 2.997986829609769366, -15.20712831582179980, 4.056362312997196184 ) ) ;
#13274 = CARTESIAN_POINT ( 'NONE',  ( 11.58677707360137532, 17.14499999999999957, -4.474811398758258285 ) ) ;
#13275 = DIRECTION ( 'NONE',  ( 0.000000000000000000, 1.000000000000000000, 0.000000000000000000 ) ) ;
#13276 = AXIS2_PLACEMENT_3D ( 'NONE', #1373, #28338, #15546 ) ;
#13277 = CARTESIAN_POINT ( 'NONE',  ( -3.128764270554720728, 7.249652477310866594, -3.416742352092642321 ) ) ;
#13278 = CARTESIAN_POINT ( 'NONE',  ( -0.02768739821015471850, 156.9833357668885014, 1.385590625008458865 ) ) ;
#13279 = CARTESIAN_POINT ( 'NONE',  ( 3.005048127465709928, 39.20946620154573026, -0.9984965929130177331 ) ) ;
#13280 = CARTESIAN_POINT ( 'NONE',  ( 8.141433899912401628, -11.15112405914982219, -2.164028758433363286 ) ) ;
#13281 = CARTESIAN_POINT ( 'NONE',  ( 9.611064403080796126, 124.8310256250372277, 0.2802631513932195562 ) ) ;
#13282 = CARTESIAN_POINT ( 'NONE',  ( -6.318938770521977055, 64.36956080246774548, 1.524000000000005350 ) ) ;
#13283 = CARTESIAN_POINT ( 'NONE',  ( -46.67338572489354931, 16.85372243840488338, -7.793947694802422673E-15 ) ) ;
#13284 = CARTESIAN_POINT ( 'NONE',  ( 8.798540905981443672, 117.6856532891334979, 0.1377605412487556136 ) ) ;
#13285 = DIRECTION ( 'NONE',  ( -0.01997839162482761832, -1.040247600000951803E-18, 0.9998004120163610509 ) ) ;
#13286 = CARTESIAN_POINT ( 'NONE',  ( -46.66121569171162520, 26.06868089111461373, -1.308362493757629030 ) ) ;
#13287 = CARTESIAN_POINT ( 'NONE',  ( -28.74159376897886276, 60.61225341505600284, 1.269999999999992912 ) ) ;
#13288 = CARTESIAN_POINT ( 'NONE',  ( -29.91360363449003401, 70.04874496952835727, -1.524000000000007127 ) ) ;
#13289 = CARTESIAN_POINT ( 'NONE',  ( -5.965356522962950159, 77.01756250000002524, 5.016499999999999737 ) ) ;
#13290 = CARTESIAN_POINT ( 'NONE',  ( -4.074955089416341991, 118.2429491485453354, 0.1454234154749719787 ) ) ;
#13291 = FACE_OUTER_BOUND ( 'NONE', #26408, .T. ) ;
#13292 = CARTESIAN_POINT ( 'NONE',  ( -56.01560174880540188, 6.374421267034191985, 2.942705720416951110 ) ) ;
#13293 = CARTESIAN_POINT ( 'NONE',  ( -57.53497731650991653, 2.247686704661286505, 1.882970859819747433 ) ) ;
#13294 = CARTESIAN_POINT ( 'NONE',  ( -0.002459401150367294953, 159.6023738651833810, 0.1230784904792620454 ) ) ;
#13295 = ORIENTED_EDGE ( 'NONE', *, *, #18274, .T. ) ;
#13296 = CARTESIAN_POINT ( 'NONE',  ( -51.58376292578905975, 16.21309621351152330, -3.606096628736487730 ) ) ;
#13297 = CARTESIAN_POINT ( 'NONE',  ( 6.070073713991016362, 121.4399315956317054, 0.1168545408771763938 ) ) ;
#13298 = ORIENTED_EDGE ( 'NONE', *, *, #38651, .F. ) ;
#13299 = DIRECTION ( 'NONE',  ( 1.011795553208986377E-16, 1.000000000000000000, -0.000000000000000000 ) ) ;
#13300 = CARTESIAN_POINT ( 'NONE',  ( -8.793090887881007234, 123.6850765633735421, -0.2090564433599596816 ) ) ;
#13301 = CARTESIAN_POINT ( 'NONE',  ( 5.314795342858649185, -13.92002763284938638, 3.476347616104731753 ) ) ;
#13302 = CARTESIAN_POINT ( 'NONE',  ( -13.59286959522826876, 121.6867650304669013, 1.114243377227002618 ) ) ;
#13303 = CARTESIAN_POINT ( 'NONE',  ( 2.488009491785908800, 18.85968022696138391, -3.895047602898422223 ) ) ;
#13304 = CARTESIAN_POINT ( 'NONE',  ( 22.75358200450888191, 150.3871190066015799, 0.9055542368224058780 ) ) ;
#13305 = CARTESIAN_POINT ( 'NONE',  ( 7.761062069545141995, 154.6910982259716150, 0.3223645707746605193 ) ) ;
#13306 = DIRECTION ( 'NONE',  ( -0.6294287539884133587, -0.7770581983690755257, 0.000000000000000000 ) ) ;
#13307 = CARTESIAN_POINT ( 'NONE',  ( -0.6011478996571989475, -4.452122406214784611, 0.7678286701737500053 ) ) ;
#13308 = CARTESIAN_POINT ( 'NONE',  ( -20.41771265994164608, 129.0384130229076334, -0.5332683426449598141 ) ) ;
#13309 = CARTESIAN_POINT ( 'NONE',  ( -4.883848590450072358, 117.7607009110569862, 0.7127853619805604168 ) ) ;
#13310 = DIRECTION ( 'NONE',  ( 0.000000000000000000, 0.000000000000000000, 1.000000000000000000 ) ) ;
#13311 = ORIENTED_EDGE ( 'NONE', *, *, #25846, .F. ) ;
#13312 = CIRCLE ( 'NONE', #13998, 0.5080000000000002292 ) ;
#13313 = CARTESIAN_POINT ( 'NONE',  ( -5.551318956506019475, 117.0040208047680608, 0.4076684244378269151 ) ) ;
#13314 = ORIENTED_EDGE ( 'NONE', *, *, #19110, .F. ) ;
#13315 = CARTESIAN_POINT ( 'NONE',  ( -14.06576283519511428, 128.5416456306063253, 1.400350009575090038 ) ) ;
#13316 = CARTESIAN_POINT ( 'NONE',  ( -58.36932441242797864, -0.2905635077575413061, -0.02691069531237075610 ) ) ;
#13317 = CARTESIAN_POINT ( 'NONE',  ( 4.008523173341837165, 118.0179939250997023, 0.8984863180294773155 ) ) ;
#13318 = CARTESIAN_POINT ( 'NONE',  ( 4.147108463826105762, 118.7489093234570561, -0.8374340306925341926 ) ) ;
#13319 = CARTESIAN_POINT ( 'NONE',  ( -0.4197673533123916778, 5.974963139197415174, -0.8815698914671175057 ) ) ;
#13320 = CARTESIAN_POINT ( 'NONE',  ( -3.949038439882312179, 117.6225627337916393, -0.7921763187007299090 ) ) ;
#13321 = CARTESIAN_POINT ( 'NONE',  ( 4.730749274543958549, 117.9657169516164856, -0.6167170664779215716 ) ) ;
#13322 = CARTESIAN_POINT ( 'NONE',  ( -6.442348895218290093E-14, 63.84746620154572838, 4.408874939877717575E-29 ) ) ;
#13323 = CARTESIAN_POINT ( 'NONE',  ( 17.01014995307818722, 147.0740084267719396, -1.247012517048586622 ) ) ;
#13324 = CARTESIAN_POINT ( 'NONE',  ( -0.6421132086019301077, 120.9975462804897433, 0.01250379197263697117 ) ) ;
#13325 = VERTEX_POINT ( 'NONE', #7159 ) ;
#13326 = CARTESIAN_POINT ( 'NONE',  ( -18.62504088965198434, 146.9271955717142930, -2.448500584228243682 ) ) ;
#13327 = CARTESIAN_POINT ( 'NONE',  ( 3.756887254765235440, -15.74060793811991843, 4.623245420838687281 ) ) ;
#13328 = CARTESIAN_POINT ( 'NONE',  ( -5.339075059129462453, 115.7029491485453718, 0.2008031272278917312 ) ) ;
#13329 = EDGE_CURVE ( 'NONE', #33817, #26454, #7103, .T. ) ;
#13330 = CARTESIAN_POINT ( 'NONE',  ( -45.68084146533627177, 21.25878370237693815, -4.188014402015116211 ) ) ;
#13331 = ORIENTED_EDGE ( 'NONE', *, *, #8940, .F. ) ;
#13332 = CARTESIAN_POINT ( 'NONE',  ( 11.35704730865796463, 122.8492764348241337, 1.683887364911069273 ) ) ;
#13333 = CARTESIAN_POINT ( 'NONE',  ( -3.999880774356848523, 33.21692059697370070, 1.336717509662867398 ) ) ;
#13334 = DIRECTION ( 'NONE',  ( 1.000000000000000000, 6.353134868986659519E-16, -0.000000000000000000 ) ) ;
#13335 = CARTESIAN_POINT ( 'NONE',  ( -1.795323270064466792, 111.6436615656963909, 3.008962535700986596 ) ) ;
#13336 = CARTESIAN_POINT ( 'NONE',  ( -6.161128625374170831, 23.17997237347384853, 5.746845633999829950 ) ) ;
#13337 = CARTESIAN_POINT ( 'NONE',  ( 5.891535241408099033, 121.4229528491920576, 0.4202535615248634837 ) ) ;
#13338 = ADVANCED_FACE ( 'NONE', ( #27152 ), #28288, .T. ) ;
#13339 = VECTOR ( 'NONE', #18405, 1000.000000000000000 ) ;
#13340 = CARTESIAN_POINT ( 'NONE',  ( 5.853624122459038404, 117.3024554866451865, -0.4121555180536239926 ) ) ;
#13341 = CARTESIAN_POINT ( 'NONE',  ( 4.850929972935443146, 117.7610086971114356, 0.9074237114610381738 ) ) ;
#13342 = CARTESIAN_POINT ( 'NONE',  ( -13.46199999999999442, 17.14499999999999957, 0.000000000000000000 ) ) ;
#13343 = CARTESIAN_POINT ( 'NONE',  ( -5.781358041568783968, 116.9360814311326777, -0.07286664083783161994 ) ) ;
#13344 = EDGE_LOOP ( 'NONE', ( #36221, #32085, #38946, #27849 ) ) ;
#13345 = CARTESIAN_POINT ( 'NONE',  ( 5.100432878203172926, 120.2001702409422990, -0.6603920651319280521 ) ) ;
#13346 = CARTESIAN_POINT ( 'NONE',  ( 6.167707869044355640, -13.99985869331082178, 1.617558169626257314 ) ) ;
#13347 = CARTESIAN_POINT ( 'NONE',  ( -15.76219760562764094, 147.2673792861271522, -0.9072345144146883866 ) ) ;
#13348 = CARTESIAN_POINT ( 'NONE',  ( 4.249299001760414640, -12.92553893317818847, 2.698699680779739207 ) ) ;
#13349 = CARTESIAN_POINT ( 'NONE',  ( -14.96856157597592940, 121.5307057168427605, 0.7335553340177137782 ) ) ;
#13350 = CARTESIAN_POINT ( 'NONE',  ( -5.152689475313444234, 116.8412042432202185, -0.1029630068797482562 ) ) ;
#13351 = CARTESIAN_POINT ( 'NONE',  ( 23.21042342040053086, 149.6290410902582551, 0.5408589295980603673 ) ) ;
#13352 = ORIENTED_EDGE ( 'NONE', *, *, #23772, .F. ) ;
#13353 = CARTESIAN_POINT ( 'NONE',  ( 3.728136974946417492, 6.765255174955887796, 2.739693761753763113 ) ) ;
#13354 = ADVANCED_FACE ( 'NONE', ( #1319 ), #16852, .T. ) ;
#13355 = CARTESIAN_POINT ( 'NONE',  ( -20.51686376604223128, 129.1072961674477710, -0.4099757654675940111 ) ) ;
#13356 = CARTESIAN_POINT ( 'NONE',  ( 13.17422243436029916, 17.14500000000093394, 5.016499999999999737 ) ) ;
#13357 = CARTESIAN_POINT ( 'NONE',  ( 2.292992513364368268, 106.8193516554411531, 4.820700389358663962 ) ) ;
#13358 = CARTESIAN_POINT ( 'NONE',  ( 7.873896660004363390, 122.1234394815680986, 0.8695851236811991125 ) ) ;
#13359 = ADVANCED_FACE ( 'NONE', ( #14276 ), #8419, .T. ) ;
#13360 = CARTESIAN_POINT ( 'NONE',  ( 2.854375549615681962, 5.100648791940559867, -3.633247542873777380 ) ) ;
#13361 = CARTESIAN_POINT ( 'NONE',  ( 21.15273274666895276, 151.2337125027825095, 1.710087910014103985 ) ) ;
#13362 = CARTESIAN_POINT ( 'NONE',  ( -0.09909826073589839135, 106.8097931225389630, 4.959282197179073925 ) ) ;
#13364 = CARTESIAN_POINT ( 'NONE',  ( 15.00359386227399483, 154.7288491705591866, -1.534247969496847164 ) ) ;
#13363 = DIRECTION ( 'NONE',  ( 5.188838149069472160E-16, -1.699382548006136559E-16, -1.000000000000000000 ) ) ;
#13365 = CARTESIAN_POINT ( 'NONE',  ( 3.679437910380295218, 2.726752568732802917, 2.794697870780981752 ) ) ;
#13366 = CARTESIAN_POINT ( 'NONE',  ( 0.006370369177271557534, 117.0014201992989058, -0.3187993231787206727 ) ) ;
#13367 = ADVANCED_FACE ( 'NONE', ( #20454 ), #12634, .T. ) ;
#13368 = AXIS2_PLACEMENT_3D ( 'NONE', #25299, #9123, #35111 ) ;
#13369 = ORIENTED_EDGE ( 'NONE', *, *, #21698, .F. ) ;
#13370 = CARTESIAN_POINT ( 'NONE',  ( -3.009276887026423264, 44.28946620154572855, 1.210121013456480377 ) ) ;
#13371 = AXIS2_PLACEMENT_3D ( 'NONE', #19717, #32737, #16529 ) ;
#13372 = CARTESIAN_POINT ( 'NONE',  ( -7.065481736843254090, 122.0164807696326790, 0.1187983231582535742 ) ) ;
#13373 = CARTESIAN_POINT ( 'NONE',  ( 3.833788745076180060, -15.06587152019073272, 5.274579322627055866 ) ) ;
#13374 = CARTESIAN_POINT ( 'NONE',  ( -44.77556674759969013, 21.10465188057021280, 3.405155276520678065 ) ) ;
#13375 = CARTESIAN_POINT ( 'NONE',  ( -2.321297342765445748, 107.3035951680803635, -4.704727343862274758 ) ) ;
#13376 = ORIENTED_EDGE ( 'NONE', *, *, #29579, .T. ) ;
#13377 = CARTESIAN_POINT ( 'NONE',  ( 6.111605970564418122, 157.2590385278250267, 1.959406070573513459 ) ) ;
#13378 = LINE ( 'NONE', #6780, #28358 ) ;
#13379 = CARTESIAN_POINT ( 'NONE',  ( -7.961576494521615643, 72.55615504727386167, -1.269999999999996243 ) ) ;
#13380 = CIRCLE ( 'NONE', #37193, 0.5079999999999993410 ) ;
#13381 = CARTESIAN_POINT ( 'NONE',  ( -22.85738479169587123, 148.8343141121478652, 0.6244747819152592916 ) ) ;
#13382 = CARTESIAN_POINT ( 'NONE',  ( 7.231359443275770182, 22.16797014818540745, 4.386519482779798196 ) ) ;
#13383 = CARTESIAN_POINT ( 'NONE',  ( 15.62286502882988870, 121.0226940419799462, -0.1111101786179099632 ) ) ;
#13384 = CARTESIAN_POINT ( 'NONE',  ( -5.322370863981875644, 57.14999999999976410, -5.239063870260801004 ) ) ;
#13385 = AXIS2_PLACEMENT_3D ( 'NONE', #31450, #8244, #21216 ) ;
#13386 = DIRECTION ( 'NONE',  ( 0.9998004120163609398, 0.000000000000000000, 0.01997839162482749342 ) ) ;
#13387 = CARTESIAN_POINT ( 'NONE',  ( -47.01877684503696742, 24.36789988528162354, 2.430126310640454257 ) ) ;
#13388 = CARTESIAN_POINT ( 'NONE',  ( 1.819893491534947838, -15.08787143633222350, 5.611221046887520103 ) ) ;
#13389 = CARTESIAN_POINT ( 'NONE',  ( -48.82738941085167284, 18.57305038084609095, 5.399437279161905856 ) ) ;
#13390 = DIRECTION ( 'NONE',  ( -0.7284927773988648658, -0.6850534820564654348, -3.970048430162226266E-15 ) ) ;
#13391 = CARTESIAN_POINT ( 'NONE',  ( -4.387617986301902917, 118.1845766253724150, 0.4238482731264395231 ) ) ;
#13392 = CARTESIAN_POINT ( 'NONE',  ( -58.29601494275114959, -0.1585044380288253008, -0.03613930236864761059 ) ) ;
#13393 = AXIS2_PLACEMENT_3D ( 'NONE', #5822, #29427, #41818 ) ;
#13394 = ORIENTED_EDGE ( 'NONE', *, *, #21517, .F. ) ;
#13395 = CARTESIAN_POINT ( 'NONE',  ( -47.02779878473986486, 24.11651466984139702, 2.637840241488476511 ) ) ;
#13397 = ADVANCED_FACE ( 'NONE', ( #29200 ), #3659, .F. ) ;
#13396 = CARTESIAN_POINT ( 'NONE',  ( -8.314269420833845459, 119.9197522654141750, -1.446063649029603715 ) ) ;
#13398 = CARTESIAN_POINT ( 'NONE',  ( -6.073876170729706203, 119.5347744825833871, -0.5156133147040063980 ) ) ;
#13399 = CARTESIAN_POINT ( 'NONE',  ( 4.441115804996636385, 118.1267861108847086, 0.7297787586869709520 ) ) ;
#13400 = CARTESIAN_POINT ( 'NONE',  ( -6.488156926834150795, 121.4051597255373025, -0.7118474008431249223 ) ) ;
#13401 = CARTESIAN_POINT ( 'NONE',  ( -2.487218026922475733, 115.7030328841145206, -1.696577405177432496 ) ) ;
#13402 = DIRECTION ( 'NONE',  ( -5.188838149069471174E-16, 1.699382548006136313E-16, 1.000000000000000000 ) ) ;
#13403 = CARTESIAN_POINT ( 'NONE',  ( 5.252825482164369397, 116.2501875120488393, -0.9643948023431453409 ) ) ;
#13404 = CARTESIAN_POINT ( 'NONE',  ( -17.23725050067796616, 146.8699245690979751, -2.055247338431126725 ) ) ;
#13405 = DIRECTION ( 'NONE',  ( -1.000000000000000000, 1.011795553208986377E-16, 0.000000000000000000 ) ) ;
#13406 = CARTESIAN_POINT ( 'NONE',  ( -0.02969037535081191920, 158.7301711276701894, 1.485827791648137497 ) ) ;
#13407 = CARTESIAN_POINT ( 'NONE',  ( 8.060916924639187187, 121.3839393899244925, -0.8986322262796456739 ) ) ;
#13408 = CARTESIAN_POINT ( 'NONE',  ( -15.38354879105530237, 147.8362818251703459, -0.1740999797858117648 ) ) ;
#13409 = ADVANCED_FACE ( 'NONE', ( #30670 ), #27484, .T. ) ;
#13410 = CARTESIAN_POINT ( 'NONE',  ( -4.478778176974229197, 3.316883148187759645, 1.141857468124592101 ) ) ;
#13411 = CARTESIAN_POINT ( 'NONE',  ( 21.68922513019249010, 151.4054434770023363, 1.149106048033103011 ) ) ;
#13412 = CARTESIAN_POINT ( 'NONE',  ( -8.095114962461808616, 74.19100168833409725, -1.523999999999996691 ) ) ;
#13413 = CARTESIAN_POINT ( 'NONE',  ( 1.863517626568274910, -15.41251410767331720, 5.374852164437769808 ) ) ;
#13414 = CARTESIAN_POINT ( 'NONE',  ( -18.16172641238603802, 140.6071502257508143, 1.752259283733317519 ) ) ;
#13415 = CARTESIAN_POINT ( 'NONE',  ( 0.9436776830090995993, 12.87300645547595046, -0.2395577073833762005 ) ) ;
#13416 = CARTESIAN_POINT ( 'NONE',  ( -10.68516669180073286, 157.9381250348597234, -0.6779181152352149464 ) ) ;
#13417 = CIRCLE ( 'NONE', #12739, 0.6350000000000001199 ) ;
#13418 = EDGE_CURVE ( 'NONE', #41583, #13983, #19992, .T. ) ;
#13419 = CARTESIAN_POINT ( 'NONE',  ( 0.7508863055360318617, -11.68651920905074348, 0.6198408032357946018 ) ) ;
#13420 = ORIENTED_EDGE ( 'NONE', *, *, #7115, .T. ) ;
#13421 = EDGE_LOOP ( 'NONE', ( #1052, #39524, #39947, #15065 ) ) ;
#13422 = CARTESIAN_POINT ( 'NONE',  ( -46.62078961162516322, 17.34433182989875277, 0.7188397291161463531 ) ) ;
#13423 = CARTESIAN_POINT ( 'NONE',  ( 5.925882289753468868, 120.8604418758245487, 0.3792092984231499875 ) ) ;
#13424 = APPLICATION_PROTOCOL_DEFINITION ( 'draft international standard', 'automotive_design', 1998, #9111 ) ;
#13425 = CARTESIAN_POINT ( 'NONE',  ( -11.89914747278639950, 128.3619849303985632, 0.5991027734528264759 ) ) ;
#13426 = CARTESIAN_POINT ( 'NONE',  ( 2.309263497243444263, -14.96449433386182193, 5.702862618531368888 ) ) ;
#13427 = CARTESIAN_POINT ( 'NONE',  ( 17.39219791206827992, 147.8988302317391117, -1.461875531624039493 ) ) ;
#13428 = CONICAL_SURFACE ( 'NONE', #10680, 16.60960244842765476, 0.7853981633974488341 ) ;
#13429 = CARTESIAN_POINT ( 'NONE',  ( -19.80203545474871518, 147.6055923437354238, -2.520003004638577515 ) ) ;
#13430 = EDGE_CURVE ( 'NONE', #1544, #32690, #28153, .T. ) ;
#13431 = FACE_OUTER_BOUND ( 'NONE', #24787, .T. ) ;
#13432 = CARTESIAN_POINT ( 'NONE',  ( 3.074000544403499902, -13.70685301784095600, 1.494313880732895283 ) ) ;
#13433 = CARTESIAN_POINT ( 'NONE',  ( -6.430405882401983853, 30.45907221301710877, 0.4699959139286034593 ) ) ;
#13434 = CARTESIAN_POINT ( 'NONE',  ( 0.6527697516717059223, 156.3069099058775748, -0.1169209421757346490 ) ) ;
#13435 = AXIS2_PLACEMENT_3D ( 'NONE', #30681, #2578, #25549 ) ;
#13436 = ORIENTED_EDGE ( 'NONE', *, *, #40122, .F. ) ;
#13437 = CARTESIAN_POINT ( 'NONE',  ( -3.562848200393185838, 109.2372022974361698, 3.773768304531518236 ) ) ;
#13438 = FACE_OUTER_BOUND ( 'NONE', #11280, .T. ) ;
#13439 = LINE ( 'NONE', #39, #31346 ) ;
#13440 = DIRECTION ( 'NONE',  ( 5.188838149069472160E-16, -1.699382548006136559E-16, -1.000000000000000000 ) ) ;
#13441 = CARTESIAN_POINT ( 'NONE',  ( 8.060084350832182665, 158.6724238832827609, 0.05135189671889815732 ) ) ;
#13442 = CARTESIAN_POINT ( 'NONE',  ( -5.966545996697778520, 118.9610140496397719, 0.3495452691818400348 ) ) ;
#13443 = AXIS2_PLACEMENT_3D ( 'NONE', #10587, #20367, #33389 ) ;
#13444 = CARTESIAN_POINT ( 'NONE',  ( 8.515285667870289099E-16, 8.844871939465425825, 0.000000000000000000 ) ) ;
#13445 = CARTESIAN_POINT ( 'NONE',  ( -24.23745918283205114, 82.38670122043342303, -1.270000000000006457 ) ) ;
#13446 = CARTESIAN_POINT ( 'NONE',  ( 0.3600194693791573530, 38.02539389153889005, -1.148431998888613359 ) ) ;
#13447 = CARTESIAN_POINT ( 'NONE',  ( 4.941607502190644041, 118.3881331334009985, 1.039683250452205998 ) ) ;
#13448 = CARTESIAN_POINT ( 'NONE',  ( -4.487480840803009130, 27.34045677879159442, -1.100063755011520872 ) ) ;
#13449 = CARTESIAN_POINT ( 'NONE',  ( 7.636339006008190822, 27.50728337528610012, -3.595707551023701765 ) ) ;
#13450 = CARTESIAN_POINT ( 'NONE',  ( -2.478289490271501805, 117.4827286966103941, -0.7432425970007181526 ) ) ;
#13451 = CARTESIAN_POINT ( 'NONE',  ( -2.269084004857128800, 124.1308405194309188, -0.09931761310301590040 ) ) ;
#13453 = CARTESIAN_POINT ( 'NONE',  ( -17.14499999999999957, 71.11999999999999034, -5.016499999999999737 ) ) ;
#13452 = B_SPLINE_CURVE_WITH_KNOTS ( 'NONE', 3,
 ( #24580, #11390, #14577, #14996, #21797, #31407, #15421, #15207, #37383, #34201 ),
 .UNSPECIFIED., .F., .F.,
 ( 4, 2, 2, 2, 4 ),
 ( 0.0001356198500382660844, 0.001295386987695697732, 0.002455154125353129109, 0.003614921263010560919, 0.004774688400667992730 ),
 .UNSPECIFIED. ) ;
#13454 = CARTESIAN_POINT ( 'NONE',  ( -3.368418438749888111, 109.1383545882859778, -3.951708265540383014 ) ) ;
#13455 = CARTESIAN_POINT ( 'NONE',  ( 3.054645280121299766, 105.1240653689918645, 4.374269570515916250 ) ) ;
#13456 = CARTESIAN_POINT ( 'NONE',  ( -4.631227783250409402, 22.10816835407601744, -0.05711764529929251599 ) ) ;
#13457 = CARTESIAN_POINT ( 'NONE',  ( -4.476425760464393555, 71.61790547347303004, 1.270000000000004903 ) ) ;
#13458 = CARTESIAN_POINT ( 'NONE',  ( 1.650612623617701257E-15, 17.14499999999999957, 0.000000000000000000 ) ) ;
#13459 = CARTESIAN_POINT ( 'NONE',  ( 3.282182858002726356, -14.11059071864860570, 3.604430013830858037 ) ) ;
#13460 = CARTESIAN_POINT ( 'NONE',  ( 2.162440637018669065, 123.3349985135950959, -0.07568789353404296871 ) ) ;
#13461 = CARTESIAN_POINT ( 'NONE',  ( -20.72298665840535037, 132.2482564273973935, 0.5730191400310229444 ) ) ;
#13462 = FACE_OUTER_BOUND ( 'NONE', #16109, .T. ) ;
#13463 = EDGE_LOOP ( 'NONE', ( #21621, #1657, #32103, #28403 ) ) ;
#13464 = DIRECTION ( 'NONE',  ( -0.9454731675810352787, 0.3256999990547799206, -7.420046207093943154E-15 ) ) ;
#13465 = ORIENTED_EDGE ( 'NONE', *, *, #20356, .T. ) ;
#13466 = CYLINDRICAL_SURFACE ( 'NONE', #3623, 5.588000000000006295 ) ;
#13467 = CARTESIAN_POINT ( 'NONE',  ( 5.836094479182562189, -14.94293577981173371, 0.6207079514943552034 ) ) ;
#13468 = CARTESIAN_POINT ( 'NONE',  ( -19.50252919055214207, 149.6234262069624492, 1.702160239338572634 ) ) ;
#13469 = CARTESIAN_POINT ( 'NONE',  ( 7.954494586186791061, 118.5968412048868288, -0.8561882949445157598 ) ) ;
#13470 = ADVANCED_FACE ( 'NONE', ( #23856 ), #33613, .T. ) ;
#13471 = CARTESIAN_POINT ( 'NONE',  ( 0.9679928046509989059, 27.93285725408814812, -0.1178628334679577422 ) ) ;
#13472 = CARTESIAN_POINT ( 'NONE',  ( -58.80888331074255859, -0.2806509898663787084, -0.1196884892477749346 ) ) ;
#13473 = ORIENTED_EDGE ( 'NONE', *, *, #24839, .T. ) ;
#13474 = CARTESIAN_POINT ( 'NONE',  ( -58.35474420885217484, -0.2600319066113354616, -0.1537082109189478740 ) ) ;
#13475 = CARTESIAN_POINT ( 'NONE',  ( 0.1664298668078588450, 110.3683645023726427, 3.586750284817682211 ) ) ;
#13476 = CARTESIAN_POINT ( 'NONE',  ( -4.645572480595541620, 117.9340260526530813, 0.7769932229682322555 ) ) ;
#13477 = CARTESIAN_POINT ( 'NONE',  ( -8.784047514290692860, 154.8283212766472445, 1.235621501372049735 ) ) ;
#13478 = LINE ( 'NONE', #30496, #4186 ) ;
#13479 = EDGE_CURVE ( 'NONE', #702, #25607, #11154, .T. ) ;
#13480 = CARTESIAN_POINT ( 'NONE',  ( 18.13417818756197519, 144.6555253171603397, -1.679261103697790913 ) ) ;
#13481 = CARTESIAN_POINT ( 'NONE',  ( -13.21388725472906955, 155.5383117973235585, -2.112422614401994636 ) ) ;
#13482 = CARTESIAN_POINT ( 'NONE',  ( -57.36719850051837000, 1.975114663830185302, -1.756955940785672077 ) ) ;
#13483 = MECHANICAL_DESIGN_GEOMETRIC_PRESENTATION_REPRESENTATION (  '', ( #26389 ), #578 ) ;
#13484 = ORIENTED_EDGE ( 'NONE', *, *, #15651, .T. ) ;
#13485 = CARTESIAN_POINT ( 'NONE',  ( 4.378236034317057879, 118.1843938197233683, -0.4336838323394221484 ) ) ;
#13486 = CARTESIAN_POINT ( 'NONE',  ( 15.50313878892739972, 143.5853813351167219, -0.4270882868188063952 ) ) ;
#13487 = EDGE_LOOP ( 'NONE', ( #19062, #24410, #18836, #16862 ) ) ;
#13488 = CARTESIAN_POINT ( 'NONE',  ( -9.288997298956406468, 155.0893615026619159, -1.903066234436350701 ) ) ;
#13489 = CARTESIAN_POINT ( 'NONE',  ( 2.352443540978347958, -15.20488079220741540, 4.935102241435597392 ) ) ;
#13490 = CYLINDRICAL_SURFACE ( 'NONE', #34725, 12.69999999999999751 ) ;
#13491 = CIRCLE ( 'NONE', #39337, 0.2539999999999937863 ) ;
#13492 = CARTESIAN_POINT ( 'NONE',  ( -57.83370854706706865, 0.8645507274500086048, 1.063039573801799031 ) ) ;
#13493 = CARTESIAN_POINT ( 'NONE',  ( 4.428293322310913993, 12.87204911218450576, 1.319288874004734158 ) ) ;
#13494 = CARTESIAN_POINT ( 'NONE',  ( 17.19591734316806608, 148.1877419978735873, 2.150982665507991776 ) ) ;
#13495 = CARTESIAN_POINT ( 'NONE',  ( 2.996590608344533280, 39.20946620154573026, -0.5752477518260917799 ) ) ;
#13496 = CARTESIAN_POINT ( 'NONE',  ( 3.043391175932955495, 18.63480288530714191, -3.501419995799015528 ) ) ;
#13497 = CARTESIAN_POINT ( 'NONE',  ( 12.91493749300776095, 133.8340822528099636, 0.3749514369420006155 ) ) ;
#13498 = CARTESIAN_POINT ( 'NONE',  ( -7.921807157844598102, 72.80702234259206307, -1.269999999999996243 ) ) ;
#13499 = CARTESIAN_POINT ( 'NONE',  ( -54.02436534585504546, 7.965282956745534548, -1.622780670314687868 ) ) ;
#13500 = CARTESIAN_POINT ( 'NONE',  ( -2.182713281679669937, 116.1939960727429622, -0.1100263013286016944 ) ) ;
#13501 = DIRECTION ( 'NONE',  ( -4.017660918040594346E-17, 1.000000000000000000, 2.376309959284834438E-19 ) ) ;
#13502 = DIRECTION ( 'NONE',  ( 0.8745520943968249084, -0.4849315768086534528, 5.361993529360573944E-16 ) ) ;
#13503 = CARTESIAN_POINT ( 'NONE',  ( -6.034489779195991079E-14, 75.78546620154573077, 9.392091281095912196E-17 ) ) ;
#13504 = DIRECTION ( 'NONE',  ( 5.188838149069472160E-16, -1.699382548006136559E-16, -1.000000000000000000 ) ) ;
#13505 = CARTESIAN_POINT ( 'NONE',  ( -5.241362157049148429, 77.01756250000002524, 5.310945289804168468 ) ) ;
#13506 = CARTESIAN_POINT ( 'NONE',  ( -6.059261036834477032, 57.14999999999997726, 5.016499999999999737 ) ) ;
#13507 = DIRECTION ( 'NONE',  ( 5.188838149069472160E-16, -1.699382548006136559E-16, -1.000000000000000000 ) ) ;
#13508 = CARTESIAN_POINT ( 'NONE',  ( -57.66243511465492588, 3.255537196535582378, 0.1194500880619485950 ) ) ;
#13509 = CARTESIAN_POINT ( 'NONE',  ( -56.04137470801128273, 5.508142037592367757, 2.879222540163115074 ) ) ;
#13510 = CARTESIAN_POINT ( 'NONE',  ( -10.74909004363699161, 157.9381345072164038, 0.1376009798949089924 ) ) ;
#13511 = ORIENTED_EDGE ( 'NONE', *, *, #33709, .T. ) ;
#13512 = CARTESIAN_POINT ( 'NONE',  ( -53.18864123405685262, 14.74122628988702743, -1.932938280191028202 ) ) ;
#13513 = CARTESIAN_POINT ( 'NONE',  ( 6.973621732378568971, 121.9497932120239199, 0.04315832297541429691 ) ) ;
#13514 = AXIS2_PLACEMENT_3D ( 'NONE', #7534, #1780, #34359 ) ;
#13515 = ORIENTED_EDGE ( 'NONE', *, *, #37950, .F. ) ;
#13516 = CARTESIAN_POINT ( 'NONE',  ( -4.232597188052773518, 155.8470599587123502, -0.1762653075193722496 ) ) ;
#13517 = CARTESIAN_POINT ( 'NONE',  ( 3.633732803939692335, -15.12841498804032270, 5.400629595854979037 ) ) ;
#13518 = AXIS2_PLACEMENT_3D ( 'NONE', #128, #42089, #13306 ) ;
#13519 = CARTESIAN_POINT ( 'NONE',  ( -4.984194916311549761, 158.4862278396301178, 1.425929471103634549 ) ) ;
#13520 = CARTESIAN_POINT ( 'NONE',  ( -4.349660437102230048, 31.17966527223318707, -1.615541842050199461 ) ) ;
#13521 = CARTESIAN_POINT ( 'NONE',  ( 4.777924661806521200, 116.8922783744782379, 0.3800144224740277243 ) ) ;
#13522 = CARTESIAN_POINT ( 'NONE',  ( 15.76634901350801243, 146.5666095545782071, 0.5163113226649066467 ) ) ;
#13523 = CARTESIAN_POINT ( 'NONE',  ( -30.15519950990045572, 69.97033940222175374, 1.269999999999991802 ) ) ;
#13524 = CARTESIAN_POINT ( 'NONE',  ( -0.9385480264228447389, -6.289884363042010484, -0.2871545319985167044 ) ) ;
#13525 = CARTESIAN_POINT ( 'NONE',  ( -0.9036256862536363732, 116.4850453793277865, -0.1155468115323371875 ) ) ;
#13526 = DIRECTION ( 'NONE',  ( -0.9998004120163608288, 0.000000000000000000, -0.01997839162482749342 ) ) ;
#13527 = DIRECTION ( 'NONE',  ( 5.188838149069472160E-16, -1.699382548006136559E-16, -1.000000000000000000 ) ) ;
#13528 = EDGE_LOOP ( 'NONE', ( #8762, #13250, #25957, #37937, #30193 ) ) ;
#13529 = CARTESIAN_POINT ( 'NONE',  ( 2.225071688287161287, 116.2692689860753603, 0.1766109378387185069 ) ) ;
#13530 = VERTEX_POINT ( 'NONE', #33887 ) ;
#13531 = CARTESIAN_POINT ( 'NONE',  ( -18.15383854178437417, 147.5382818419693649, 1.618175512470155342 ) ) ;
#13532 = CARTESIAN_POINT ( 'NONE',  ( -57.71595586907567821, 1.118948197508295328, -1.187837037485634628 ) ) ;
#13533 = CARTESIAN_POINT ( 'NONE',  ( 18.77683424009538626, 152.0234722879370111, 2.226617664588433243 ) ) ;
#13534 = CARTESIAN_POINT ( 'NONE',  ( 2.527692779614272744, 158.0185616612000956, -1.624164342510254988 ) ) ;
#13535 = CARTESIAN_POINT ( 'NONE',  ( -0.8880852245287531588, 7.049514723814470862, -0.3999422104893632923 ) ) ;
#13536 = CARTESIAN_POINT ( 'NONE',  ( -14.46681479972627926, 121.7426775721902175, -1.517288920005034791 ) ) ;
#13537 = CARTESIAN_POINT ( 'NONE',  ( 4.621803021457706606, 118.0614903755723049, -0.5437508832788947588 ) ) ;
#13538 = CARTESIAN_POINT ( 'NONE',  ( 5.032151674051235979, 104.6144662015512381, 1.777523892075001388 ) ) ;
#13539 = CARTESIAN_POINT ( 'NONE',  ( 16.48541106618845831, 147.8801373804967341, -1.108338632072817243 ) ) ;
#13540 = CARTESIAN_POINT ( 'NONE',  ( -1.563936845556568089, 156.2577446057484281, -0.001723203835320021677 ) ) ;
#13541 = ORIENTED_EDGE ( 'NONE', *, *, #29947, .F. ) ;
#13542 = CARTESIAN_POINT ( 'NONE',  ( -6.601024023181220279, 120.1594786313440011, -1.214938174674062621 ) ) ;
#13543 = CARTESIAN_POINT ( 'NONE',  ( 5.240434970354078459, -15.39321860721029545, 1.015353449650246764 ) ) ;
#13544 = DIRECTION ( 'NONE',  ( 4.017660918040594346E-17, -1.000000000000000000, -2.376309959284834438E-19 ) ) ;
#13545 = CARTESIAN_POINT ( 'NONE',  ( -4.600069725331597859, 118.0596821417892954, -0.7231468346112266410 ) ) ;
#13546 = CARTESIAN_POINT ( 'NONE',  ( -45.82931853585289872, 22.14969803457954356, -3.600065900675656128 ) ) ;
#13547 = CARTESIAN_POINT ( 'NONE',  ( -17.14499999999999957, 71.11999999999999034, 5.016499999999999737 ) ) ;
#13548 = CARTESIAN_POINT ( 'NONE',  ( 10.38552121992528399, 122.0805278159965610, 1.592441429402150055 ) ) ;
#13549 = CYLINDRICAL_SURFACE ( 'NONE', #15455, 0.5080000000000002292 ) ;
#13550 = CIRCLE ( 'NONE', #16944, 3.683000000000001162 ) ;
#13551 = CARTESIAN_POINT ( 'NONE',  ( 1.794468298957800689, 116.4672891243423578, 0.03585774721038192947 ) ) ;
#13552 = CARTESIAN_POINT ( 'NONE',  ( 0.01634572621781915994, 29.22912819268679030, -8.429653881604959764 ) ) ;
#13553 = CARTESIAN_POINT ( 'NONE',  ( 4.372087114477248626, 155.8497297829079571, 0.6179351164228052973 ) ) ;
#13554 = CARTESIAN_POINT ( 'NONE',  ( 2.899870334229791791, 116.9538966677400254, -0.3598414239652114044 ) ) ;
#13555 = EDGE_CURVE ( 'NONE', #32240, #33599, #19741, .T. ) ;
#13556 = CARTESIAN_POINT ( 'NONE',  ( -46.33290834485746501, 20.59977736898093070, -4.631597800898671125 ) ) ;
#13557 = ORIENTED_EDGE ( 'NONE', *, *, #12649, .T. ) ;
#13558 = CARTESIAN_POINT ( 'NONE',  ( 0.1700004239520251370, 118.7629491485454025, 1.279869604491548296 ) ) ;
#13559 = CARTESIAN_POINT ( 'NONE',  ( -20.69945920510674142, 152.5542719854981044, -0.3887601451951301912 ) ) ;
#13560 = VERTEX_POINT ( 'NONE', #4924 ) ;
#13561 = CARTESIAN_POINT ( 'NONE',  ( 6.724651104264945722, 120.8999252434172291, -0.7604862180030697028 ) ) ;
#13562 = CARTESIAN_POINT ( 'NONE',  ( 6.475684456959278634, -13.49251406434824574, 0.1304084665236045215 ) ) ;
#13563 = CARTESIAN_POINT ( 'NONE',  ( -4.292261259499774440, 155.8363458669846864, -0.4108933393057503380 ) ) ;
#13564 = CARTESIAN_POINT ( 'NONE',  ( 3.919216764667305064, -12.20455369412110080, 1.363517133079271026 ) ) ;
#13565 = CARTESIAN_POINT ( 'NONE',  ( -19.81309253913748947, 152.3633698111425758, 1.013446639353942968 ) ) ;
#13566 = CARTESIAN_POINT ( 'NONE',  ( 7.213960532363566713, 83.56599999999998829, -1.904999999999999805 ) ) ;
#13567 = CARTESIAN_POINT ( 'NONE',  ( 16.27462974253330685, 121.4070763266325628, 0.3766275504196341939 ) ) ;
#13568 = EDGE_CURVE ( 'NONE', #4125, #120, #18621, .T. ) ;
#13569 = VERTEX_POINT ( 'NONE', #14264 ) ;
#13570 = CARTESIAN_POINT ( 'NONE',  ( 4.586363120317823672, -1.655842793181455663, -0.6244342276643227718 ) ) ;
#13571 = CARTESIAN_POINT ( 'NONE',  ( -15.73471677569744287, 120.8416612192341972, -0.3144170877231854955 ) ) ;
#13572 = DIRECTION ( 'NONE',  ( -0.01997839162482761832, -1.040247600000950455E-18, 0.9998004120163610509 ) ) ;
#13573 = CARTESIAN_POINT ( 'NONE',  ( 2.780396738703073911, 107.4069940011556383, 4.543958154617097733 ) ) ;
#13574 = CARTESIAN_POINT ( 'NONE',  ( 8.061196390534837164, 121.1687499546863336, 1.293492009120990716 ) ) ;
#13575 = AXIS2_PLACEMENT_3D ( 'NONE', #1018, #805, #1433 ) ;
#13576 = CARTESIAN_POINT ( 'NONE',  ( 2.901706292870370518, -4.507343114274551255, -3.632229383212865592 ) ) ;
#13577 = CARTESIAN_POINT ( 'NONE',  ( 15.68124023389185240, 122.9504679175852573, 1.501494826411870154 ) ) ;
#13578 = CARTESIAN_POINT ( 'NONE',  ( 15.26262975083392170, 148.0175730703490160, 0.3049836654617371079 ) ) ;
#13580 = CARTESIAN_POINT ( 'NONE',  ( 9.025716902755924309, 119.5326672034033777, -1.052790416315139144 ) ) ;
#13579 = CARTESIAN_POINT ( 'NONE',  ( 5.813542725970706648, 56.51499999999999346, 4.384680539058527948 ) ) ;
#13581 = CARTESIAN_POINT ( 'NONE',  ( 2.198398128136354934, 2.077049112184502278, 4.064154346441791965 ) ) ;
#13582 = CARTESIAN_POINT ( 'NONE',  ( -2.899385524442621875, 117.0242007548465608, -0.5112881796358939024 ) ) ;
#13583 = ORIENTED_EDGE ( 'NONE', *, *, #42077, .T. ) ;
#13584 = CARTESIAN_POINT ( 'NONE',  ( -4.305249565653826771, 155.8363458669846864, 0.2390946120805821085 ) ) ;
#13585 = CARTESIAN_POINT ( 'NONE',  ( 5.253367374056280070, -14.88852847978991356, 3.689182801501961428 ) ) ;
#13586 = CARTESIAN_POINT ( 'NONE',  ( -4.085839532347240066, 71.06758511999679229, -1.523999999999994026 ) ) ;
#13587 = CARTESIAN_POINT ( 'NONE',  ( -0.1908661700457686961, 105.7852372209750200, -5.338925892754766700 ) ) ;
#13588 = ORIENTED_EDGE ( 'NONE', *, *, #41797, .F. ) ;
#13589 = CARTESIAN_POINT ( 'NONE',  ( 9.864431837517868118, 120.7895603300898699, 1.595968683908904007 ) ) ;
#13590 = CARTESIAN_POINT ( 'NONE',  ( -9.094996104468895837, 78.64197151092922411, 1.904999999999988258 ) ) ;
#13591 = CARTESIAN_POINT ( 'NONE',  ( -18.01920641645601151, 83.84822824455467583, 1.523999999999996025 ) ) ;
#13592 = CARTESIAN_POINT ( 'NONE',  ( -20.00278215841964524, 152.4248492066682559, 0.8711105393690440346 ) ) ;
#13594 = EDGE_CURVE ( 'NONE', #35463, #33914, #295, .T. ) ;
#13593 = CARTESIAN_POINT ( 'NONE',  ( 8.378134419073882455, 22.78949214230337006, 1.148743996083190888 ) ) ;
#13595 = CARTESIAN_POINT ( 'NONE',  ( 16.02795213054438506, 143.8376908863262997, 1.609587254066635387 ) ) ;
#13596 = CIRCLE ( 'NONE', #40127, 5.080000000000006288 ) ;
#13597 = CARTESIAN_POINT ( 'NONE',  ( 1.900581966505874076, 116.7132768022172797, -0.2320997050762015623 ) ) ;
#13598 = CARTESIAN_POINT ( 'NONE',  ( -50.92517188622475288, 14.59490250589506921, 4.563427635915562774 ) ) ;
#13599 = CARTESIAN_POINT ( 'NONE',  ( -47.59569394876871939, 21.45978420380969354, 4.300550031832332643 ) ) ;
#13600 = LINE ( 'NONE', #24805, #23000 ) ;
#13601 = CARTESIAN_POINT ( 'NONE',  ( -53.00789483126595769, 12.40033530745290236, 4.180047681284801975 ) ) ;
#13602 = CARTESIAN_POINT ( 'NONE',  ( -58.36929466660706112, 0.2635729057794952701, 0.9100288767555340108 ) ) ;
#13603 = CARTESIAN_POINT ( 'NONE',  ( -4.496964070084271903, 118.1160052686005457, 0.5628395517699180672 ) ) ;
#13604 = CARTESIAN_POINT ( 'NONE',  ( -58.11144429832071268, 0.1746852717545849254, -0.04262357901410007005 ) ) ;
#13605 = B_SPLINE_CURVE_WITH_KNOTS ( 'NONE', 3,
 ( #21069, #14887, #8304, #37696, #18499, #24271, #21274, #11079, #40897, #11701, #27272, #33885, #34304, #28097, #24904, #8725, #37903, #41109, #17668, #30668, #24688, #5133, #21686, #4922, #40287, #1516, #37276, #5334, #8518, #21476, #18289, #34508, #34094, #17877, #11915, #30880, #34711, #1721, #14677, #27683, #24474, #35551, #41322, #2562, #25115, #32344, #35336, #22522, #15934 ),
 .UNSPECIFIED., .F., .F.,
 ( 4, 1, 1, 1, 1, 1, 1, 1, 1, 1, 1, 1, 1, 1, 1, 1, 1, 1, 1, 1, 1, 1, 1, 1, 1, 1, 1, 1, 1, 1, 1, 1, 1, 1, 1, 1, 1, 1, 1, 1, 1, 1, 1, 1, 1, 1, 4 ),
 ( 0.000000000000000000, 0.007812500000000000000, 0.01562500000000000000, 0.02343750000000000000, 0.03125000000000000000, 0.04687500000000000000, 0.06250000000000000000, 0.07812500000000000000, 0.09375000000000000000, 0.1093750000000000000, 0.1250000000000000000, 0.1406250000000000000, 0.1562500000000000000, 0.1875000000000000000, 0.2187500000000000000, 0.2500000000000000000, 0.2812500000000000000, 0.3125000000000000000, 0.3281250000000000000, 0.3437500000000000000, 0.3750000000000000000, 0.4062500000000000000, 0.4375000000000000000, 0.4687500000000000000, 0.5000000000000000000, 0.5312500000000000000, 0.5625000000000000000, 0.5937500000000000000, 0.6250000000000000000, 0.6562500000000000000, 0.6718750000000000000, 0.6875000000000000000, 0.7187500000000000000, 0.7500000000000000000, 0.7812500000000000000, 0.8125000000000000000, 0.8437500000000000000, 0.8750000000000000000, 0.8906250000000000000, 0.9062500000000000000, 0.9218750000000000000, 0.9375000000000000000, 0.9531250000000000000, 0.9687500000000000000, 0.9765625000000000000, 0.9843750000000000000, 1.000000000000000000 ),
 .UNSPECIFIED. ) ;
#13606 = ORIENTED_EDGE ( 'NONE', *, *, #36604, .F. ) ;
#13607 = CARTESIAN_POINT ( 'NONE',  ( -47.00787117332040310, 24.49876931072293829, 2.333946431867817584 ) ) ;
#13608 =( BOUNDED_SURFACE ( )  B_SPLINE_SURFACE ( 3, 2, ( 
 ( #21639, #1876, #41273 ),
 ( #34664, #38284, #28050 ),
 ( #37430, #2302, #25279 ),
 ( #41059, #28685, #34253 ),
 ( #5917, #31241, #41485 ),
 ( #11869, #11652, #31036 ),
 ( #2085, #24859, #31675 ),
 ( #37855, #5492, #2724 ),
 ( #18453, #31458, #15262 ),
 ( #9103, #28266, #8886 ),
 ( #22068, #35095, #12078 ),
 ( #34879, #18879, #35723 ) ),
 .UNSPECIFIED., .F., .F., .T. ) 
 B_SPLINE_SURFACE_WITH_KNOTS ( ( 4, 2, 2, 2, 2, 4 ),
 ( 3, 3 ),
 ( 0.000000000000000000, 0.0003677900075225773967, 0.0007355800150451547934, 0.001103370022567732190, 0.001287265026329020888, 0.001471160030090309587 ),
 ( 0.000000000000000000, 1.000000000000000000 ),
 .UNSPECIFIED. ) 
 GEOMETRIC_REPRESENTATION_ITEM ( )  RATIONAL_B_SPLINE_SURFACE ( (
 ( 1.000000000000000000, 0.7071067811865475727, 1.000000000000000000),
 ( 1.000000000000000000, 0.7071067811865475727, 1.000000000000000000),
 ( 1.000000000000000000, 0.7071067811865552333, 1.000000000000000000),
 ( 1.000000000000000000, 0.7071067811865552333, 1.000000000000000000),
 ( 1.000000000000000000, 0.7071067811865553443, 1.000000000000000000),
 ( 1.000000000000000000, 0.7071067811865553443, 1.000000000000000000),
 ( 1.000000000000000000, 0.7071067811865398012, 1.000000000000000000),
 ( 1.000000000000000000, 0.7071067811865398012, 1.000000000000000000),
 ( 1.000000000000000000, 0.7071067811865514585, 1.000000000000000000),
 ( 1.000000000000000000, 0.7071067811865514585, 1.000000000000000000),
 ( 1.000000000000000000, 0.7071067811865514585, 1.000000000000000000),
 ( 1.000000000000000000, 0.7071067811865514585, 1.000000000000000000) ) ) 
 REPRESENTATION_ITEM ( '' )  SURFACE ( )  );
#13609 = CARTESIAN_POINT ( 'NONE',  ( -8.283754562202487293, 120.0681802063006671, -1.449964621888376159 ) ) ;
#13610 = CARTESIAN_POINT ( 'NONE',  ( -6.667064533335244292, 121.2389289720308199, -0.3413157713140473892 ) ) ;
#13611 = CARTESIAN_POINT ( 'NONE',  ( 4.547318138317117509, 118.0745339805481109, 0.7854269464174529203 ) ) ;
#13612 = CARTESIAN_POINT ( 'NONE',  ( -12.19070665030426071, 151.9982576965888654, -1.154562729007634569 ) ) ;
#13613 =( NAMED_UNIT ( * ) SI_UNIT ( $, .STERADIAN. ) SOLID_ANGLE_UNIT ( ) );
#13614 = CARTESIAN_POINT ( 'NONE',  ( 4.811878810637661097, 117.9496053154559689, -0.9251022342672158283 ) ) ;
#13615 = CARTESIAN_POINT ( 'NONE',  ( 7.328771362700555514, 123.0350022594044219, 0.07777345538051000373 ) ) ;
#13616 = CARTESIAN_POINT ( 'NONE',  ( -13.72925640114938872, 131.0408573235120571, -1.723107598632782844 ) ) ;
#13617 = CARTESIAN_POINT ( 'NONE',  ( -0.002459394113084579191, 156.3065584682211124, 0.1230781383047673677 ) ) ;
#13618 = CARTESIAN_POINT ( 'NONE',  ( 7.882738460396603308, 122.2119657951149918, -0.4812898729222590544 ) ) ;
#13619 = CARTESIAN_POINT ( 'NONE',  ( -9.096994273319783275, 153.9681518559695803, -0.06573532333832052266 ) ) ;
#13620 = CARTESIAN_POINT ( 'NONE',  ( -4.515506726787251068, -6.291224493951820484, 1.111903093310195212 ) ) ;
#13621 = CARTESIAN_POINT ( 'NONE',  ( 5.832486214875661545, 117.3024554866451865, 0.6456718139904971121 ) ) ;
#13622 = DIRECTION ( 'NONE',  ( 5.188838149069472160E-16, -1.699382548006136559E-16, -1.000000000000000000 ) ) ;
#13623 = CARTESIAN_POINT ( 'NONE',  ( 3.134532381368876575, -15.16579696257060128, 3.749817985361381112 ) ) ;
#13624 = CARTESIAN_POINT ( 'NONE',  ( -13.18164045127540440, 153.9517556018257096, 1.734949727869876002 ) ) ;
#13625 = CARTESIAN_POINT ( 'NONE',  ( 0.9708619386763404080, 12.65153173543952470, -0.1022289352641109206 ) ) ;
#13626 = CARTESIAN_POINT ( 'NONE',  ( -22.96526709448186310, 149.8455236008688303, -1.052246632350672506 ) ) ;
#13627 = CARTESIAN_POINT ( 'NONE',  ( -0.8940008744714061928, 26.26452439613007428, -0.3861867617640990513 ) ) ;
#13628 = ORIENTED_EDGE ( 'NONE', *, *, #13329, .F. ) ;
#13629 = EDGE_CURVE ( 'NONE', #25488, #41561, #37080, .T. ) ;
#13630 = CARTESIAN_POINT ( 'NONE',  ( -44.35420297070785978, 19.68308750433651966, 0.4327882352162311097 ) ) ;
#13631 = CARTESIAN_POINT ( 'NONE',  ( 7.618479139564604985, 124.9344662015457317, 0.1522353441811855612 ) ) ;
#13632 = CARTESIAN_POINT ( 'NONE',  ( -4.498274173886023242, 155.8822484669112214, 0.6329996689149903766 ) ) ;
#13633 = CARTESIAN_POINT ( 'NONE',  ( 3.392078256862109953, -14.39927144874259035, 5.014931565121842461 ) ) ;
#13634 = CARTESIAN_POINT ( 'NONE',  ( 9.055011062051939064, 121.9018297702777858, -0.9711463333382074348 ) ) ;
#13635 = CARTESIAN_POINT ( 'NONE',  ( -7.562035183886322898, 119.9600249249614592, -1.380075063195379093 ) ) ;
#13636 = CARTESIAN_POINT ( 'NONE',  ( -0.2157595710058203831, 104.6144662015457243, 4.831689807522736579 ) ) ;
#13637 = CARTESIAN_POINT ( 'NONE',  ( 3.025122737553283869, -13.62787997529110662, 1.286645544439679156 ) ) ;
#13638 = CARTESIAN_POINT ( 'NONE',  ( -4.967168320455268571, 117.4023968188195681, -1.002192383175803503 ) ) ;
#13639 = CARTESIAN_POINT ( 'NONE',  ( 0.002459394112955782911, 156.3065584682211124, -0.1230781383047671457 ) ) ;
#13640 = ORIENTED_EDGE ( 'NONE', *, *, #30481, .T. ) ;
#13641 = EDGE_CURVE ( 'NONE', #1503, #34270, #41761, .T. ) ;
#13642 = CARTESIAN_POINT ( 'NONE',  ( -4.555615850703588876, 110.9173261774677712, 2.841647770357901504 ) ) ;
#13643 = CARTESIAN_POINT ( 'NONE',  ( 2.278431206749268245, 107.0260912999229390, 4.818171318492614041 ) ) ;
#13644 = DIRECTION ( 'NONE',  ( 4.017660918040594346E-17, -1.000000000000000000, -2.376309959284834438E-19 ) ) ;
#13645 = CIRCLE ( 'NONE', #24514, 5.588000000000006295 ) ;
#13646 = DIRECTION ( 'NONE',  ( 0.1906721105965186736, -0.9816537812491066273, 0.000000000000000000 ) ) ;
#13647 = CARTESIAN_POINT ( 'NONE',  ( 4.745947329130571823, 116.7839080817633430, -0.02307940527355892280 ) ) ;
#13648 = ADVANCED_FACE ( 'NONE', ( #30462 ), #1307, .T. ) ;
#13649 = CARTESIAN_POINT ( 'NONE',  ( -5.946884660761687869, 118.9717589635377664, 0.3494607991981762418 ) ) ;
#13650 = AXIS2_PLACEMENT_3D ( 'NONE', #33043, #16837, #29837 ) ;
#13651 = EDGE_CURVE ( 'NONE', #26382, #5996, #27687, .T. ) ;
#13652 = CARTESIAN_POINT ( 'NONE',  ( -6.507153519498132566E-14, 76.29346620154572634, 3.067795752821199360E-29 ) ) ;
#13653 = CARTESIAN_POINT ( 'NONE',  ( 11.82906070755491434, 56.41571150956137615, 5.016499999999999737 ) ) ;
#13654 = CARTESIAN_POINT ( 'NONE',  ( -4.399413851824025556, 32.38558793863810337, 0.9715087743876699156 ) ) ;
#13655 = CARTESIAN_POINT ( 'NONE',  ( 20.10299018766027146, 141.3454246894093274, 2.438971827487009580 ) ) ;
#13656 = CARTESIAN_POINT ( 'NONE',  ( -4.596079559025361583, 18.26954911218466648, 0.4757704999388879807 ) ) ;
#13657 = CARTESIAN_POINT ( 'NONE',  ( 0.8142577860443056537, 14.98675861574836077, 8.418590528086960845 ) ) ;
#13658 = CARTESIAN_POINT ( 'NONE',  ( 5.509788357450847940, 117.4222437278462223, -0.6928894233252995694 ) ) ;
#13659 = CARTESIAN_POINT ( 'NONE',  ( -2.216013192100319884, 123.7320667226965867, -0.1296889073052085173 ) ) ;
#13660 = CARTESIAN_POINT ( 'NONE',  ( 4.810181142648978891, 117.4081489754564274, 1.190371033444491244 ) ) ;
#13661 = PLANE ( 'NONE',  #5936 ) ;
#13662 = CARTESIAN_POINT ( 'NONE',  ( -0.003073426022617897335, 123.4679809879534247, 0.1538068059577180902 ) ) ;
#13663 = CARTESIAN_POINT ( 'NONE',  ( 1.790774717077139089, 25.13178105314743860, 4.274281468382033822 ) ) ;
#13664 = CARTESIAN_POINT ( 'NONE',  ( -33.20758249455312239, 49.81222039523557044, 1.269999999999993578 ) ) ;
#13665 = CARTESIAN_POINT ( 'NONE',  ( -23.45208337669106058, 146.8499405025503961, -0.4686284387228000226 ) ) ;
#13666 = CARTESIAN_POINT ( 'NONE',  ( 1.878022632408997250, -15.11918648689831990, 5.509382895440600336 ) ) ;
#13667 = CARTESIAN_POINT ( 'NONE',  ( 3.706399805698057826, 113.7286232773062125, -2.153009399082070452 ) ) ;
#13668 = CARTESIAN_POINT ( 'NONE',  ( -20.86923087398519172, 132.2939277659177151, 0.4710007621541096867 ) ) ;
#13669 = ADVANCED_FACE ( 'NONE', ( #34306 ), #27274, .T. ) ;
#13670 = CARTESIAN_POINT ( 'NONE',  ( -26.29578028364076658, 73.87584665086983193, 1.523999999999993360 ) ) ;
#13671 = ORIENTED_EDGE ( 'NONE', *, *, #17305, .F. ) ;
#13672 = CARTESIAN_POINT ( 'NONE',  ( -6.059261036834476144, 56.51499999999998636, 4.381499999999999950 ) ) ;
#13673 = EDGE_LOOP ( 'NONE', ( #21861, #21305 ) ) ;
#13674 = CARTESIAN_POINT ( 'NONE',  ( -2.803395127021860223, 31.26063551530791074, 0.8708390753670086637 ) ) ;
#13675 = CARTESIAN_POINT ( 'NONE',  ( 5.293312112441732609, -15.32963308811979886, 0.4416779358531437993 ) ) ;
#13676 = CARTESIAN_POINT ( 'NONE',  ( -0.4598942929540284497, 118.4074432378348689, 0.5883637925338035535 ) ) ;
#13677 = CARTESIAN_POINT ( 'NONE',  ( 15.22748671137934551, 123.1171956318823533, -1.061527106655570707 ) ) ;
#13678 = CARTESIAN_POINT ( 'NONE',  ( 4.560443952884764229, -11.68867000232777542, 0.6947937212093100445 ) ) ;
#13679 = CARTESIAN_POINT ( 'NONE',  ( -58.60178378695536594, -0.2365438316893033466, -0.4554716356075824701 ) ) ;
#13680 = ORIENTED_EDGE ( 'NONE', *, *, #37416, .T. ) ;
#13681 = CARTESIAN_POINT ( 'NONE',  ( -4.810636611593423595, 117.4081599864878598, -1.190287313834438532 ) ) ;
#13682 = CARTESIAN_POINT ( 'NONE',  ( 0.08587196332404170573, 108.5751225745497806, 4.267111774705385052 ) ) ;
#13683 = CARTESIAN_POINT ( 'NONE',  ( 0.000000000000000000, 0.000000000000000000, 0.000000000000000000 ) ) ;
#13684 = B_SPLINE_SURFACE_WITH_KNOTS ( 'NONE', 3, 3, ( 
 ( #40350, #17528, #20929, #7961, #7544, #4569, #14326, #14541, #30735, #27338, #30529, #26915, #27550, #33953, #24131, #40556, #33533, #33320, #39929, #17325, #4784, #24543, #953, #24340, #37344, #27125, #1159, #8164, #21132, #7334, #4988, #30948, #1788, #27751 ),
 ( #40761, #13921, #20292, #14124, #37976, #5405, #8801, #38195, #28175, #18997, #11772, #15384, #2633, #41824, #5620, #1995, #21548, #41180, #21760, #12416, #32001, #34365, #18361, #28808, #11983, #8374, #28389, #9221, #31795, #18576, #12200, #35008, #15592, #38410 ),
 ( #22179, #21339, #2840, #15799, #41395, #24763, #34578, #37761, #34786, #24977, #14958, #31585, #28597, #31156, #35209, #2423, #6036, #27959, #9011, #31367, #25191, #15169, #41606, #25408, #21976, #5828, #12618, #37550, #2210, #18783, #5198, #18152, #40968, #8585 ),
 ( #274, #16429, #16857, #19209, #6655, #13460, #23227, #39451, #9629, #32632, #13030, #6239, #29435, #3893, #29649, #60, #22596, #26020, #19833, #6442, #36260, #22387, #38818, #36047, #33062, #39029, #32847, #3679, #12822, #13248, #29007, #32217, #29218, #16641 ),
 ( #487, #695, #3253, #39236, #26232, #9837, #19619, #35628, #10046, #35411, #19417, #20044, #3050, #32423, #22803, #23018, #29857, #10254, #6861, #35840, #25605, #16008, #16213, #3467, #26448, #7080, #38614, #42024, #25809, #9419, #36678, #33488, #23658, #27082 ),
 ( #7915, #23873, #30480, #11099, #33906, #14491, #17484, #23439, #26872, #14079, #904, #33275, #39879, #21089, #26659, #4317, #20880, #13878, #10676, #36468, #4521, #4734, #24291, #40306, #7711, #10885, #7499, #1324, #20459, #14281, #27291, #7287, #17686, #17899 ),
 ( #40090, #17064, #20249, #17281, #30067, #36893, #30270, #20673, #1112, #11306, #1536, #33697, #24087, #4104, #37097, #30686, #27504, #40512, #37296, #8115, #34113, #4940, #30902, #13667, #39666, #10471, #2584, #11934, #34953, #31740, #14907, #8324, #18310, #9170 ),
 ( #37499, #24926, #15544, #41554, #28546, #27910, #8747, #31312, #24495, #5564, #22126, #5776, #2156, #40917, #15116, #38143, #24710, #12362, #40712, #11723, #12147, #35156, #28119, #8956, #21923, #31111, #18521, #5151, #21295, #5357, #18730, #18945, #41128, #25350 ),
 ( #15329, #31527, #37924, #21709, #37715, #2371, #11508, #8538, #38353, #34323, #21498, #34733, #41345, #5982, #1741, #25139, #28336, #14700, #18106, #34531, #27705, #1948, #432, #32795, #38557, #32161, #15955, #12768, #9576, #41969, #3195, #29599, #25552, #16375 ),
 ( #29380, #9991, #3626, #35783, #41765, #2995, #32367, #19156, #9370, #28951, #39398, #2790, #22545, #26179, #25758, #38765, #12565, #22751, #22963, #13403, #220, #25967, #29162, #35574, #6597, #6392, #19566, #32575, #22334, #35992, #36205, #3407, #28752, #8 ),
 ( #13195, #19362, #39182, #6806, #19775, #12974, #16158, #38975, #9783, #35357, #6187, #16591, #26393, #10200, #23171, #7027, #31951, #15747, #7864, #20404, #646, #40462, #40252, #20826, #30220, #11046, #33851, #33224, #26605, #36626, #27446, #20198, #36420, #17636 ),
 ( #4679, #4051, #27031, #7446, #13615, #23816, #11252, #24031, #33434, #17012, #4261, #14230, #850, #30638, #16804, #30011, #30427, #24236, #17224, #27238, #37047, #7238, #36837, #23388, #39612, #23605, #1481, #37246, #1060, #14437, #19994, #13824, #33012, #3840 ) ),
 .UNSPECIFIED., .F., .F., .F.,
 ( 4, 1, 1, 1, 1, 1, 3, 4 ),
 ( 4, 1, 1, 1, 1, 1, 1, 1, 1, 1, 1, 1, 1, 1, 1, 1, 1, 1, 1, 2, 1, 1, 1, 1, 1, 1, 1, 1, 1, 1, 4 ),
 ( 0.000000000000000000, 0.1666666666666666574, 0.2500000000000000000, 0.5000000000000000000, 0.5555555555555555802, 0.7500000000000000000, 1.000000000000000000, 1.010000000000000009 ),
 ( 0.000000000000000000, 0.02126250000000000015, 0.04252500000000000030, 0.06378749999999999698, 0.08505000000000000060, 0.1063125000000000042, 0.1275749999999999940, 0.1488374999999999837, 0.1701000000000000012, 0.1913624999999999909, 0.2126250000000000084, 0.2338874999999999704, 0.2551500000000000434, 0.2764124999999999499, 0.2870437499999999864, 0.2976749999999999674, 0.3083062500000000039, 0.3189375000000000404, 0.3295687499999999659, 0.3402000000000000024, 0.4226750000000000229, 0.5051499999999999879, 0.5876249999999998419, 0.6700999999999999179, 0.7525749999999999940, 0.7938125000000000320, 0.8350499999999999590, 0.8762874999999994419, 0.9175249999999994799, 0.9587624999999999620, 1.000000000000000000 ),
 .UNSPECIFIED. ) ;
#13685 = CARTESIAN_POINT ( 'NONE',  ( -17.03734119261612889, 146.7604995623492243, 1.248076303867124093 ) ) ;
#13686 = DIRECTION ( 'NONE',  ( -5.188838149069472160E-16, 1.699382548006136559E-16, 1.000000000000000000 ) ) ;
#13687 = CARTESIAN_POINT ( 'NONE',  ( 18.71424449056243233, 147.4429432625130119, -1.699796950208447788 ) ) ;
#13688 = CIRCLE ( 'NONE', #16368, 6.350000000000004974 ) ;
#13689 = CARTESIAN_POINT ( 'NONE',  ( -7.783141725463827321, 119.0983413489662297, -1.312215641098251950 ) ) ;
#13690 = FACE_OUTER_BOUND ( 'NONE', #40974, .T. ) ;
#13691 = ORIENTED_EDGE ( 'NONE', *, *, #20230, .F. ) ;
#13692 = CARTESIAN_POINT ( 'NONE',  ( 4.429221712000376954, 118.1654444364263128, -0.4667334324146756863 ) ) ;
#13693 = EDGE_CURVE ( 'NONE', #1790, #6660, #12529, .T. ) ;
#13694 = CARTESIAN_POINT ( 'NONE',  ( 9.185752227574047524, 123.6526633469202920, -0.3199782652467453303 ) ) ;
#13695 = VERTEX_POINT ( 'NONE', #33470 ) ;
#13696 = CARTESIAN_POINT ( 'NONE',  ( 2.867866294591228993, -15.05265924143639467, 4.220695585399262484 ) ) ;
#13697 = CARTESIAN_POINT ( 'NONE',  ( -26.51793118801306548, 72.98537704160715123, 1.523999999999993360 ) ) ;
#13698 = CARTESIAN_POINT ( 'NONE',  ( -58.31060438690772685, -0.1666892599193892099, 0.3090539641401659487 ) ) ;
#13699 = CARTESIAN_POINT ( 'NONE',  ( -4.556395268149300293, 8.773967715207941609, 0.7749943352582737699 ) ) ;
#13700 = CARTESIAN_POINT ( 'NONE',  ( 4.324763564747695632, 120.2039194668847699, 0.7996884002708145589 ) ) ;
#13701 = CARTESIAN_POINT ( 'NONE',  ( 2.988133089223356187, 39.20946620154573026, -0.1519989107391659100 ) ) ;
#13702 = AXIS2_PLACEMENT_3D ( 'NONE', #34339, #11526, #14505 ) ;
#13703 = EDGE_CURVE ( 'NONE', #40718, #25505, #23639, .T. ) ;
#13704 = CARTESIAN_POINT ( 'NONE',  ( 1.111903444298625754, 15.29877551736591812, 4.515507465039587665 ) ) ;
#13705 = CARTESIAN_POINT ( 'NONE',  ( 3.737471135337817607, 121.0798372856833538, 0.1416028149587414686 ) ) ;
#13706 = CARTESIAN_POINT ( 'NONE',  ( -4.522151473809593369, 110.7919029432140974, 2.894729270667253829 ) ) ;
#13707 = CARTESIAN_POINT ( 'NONE',  ( -55.77633192430580777, 4.649224570933515821, -0.8844362032702758336 ) ) ;
#13708 = CARTESIAN_POINT ( 'NONE',  ( -8.784945553904831783, 117.7269525811338013, -0.3943082114503992930 ) ) ;
#13709 = CARTESIAN_POINT ( 'NONE',  ( -1.028573857428271010, 117.3993836102140449, 1.440221441096896315 ) ) ;
#13710 = AXIS2_PLACEMENT_3D ( 'NONE', #35504, #22894, #6958 ) ;
#13711 = FACE_OUTER_BOUND ( 'NONE', #21682, .T. ) ;
#13712 = CARTESIAN_POINT ( 'NONE',  ( -5.078986093043186045, 81.62746620154572952, -0.1014902294541231709 ) ) ;
#13713 = CARTESIAN_POINT ( 'NONE',  ( -5.475330206976889436, 88.73331249999998249, 5.107412922131463695 ) ) ;
#13714 = DIRECTION ( 'NONE',  ( -5.206863593109713661E-17, 1.000000000000000000, -1.077750396879097183E-30 ) ) ;
#13715 = DIRECTION ( 'NONE',  ( 0.4849315768086480127, 0.8745520943968279060, 1.030032898892941415E-16 ) ) ;
#13716 = CARTESIAN_POINT ( 'NONE',  ( -58.62011547798931588, 0.4741971735572336755, 0.2911429440373402566 ) ) ;
#13717 = CARTESIAN_POINT ( 'NONE',  ( -58.30521585032268206, -0.1116666926106041347, 0.6575736669891736330 ) ) ;
#13718 = CARTESIAN_POINT ( 'NONE',  ( -18.44111676445476888, 125.1790410860780298, 0.1047302884851513127 ) ) ;
#13719 = ORIENTED_EDGE ( 'NONE', *, *, #17931, .T. ) ;
#13720 = CARTESIAN_POINT ( 'NONE',  ( -57.67985703563598321, 3.143487229238031588, -0.2637475255842378630 ) ) ;
#13721 = CARTESIAN_POINT ( 'NONE',  ( 7.791856601383843284, 122.6038259070386687, 0.04541553377301332101 ) ) ;
#13722 = EDGE_LOOP ( 'NONE', ( #11697, #24432, #41846, #6888 ) ) ;
#13723 = CARTESIAN_POINT ( 'NONE',  ( 3.653205933764129831, 115.7029491755316712, -1.478537451617223386 ) ) ;
#13724 = CARTESIAN_POINT ( 'NONE',  ( -15.76280660274407808, 145.9085485750152316, -0.3664889719343313867 ) ) ;
#13725 = CARTESIAN_POINT ( 'NONE',  ( 4.840206765044483994, -15.05961300585426166, 4.264492456498921946 ) ) ;
#13726 = AXIS2_PLACEMENT_3D ( 'NONE', #14955, #21757, #8582 ) ;
#13727 = CARTESIAN_POINT ( 'NONE',  ( -11.93281433870470742, 156.4809912657682673, 1.479000486392927138 ) ) ;
#13728 = CARTESIAN_POINT ( 'NONE',  ( 3.655561289726139140, 27.93047918286777076, -2.829280713513928180 ) ) ;
#13729 = CARTESIAN_POINT ( 'NONE',  ( 21.82265835376359675, 151.4369626909183637, 0.8820245880042207887 ) ) ;
#13730 = CARTESIAN_POINT ( 'NONE',  ( 12.76659075803674348, 133.6868103333486602, 0.4399761219218703556 ) ) ;
#13731 = FACE_OUTER_BOUND ( 'NONE', #4336, .T. ) ;
#13732 = CARTESIAN_POINT ( 'NONE',  ( 0.9340445150430609633, -0.5783478219614121008, -0.2901879621234355056 ) ) ;
#13733 = CARTESIAN_POINT ( 'NONE',  ( -0.3088162040007921827, 116.5752054743899038, -0.1648661904198056027 ) ) ;
#13734 = CARTESIAN_POINT ( 'NONE',  ( 6.059261036834400649, 64.39150124418098642, 5.016499999999999737 ) ) ;
#13735 = LINE ( 'NONE', #33552, #5755 ) ;
#13736 = VERTEX_POINT ( 'NONE', #24068 ) ;
#13737 = CARTESIAN_POINT ( 'NONE',  ( 2.232464228204602996, 116.2826474796002287, 0.1929315044139254531 ) ) ;
#13738 = CARTESIAN_POINT ( 'NONE',  ( -13.85609184427570995, 152.5163154464351294, 1.589750347114884166 ) ) ;
#13739 = CARTESIAN_POINT ( 'NONE',  ( -57.59849520485223451, 1.372415327657551032, -1.305467049941703594 ) ) ;
#13740 = CARTESIAN_POINT ( 'NONE',  ( 21.26307135201298948, 148.5140355411650717, 2.311892396764664070 ) ) ;
#13741 = CARTESIAN_POINT ( 'NONE',  ( 4.169621149806018501, 118.9132445967212419, -0.8414384147219282628 ) ) ;
#13742 = CARTESIAN_POINT ( 'NONE',  ( 0.7725557299734273631, -15.30006921971679112, -0.5871674697799584841 ) ) ;
#13743 = AXIS2_PLACEMENT_3D ( 'NONE', #30886, #7486, #4927 ) ;
#13744 = CARTESIAN_POINT ( 'NONE',  ( -20.53318969041758635, 136.3738900553462372, -2.061127768630951707 ) ) ;
#13745 = CARTESIAN_POINT ( 'NONE',  ( 4.652316817438794772, 118.0213487410945845, -0.6399539048371912786 ) ) ;
#13746 = DIRECTION ( 'NONE',  ( -0.2290273297124634233, 0.9734199927291296017, -2.580167833703404029E-15 ) ) ;
#13747 = CARTESIAN_POINT ( 'NONE',  ( 6.515494676151939224, 155.4519854478747902, -0.9200225795255460026 ) ) ;
#13748 = CARTESIAN_POINT ( 'NONE',  ( -9.049782359939607446, 124.0675141969884692, -0.1808361888366264991 ) ) ;
#13749 = EDGE_LOOP ( 'NONE', ( #40805, #14918, #27352, #866 ) ) ;
#13750 = CARTESIAN_POINT ( 'NONE',  ( -9.495519422240835894, 121.2752502669211339, -1.536911970732435462 ) ) ;
#13751 = CARTESIAN_POINT ( 'NONE',  ( 1.959965285483297404, -15.65532139403495648, 5.519319896091174904 ) ) ;
#13752 = CARTESIAN_POINT ( 'NONE',  ( -4.559029627764906500, 31.49133049583777932, -0.6947656260690758812 ) ) ;
#13753 = CARTESIAN_POINT ( 'NONE',  ( -4.584608287924823777, 117.9735455925265768, -0.9262146779261964946 ) ) ;
#13754 = CARTESIAN_POINT ( 'NONE',  ( -56.80697847991661575, 4.636179106009441497, -2.484889565616585472 ) ) ;
#13755 = CARTESIAN_POINT ( 'NONE',  ( 4.065926199369043204, 118.2429491485453354, 0.3080910687088499467 ) ) ;
#13756 = CARTESIAN_POINT ( 'NONE',  ( 5.042934966769523797, 119.7208665877771665, 1.041708725922360523 ) ) ;
#13757 = CARTESIAN_POINT ( 'NONE',  ( 14.73199999999999932, 57.78500000000000369, 0.000000000000000000 ) ) ;
#13758 = CARTESIAN_POINT ( 'NONE',  ( 18.63504953328963154, 154.1157618415863624, 0.3723726386282266709 ) ) ;
#13759 = CARTESIAN_POINT ( 'NONE',  ( 4.559522851259544041, 6.111780172613243245, 7.100340242056582873 ) ) ;
#13760 = CARTESIAN_POINT ( 'NONE',  ( 4.509850150708832217, 121.0527503406816123, 0.3565835012282698169 ) ) ;
#13761 = CARTESIAN_POINT ( 'NONE',  ( 3.898136962790617943, 117.1932757116604762, -0.4670938640342005010 ) ) ;
#13762 = CARTESIAN_POINT ( 'NONE',  ( -6.501940248589056060E-14, 66.13346620154574396, -9.529289869050788486E-18 ) ) ;
#13763 = EDGE_LOOP ( 'NONE', ( #18117, #30983, #22892, #16904 ) ) ;
#13764 = CARTESIAN_POINT ( 'NONE',  ( 1.378659152591106274, 115.6909491485452719, 1.738311037673413662 ) ) ;
#13765 = PRODUCT_DEFINITION_CONTEXT ( 'detailed design', #33067, 'design' ) ;
#13766 = CARTESIAN_POINT ( 'NONE',  ( -23.11138188961087891, 149.8995197111492814, -0.3848215369211049897 ) ) ;
#13767 = ORIENTED_EDGE ( 'NONE', *, *, #41740, .T. ) ;
#13768 = CARTESIAN_POINT ( 'NONE',  ( -8.019101373013308276, 121.3809242941630373, -1.222737436254428545 ) ) ;
#13769 = CARTESIAN_POINT ( 'NONE',  ( -46.96231544241639710, 24.98353995950039419, -1.991484372665529579 ) ) ;
#13770 = ORIENTED_EDGE ( 'NONE', *, *, #38572, .F. ) ;
#13771 = CARTESIAN_POINT ( 'NONE',  ( -11.96402413561931155, 151.9649008058812569, -0.7942868072307402993 ) ) ;
#13772 = CARTESIAN_POINT ( 'NONE',  ( 2.933303798676236696, -14.66982100897798524, 5.370674165220748364 ) ) ;
#13773 = CARTESIAN_POINT ( 'NONE',  ( -22.10195095183553349, 148.8299554149626260, 1.146864445019731393 ) ) ;
#13774 = DIRECTION ( 'NONE',  ( -4.017660918040594346E-17, 1.000000000000000000, 2.376309959284834438E-19 ) ) ;
#13775 = CARTESIAN_POINT ( 'NONE',  ( 20.46883641438825308, 129.0748834149669904, 0.4693348210411831811 ) ) ;
#13776 = ORIENTED_EDGE ( 'NONE', *, *, #21226, .F. ) ;
#13777 = CARTESIAN_POINT ( 'NONE',  ( -1.214995109038484067, 0.9429784454696930052, -4.460028654918597901 ) ) ;
#13778 = CARTESIAN_POINT ( 'NONE',  ( -22.83540780336928577, 150.4058779721138421, -0.4563057931615319140 ) ) ;
#13779 = CARTESIAN_POINT ( 'NONE',  ( -41.34500286397576474, 23.15616463071227571, -1.524000640040308330 ) ) ;
#13780 = AXIS2_PLACEMENT_3D ( 'NONE', #17981, #30978, #24576 ) ;
#13781 = LINE ( 'NONE', #24192, #16967 ) ;
#13782 = CARTESIAN_POINT ( 'NONE',  ( -5.034331710563058948, 119.1737376751357118, 0.9019231717209493793 ) ) ;
#13783 = CARTESIAN_POINT ( 'NONE',  ( -2.900346660479264482, -2.445871450894649968, -3.618988008572288972 ) ) ;
#13784 = CARTESIAN_POINT ( 'NONE',  ( 20.95410280040430351, 151.1643092826112138, 1.845047842948928762 ) ) ;
#13785 = CARTESIAN_POINT ( 'NONE',  ( -58.50248613192575675, -0.02569321026361925941, -0.6864972099078561207 ) ) ;
#13787 = CARTESIAN_POINT ( 'NONE',  ( 18.13891979603522486, 131.7244750738095149, -1.506900917850658050 ) ) ;
#13786 = CARTESIAN_POINT ( 'NONE',  ( -17.09698261757901960, 84.43312239790384410, 1.269999999999996243 ) ) ;
#13788 = CARTESIAN_POINT ( 'NONE',  ( -3.339653329301207840, -2.245917679271888900, -3.199182135983138053 ) ) ;
#13789 = CARTESIAN_POINT ( 'NONE',  ( -12.90531570856127175, 156.9034992427187376, -1.273604633583561796 ) ) ;
#13790 = VERTEX_POINT ( 'NONE', #1094 ) ;
#13791 = CARTESIAN_POINT ( 'NONE',  ( -7.620757776630488145, 122.3831840716419066, 0.1218999176909029841 ) ) ;
#13792 = CARTESIAN_POINT ( 'NONE',  ( 3.639791848495840476, -15.36872039720094207, 5.326864320309495859 ) ) ;
#13793 = FACE_OUTER_BOUND ( 'NONE', #27294, .T. ) ;
#13794 = AXIS2_PLACEMENT_3D ( 'NONE', #9227, #5411, #19003 ) ;
#13795 = FACE_OUTER_BOUND ( 'NONE', #11295, .T. ) ;
#13796 = ORIENTED_EDGE ( 'NONE', *, *, #18928, .F. ) ;
#13797 = CARTESIAN_POINT ( 'NONE',  ( 6.251746415250003963, 157.3995435888475072, 1.956906209352898829 ) ) ;
#13798 = DIRECTION ( 'NONE',  ( -4.017660918040594346E-17, 1.000000000000000000, 2.376309959284834438E-19 ) ) ;
#13799 = LINE ( 'NONE', #40017, #12342 ) ;
#13800 = AXIS2_PLACEMENT_3D ( 'NONE', #16096, #6329, #3136 ) ;
#13801 = CARTESIAN_POINT ( 'NONE',  ( -1.353295744334297224, 159.4649289425152858, 0.7236632733165272446 ) ) ;
#13802 = CARTESIAN_POINT ( 'NONE',  ( 0.09500447679424951775, 1.427469433126556053, 8.421719372511704549 ) ) ;
#13803 = CARTESIAN_POINT ( 'NONE',  ( -0.01887828017123771920, 156.5412816204240301, 0.9447463363288814975 ) ) ;
#13804 = CARTESIAN_POINT ( 'NONE',  ( -19.15923810799328209, 79.68098548105338352, 1.269999999999995799 ) ) ;
#13805 = CIRCLE ( 'NONE', #24683, 0.2540000000000062208 ) ;
#13806 = CARTESIAN_POINT ( 'NONE',  ( 6.917230302148959176, 117.3903047926647787, -0.3126493885886559854 ) ) ;
#13807 = DIRECTION ( 'NONE',  ( 0.9998004120163608288, 5.205824365704082573E-17, 0.01997839162482763914 ) ) ;
#13808 = CARTESIAN_POINT ( 'NONE',  ( -57.03986430441516831, 2.569584422222054076, 1.777618630297834734 ) ) ;
#13809 = CARTESIAN_POINT ( 'NONE',  ( -47.99025707952957021, 21.67807857130912907, 3.596429695783027292 ) ) ;
#13810 = CARTESIAN_POINT ( 'NONE',  ( 3.496333745419838657, 108.2590522130000323, -4.019922511746928606 ) ) ;
#13811 = CARTESIAN_POINT ( 'NONE',  ( -52.26939619200407350, 13.58078015197115818, 4.476849201000069556 ) ) ;
#13812 = CARTESIAN_POINT ( 'NONE',  ( -58.62105023224247446, -0.2745841218223041280, 0.4015347698698587542 ) ) ;
#13813 = CARTESIAN_POINT ( 'NONE',  ( -4.464873506718732621, 118.1580953083285692, 0.4253042567280939101 ) ) ;
#13814 = ORIENTED_EDGE ( 'NONE', *, *, #31398, .F. ) ;
#13815 = CARTESIAN_POINT ( 'NONE',  ( -46.81005371095109524, 25.73327194510133253, 1.583310528698471664 ) ) ;
#13816 = CARTESIAN_POINT ( 'NONE',  ( 6.137199031469663169, 119.5145805505420924, -1.013644267285056966 ) ) ;
#13817 = CARTESIAN_POINT ( 'NONE',  ( -6.530233653229074342, 120.6338824379019172, -0.3959831657380195047 ) ) ;
#13818 = VECTOR ( 'NONE', #39390, 1000.000000000000114 ) ;
#13819 = CARTESIAN_POINT ( 'NONE',  ( 4.599842283008522159, 118.0596567094243596, 0.7232788779925730660 ) ) ;
#13820 = CARTESIAN_POINT ( 'NONE',  ( -16.01418025823793911, 147.7157881801689427, -1.429122529412921061 ) ) ;
#13821 = AXIS2_PLACEMENT_3D ( 'NONE', #16598, #33020, #3003 ) ;
#13822 = CARTESIAN_POINT ( 'NONE',  ( -1.665825627024804634, 115.7029491485453434, -1.727339162086583890 ) ) ;
#13823 = CARTESIAN_POINT ( 'NONE',  ( 2.753590479458230433, 118.1651001943547925, -0.7052533925992238162 ) ) ;
#13824 = CARTESIAN_POINT ( 'NONE',  ( 0.8832484628481780398, 105.9424719104300436, -5.282093952356136768 ) ) ;
#13825 = CARTESIAN_POINT ( 'NONE',  ( -13.16414530391302584, 152.2904283036577908, -1.902647459344306347 ) ) ;
#13826 = CARTESIAN_POINT ( 'NONE',  ( -5.332935397695335311, 104.6144662015457385, -0.1065647409268299373 ) ) ;
#13827 = CARTESIAN_POINT ( 'NONE',  ( -3.525175246668108109, 31.21832863748435472, -0.5828980424257260706 ) ) ;
#13828 = CARTESIAN_POINT ( 'NONE',  ( 8.511289907599318028, 119.1972314554220276, -1.000383355283308129 ) ) ;
#13829 = CARTESIAN_POINT ( 'NONE',  ( -7.997804479448351600, 122.8474177855006246, -0.03617150109717347239 ) ) ;
#13830 = CARTESIAN_POINT ( 'NONE',  ( -3.909619041219700719, 60.89059347946586342, 1.524000000000007349 ) ) ;
#13831 = CARTESIAN_POINT ( 'NONE',  ( 0.3303419930533891824, 116.8490449975401617, 0.2909865916005164310 ) ) ;
#13832 = CARTESIAN_POINT ( 'NONE',  ( 5.664977208693799504, 88.73331249999999670, -5.033228321271210781 ) ) ;
#13833 = CARTESIAN_POINT ( 'NONE',  ( 1.824651611884654967, -15.33505462125983598, 5.392305443003406751 ) ) ;
#13834 = CARTESIAN_POINT ( 'NONE',  ( -19.30447918735904622, 147.3692480224366079, 1.738561774106543778 ) ) ;
#13835 = CARTESIAN_POINT ( 'NONE',  ( -0.2718671964776636085, -13.46374167387040366, -0.9358251418597670623 ) ) ;
#13836 = CARTESIAN_POINT ( 'NONE',  ( -23.06197264524096724, 149.2510847660714148, -1.189562549516614443 ) ) ;
#13837 = AXIS2_PLACEMENT_3D ( 'NONE', #26381, #30000, #35979 ) ;
#13838 = CARTESIAN_POINT ( 'NONE',  ( 0.9522911014763013604, -10.27702741150894994, -0.2247348558088197723 ) ) ;
#13839 = ORIENTED_EDGE ( 'NONE', *, *, #9963, .F. ) ;
#13840 = CARTESIAN_POINT ( 'NONE',  ( -47.14728576169839869, 19.79714445405676670, 4.666695388795770505 ) ) ;
#13841 = CARTESIAN_POINT ( 'NONE',  ( 5.292905998138358825, 116.9650601603920279, 0.9543338394691548432 ) ) ;
#13842 = CARTESIAN_POINT ( 'NONE',  ( -0.6112472438487006610, 120.6441756478195089, 0.2446543754660638059 ) ) ;
#13843 = CARTESIAN_POINT ( 'NONE',  ( 3.798736437616232919, -14.27876630094554500, 4.860596070177301442 ) ) ;
#13844 = CARTESIAN_POINT ( 'NONE',  ( 7.347594966877624145, 120.9764928074160082, -0.8683198564056585633 ) ) ;
#13845 = CARTESIAN_POINT ( 'NONE',  ( -8.661198069469564942, 120.2102557752085232, -1.489220423754913369 ) ) ;
#13846 = CARTESIAN_POINT ( 'NONE',  ( 4.531670475907399798, 115.7029491485453434, 1.515581646943963356 ) ) ;
#13847 = CARTESIAN_POINT ( 'NONE',  ( 2.967701212693483193, -13.54563334627871463, 1.070011838909553425 ) ) ;
#13848 = CARTESIAN_POINT ( 'NONE',  ( -4.948335771857875542, 117.4718462369176137, -1.024210282226911684 ) ) ;
#13849 = CARTESIAN_POINT ( 'NONE',  ( 7.846345427436761000, 154.6110463214094182, -0.1182179892959121792 ) ) ;
#13850 = EDGE_LOOP ( 'NONE', ( #15224, #29274, #36132, #19906 ) ) ;
#13851 = CARTESIAN_POINT ( 'NONE',  ( -3.892802331515536007, 109.0594729580251254, 3.652645560113729761 ) ) ;
#13852 = CARTESIAN_POINT ( 'NONE',  ( 3.936408729728400058, 109.5187069194626872, 3.609317897251677287 ) ) ;
#13853 = CIRCLE ( 'NONE', #32936, 0.2539999999999992819 ) ;
#13854 = CARTESIAN_POINT ( 'NONE',  ( -13.70496720263922619, 119.6480011847203002, -0.2738578607179661395 ) ) ;
#13855 = ADVANCED_FACE ( 'NONE', ( #40074, #31505 ), #9151, .F. ) ;
#13856 = CARTESIAN_POINT ( 'NONE',  ( -12.21488373879589240, 55.24499999999999034, 5.016499999999999737 ) ) ;
#13857 = CARTESIAN_POINT ( 'NONE',  ( 5.742584425896265721, 159.1207877133979309, 0.01316620519284362155 ) ) ;
#13858 =( BOUNDED_SURFACE ( )  B_SPLINE_SURFACE ( 3, 2, ( 
 ( #23064, #6911, #13506 ),
 ( #15684, #25285, #26066 ),
 ( #10305, #7129, #20085 ),
 ( #9107, #3939, #739 ),
 ( #38076, #34883, #5715 ),
 ( #38288, #22071, #35098 ),
 ( #4362, #20289, #7958 ),
 ( #950, #23485, #36933 ),
 ( #14122, #4781, #39714 ),
 ( #17730, #7541, #13919 ),
 ( #27335, #27121, #40554 ),
 ( #10928, #7753, #33949 ) ),
 .UNSPECIFIED., .F., .F., .F. ) 
 B_SPLINE_SURFACE_WITH_KNOTS ( ( 4, 2, 2, 2, 2, 4 ),
 ( 3, 3 ),
 ( -1.734723475976807094E-18, 0.0003677900075225834682, 0.0007355800150451686711, 0.001103370022567753874, 0.001287265026329046476, 0.001471160030090339077 ),
 ( 0.000000000000000000, 1.000000000000000000 ),
 .UNSPECIFIED. ) 
 GEOMETRIC_REPRESENTATION_ITEM ( )  RATIONAL_B_SPLINE_SURFACE ( (
 ( 1.000000000000000000, 0.7071067811865475727, 1.000000000000000000),
 ( 1.000000000000000000, 0.7071067811865475727, 1.000000000000000000),
 ( 1.000000000000000000, 0.7071067811865514585, 1.000000000000000000),
 ( 1.000000000000000000, 0.7071067811865514585, 1.000000000000000000),
 ( 1.000000000000000000, 0.7071067811865436870, 1.000000000000000000),
 ( 1.000000000000000000, 0.7071067811865436870, 1.000000000000000000),
 ( 1.000000000000000000, 0.7071067811865514585, 1.000000000000000000),
 ( 1.000000000000000000, 0.7071067811865514585, 1.000000000000000000),
 ( 1.000000000000000000, 0.7071067811865514585, 1.000000000000000000),
 ( 1.000000000000000000, 0.7071067811865514585, 1.000000000000000000),
 ( 1.000000000000000000, 0.7071067811865475727, 1.000000000000000000),
 ( 1.000000000000000000, 0.7071067811865475727, 1.000000000000000000) ) ) 
 REPRESENTATION_ITEM ( '' )  SURFACE ( )  );
#13859 = DIRECTION ( 'NONE',  ( -0.9998004120163609398, 0.000000000000000000, -0.01997839162482749689 ) ) ;
#13860 = AXIS2_PLACEMENT_3D ( 'NONE', #7483, #17670, #8306 ) ;
#13861 = CARTESIAN_POINT ( 'NONE',  ( 1.692908751855406679, -15.45794499411305623, 5.831830892034441050 ) ) ;
#13862 = CARTESIAN_POINT ( 'NONE',  ( 11.62920297224753874, 55.59919541885984273, 5.016499999999892268 ) ) ;
#13863 = CARTESIAN_POINT ( 'NONE',  ( -6.580517660824093636E-14, 85.69146620154573668, -4.881702850681514412E-18 ) ) ;
#13864 = EDGE_CURVE ( 'NONE', #18999, #24610, #15669, .T. ) ;
#13865 = CARTESIAN_POINT ( 'NONE',  ( 19.97852701226055316, 149.8444905389382882, 2.417717604095676265 ) ) ;
#13866 = EDGE_LOOP ( 'NONE', ( #9461, #38640, #5442, #20723 ) ) ;
#13867 = CARTESIAN_POINT ( 'NONE',  ( -8.379105243356219646, 21.88232641057985361, -0.8402904295462267914 ) ) ;
#13868 = CARTESIAN_POINT ( 'NONE',  ( 5.545307748665752712, 117.8092076766180867, -0.8261742690153465185 ) ) ;
#13869 = CARTESIAN_POINT ( 'NONE',  ( -1.726955742647845460, 108.8931014686503289, -4.100893600158903141 ) ) ;
#13870 = AXIS2_PLACEMENT_3D ( 'NONE', #16683, #6482, #26705 ) ;
#13871 = CARTESIAN_POINT ( 'NONE',  ( -5.525651935317164920, 78.91763798174274314, 5.107334513333068315 ) ) ;
#13872 = DIRECTION ( 'NONE',  ( 0.8745520943968249084, -0.4849315768086533418, 5.271987356194193006E-16 ) ) ;
#13873 = CARTESIAN_POINT ( 'NONE',  ( -5.314273266013044505, 104.6144662015457527, 0.4583182832411464291 ) ) ;
#13874 = CARTESIAN_POINT ( 'NONE',  ( 4.440276399826426967, -1.430929408009915083, -1.287880193523989636 ) ) ;
#13875 = DIRECTION ( 'NONE',  ( -5.188838149069471174E-16, 1.699382548006136313E-16, 1.000000000000000000 ) ) ;
#13876 = CARTESIAN_POINT ( 'NONE',  ( 0.1066493941974573784, 105.7853621660184444, -5.332931186019219005 ) ) ;
#13877 = CARTESIAN_POINT ( 'NONE',  ( 2.491201389814710065, -14.86453887000410745, 4.964479704013470496 ) ) ;
#13878 = CARTESIAN_POINT ( 'NONE',  ( 3.201024870707998016, 118.2446163226072713, -0.7148959180058853669 ) ) ;
#13879 = CARTESIAN_POINT ( 'NONE',  ( -15.64055365641546835, 121.4606353739761744, 0.3859511643760805133 ) ) ;
#13880 = CARTESIAN_POINT ( 'NONE',  ( 4.828635879361813821, 117.4024293536648855, -1.010132067140149026 ) ) ;
#13881 = CARTESIAN_POINT ( 'NONE',  ( -3.682264917456322895, 69.43546620154573645, -0.07358041635423923088 ) ) ;
#13882 = ORIENTED_EDGE ( 'NONE', *, *, #13113, .F. ) ;
#13883 = LINE ( 'NONE', #29225, #29456 ) ;
#13884 = VECTOR ( 'NONE', #41118, 1000.000000000000114 ) ;
#13885 = CARTESIAN_POINT ( 'NONE',  ( 2.989574797431095554, -15.77888062423098070, 5.070590765341169259 ) ) ;
#13886 = CARTESIAN_POINT ( 'NONE',  ( -6.603547431282940749, 157.6773268839678508, 1.653176294384505640 ) ) ;
#13887 = CARTESIAN_POINT ( 'NONE',  ( -0.6053885369530382921, 31.17761759867932980, -0.7634260365338448873 ) ) ;
#13888 = EDGE_CURVE ( 'NONE', #14753, #18130, #17263, .T. ) ;
#13889 = ORIENTED_EDGE ( 'NONE', *, *, #40979, .F. ) ;
#13890 = CARTESIAN_POINT ( 'NONE',  ( -6.513165593194060347E-14, 68.92746620154572668, -8.865348866426607246E-18 ) ) ;
#13891 = CARTESIAN_POINT ( 'NONE',  ( 1.032349031751431445, 124.2655319029901335, 0.08020592950830184031 ) ) ;
#13892 = PRESENTATION_STYLE_ASSIGNMENT (( #4119 ) ) ;
#13893 = CARTESIAN_POINT ( 'NONE',  ( -15.87656987697871891, 149.2064892436030163, 1.252469198948042761 ) ) ;
#13894 = EDGE_CURVE ( 'NONE', #4862, #9633, #12341, .T. ) ;
#13895 = CARTESIAN_POINT ( 'NONE',  ( 18.67487979129049336, 147.7499600834086948, -1.698815563122507699 ) ) ;
#13896 = CARTESIAN_POINT ( 'NONE',  ( -20.40332572169753433, 149.1468970683199586, -2.432323357318188606 ) ) ;
#13897 = DIRECTION ( 'NONE',  ( 0.6294287539884068083, 0.7770581983690809658, 1.945484789722802745E-16 ) ) ;
#13898 = EDGE_CURVE ( 'NONE', #41432, #22599, #31935, .T. ) ;
#13899 = ORIENTED_EDGE ( 'NONE', *, *, #26607, .T. ) ;
#13900 = CARTESIAN_POINT ( 'NONE',  ( 4.415132207561733857, 118.1795667174292532, -0.3921168564559623371 ) ) ;
#13901 = CARTESIAN_POINT ( 'NONE',  ( 15.74292597311039898, 147.5983985311728759, -0.4089823612135939368 ) ) ;
#13902 = ORIENTED_EDGE ( 'NONE', *, *, #21380, .F. ) ;
#13903 = CARTESIAN_POINT ( 'NONE',  ( 2.709380901426776678, -15.26748983718428931, 4.527680251005613776 ) ) ;
#13904 = CARTESIAN_POINT ( 'NONE',  ( 10.28897677580358128, 56.51500000000000057, -5.016500000000001513 ) ) ;
#13905 = CARTESIAN_POINT ( 'NONE',  ( -52.79140191244064084, 11.19429870258845128, 3.959798436812983713 ) ) ;
#13906 = CARTESIAN_POINT ( 'NONE',  ( -4.324967070706027705, -0.5217348546298695711, 1.653223044864502222 ) ) ;
#13907 = CARTESIAN_POINT ( 'NONE',  ( 15.02674521555423581, 134.7883251604851580, 1.951091898071899200 ) ) ;
#13908 = CARTESIAN_POINT ( 'NONE',  ( -2.960856320778833428, 31.17411798999470918, 0.6378382452821284021 ) ) ;
#13909 = CARTESIAN_POINT ( 'NONE',  ( 3.700881553190929374, 8.714383148187751615, -2.768892949411812854 ) ) ;
#13910 = CARTESIAN_POINT ( 'NONE',  ( 8.506011814013298533, 123.3280575159016905, 0.2025880313713111225 ) ) ;
#13911 = CARTESIAN_POINT ( 'NONE',  ( 1.734723475976807094E-15, 17.14499999999999957, 0.000000000000000000 ) ) ;
#13912 = CARTESIAN_POINT ( 'NONE',  ( -50.77948459960266092, 12.22376025917672138, -0.7375277020707465825 ) ) ;
#13913 = CARTESIAN_POINT ( 'NONE',  ( 5.560813481388145796, 116.7424064675562505, -0.1180550052279501078 ) ) ;
#13914 = CARTESIAN_POINT ( 'NONE',  ( 3.682264917456193665, 63.84746620154572838, 0.07358041635423968885 ) ) ;
#13915 = CARTESIAN_POINT ( 'NONE',  ( -12.79279280188647760, 63.69337819391066091, -1.269999999999997353 ) ) ;
#13916 = CARTESIAN_POINT ( 'NONE',  ( -29.16381924947294024, 66.91553870234344004, 1.269999999999992024 ) ) ;
#13917 = CARTESIAN_POINT ( 'NONE',  ( -3.174366308152013705, 97.37546620154573418, -0.06343139340882732180 ) ) ;
#13918 = CARTESIAN_POINT ( 'NONE',  ( 1.223683442775902463, 5.461509463947571419, 8.358860550006438572 ) ) ;
#13919 = CARTESIAN_POINT ( 'NONE',  ( -5.256643466843552659, 57.14999999999978542, 5.296410794270378197 ) ) ;
#13920 = CARTESIAN_POINT ( 'NONE',  ( -58.26284211471887176, 1.387681237079871455, 0.7239480823116738462 ) ) ;
#13921 = CARTESIAN_POINT ( 'NONE',  ( 0.4234688608138943988, 124.8375573595198063, -0.002553167718423972939 ) ) ;
#13922 = CARTESIAN_POINT ( 'NONE',  ( -21.27466159042558758, 132.4531229209162575, 0.1171209876626085472 ) ) ;
#13923 = ADVANCED_FACE ( 'NONE', ( #15525 ), #28732, .F. ) ;
#13924 = EDGE_LOOP ( 'NONE', ( #8972, #26092, #37012, #34223, #21179, #3763, #17601, #9359, #23549 ) ) ;
#13925 = CARTESIAN_POINT ( 'NONE',  ( -57.78461401849435930, 2.885363594410716992, -0.1114619696582919983 ) ) ;
#13926 = CARTESIAN_POINT ( 'NONE',  ( 6.988932177366979026, 121.9539960043768616, 0.09502985394448600076 ) ) ;
#13927 = ORIENTED_EDGE ( 'NONE', *, *, #33778, .T. ) ;
#13928 = DIRECTION ( 'NONE',  ( -0.8745520943968250194, 0.4849315768086532863, -5.361993529360574930E-16 ) ) ;
#13929 = CARTESIAN_POINT ( 'NONE',  ( -15.72575858332452015, 145.6903699455376113, -0.3657738730356400181 ) ) ;
#13930 = CARTESIAN_POINT ( 'NONE',  ( 6.002709446384779213, -13.95775275001606630, 2.224537231649871494 ) ) ;
#13931 = CARTESIAN_POINT ( 'NONE',  ( -17.75928342660610681, 128.5843929717815115, 1.279242276855531379 ) ) ;
#13932 = CARTESIAN_POINT ( 'NONE',  ( -3.562413952978887632, 23.18266144714348798, 2.948169924785601470 ) ) ;
#13933 = CARTESIAN_POINT ( 'NONE',  ( 22.49834027909111356, 137.1624432810789358, 0.8864494676080415525 ) ) ;
#13934 = CARTESIAN_POINT ( 'NONE',  ( 2.137372358784370263, -15.62272051899096859, 5.517997703402476084 ) ) ;
#13935 = CARTESIAN_POINT ( 'NONE',  ( -29.66844284761598871, 68.28155107131718182, 1.269999999999993356 ) ) ;
#13936 = CARTESIAN_POINT ( 'NONE',  ( -0.5845540250341307864, -7.254922367050685494, -0.7839501960785225654 ) ) ;
#13937 = CARTESIAN_POINT ( 'NONE',  ( -1.410028229074622219, 159.6020224343070026, -0.1582310832764448894 ) ) ;
#13938 = CARTESIAN_POINT ( 'NONE',  ( -3.174366308152013705, 104.6144662015457243, -0.06343139340882732180 ) ) ;
#13939 = CARTESIAN_POINT ( 'NONE',  ( 8.754061279740081858, 117.8557914870123682, 0.6177215411034930881 ) ) ;
#13940 = CARTESIAN_POINT ( 'NONE',  ( -0.01023306027096490718, 119.5380416804913324, 0.5121041807152045822 ) ) ;
#13941 = CARTESIAN_POINT ( 'NONE',  ( -58.08011890042329384, 0.3308434713582167341, -0.7480479229743117742 ) ) ;
#13942 = CARTESIAN_POINT ( 'NONE',  ( 9.459309661781043488, 157.4068808874136209, 1.850812122078211441 ) ) ;
#13943 = CARTESIAN_POINT ( 'NONE',  ( 19.53500017296053670, 148.0998626603252148, -1.736236475658778033 ) ) ;
#13944 = CARTESIAN_POINT ( 'NONE',  ( 0.6087277426107279288, -8.065848283227245119, 0.7602462886992925606 ) ) ;
#13945 = CARTESIAN_POINT ( 'NONE',  ( -12.26619010297312684, 120.4651188882986759, -1.462776157934944310 ) ) ;
#13946 = CARTESIAN_POINT ( 'NONE',  ( -46.31144060707497090, 24.05480373873685451, -2.308638262703932575 ) ) ;
#13947 = EDGE_CURVE ( 'NONE', #4862, #5073, #17956, .T. ) ;
#13948 = CARTESIAN_POINT ( 'NONE',  ( 4.553366535382863844, 104.6144662015457243, 1.608775678008367516 ) ) ;
#13949 = CARTESIAN_POINT ( 'NONE',  ( 0.7532517793758595204, 156.4767055779393559, -0.8130599351363748672 ) ) ;
#13950 = CARTESIAN_POINT ( 'NONE',  ( -13.59117098933512580, 150.2425924485890505, -0.2715839415562138481 ) ) ;
#13951 = VERTEX_POINT ( 'NONE', #41744 ) ;
#13952 = CARTESIAN_POINT ( 'NONE',  ( -11.26837603645374131, 123.0403929720162495, -1.648478483780370318 ) ) ;
#13953 = CARTESIAN_POINT ( 'NONE',  ( 5.315755633098069310, -15.26259334675766866, -0.1387823706055290596 ) ) ;
#13954 = LINE ( 'NONE', #16938, #2727 ) ;
#13955 = CARTESIAN_POINT ( 'NONE',  ( -4.512940082713024381, 118.0696988386537214, -0.8149125216352793855 ) ) ;
#13956 = CARTESIAN_POINT ( 'NONE',  ( -54.12303657725384198, 9.464413707472848714, -3.807237671326768602 ) ) ;
#13957 = DIRECTION ( 'NONE',  ( -5.188838149069472160E-16, 1.699382548006136559E-16, 1.000000000000000000 ) ) ;
#13958 = CARTESIAN_POINT ( 'NONE',  ( 13.99859221269040432, 128.5416456306063253, 1.961142612884885450 ) ) ;
#13959 = CARTESIAN_POINT ( 'NONE',  ( -14.60500000000000043, 71.11999999999999034, 5.016499999999999737 ) ) ;
#13960 = CARTESIAN_POINT ( 'NONE',  ( 5.757472737270592944, 159.1136035536173097, 0.1150480073142623738 ) ) ;
#13961 = CARTESIAN_POINT ( 'NONE',  ( 6.431785950458272616, 8.712657024569978148, -5.436233950049250474 ) ) ;
#13962 = CARTESIAN_POINT ( 'NONE',  ( 6.479751845157252887, 121.6679077367135591, 0.4493306481243478645 ) ) ;
#13963 = CARTESIAN_POINT ( 'NONE',  ( 15.15503192428636581, 121.4505734225448066, -0.6300967139502822167 ) ) ;
#13964 = DIRECTION ( 'NONE',  ( -1.000000000000000000, -6.353134868986659519E-16, 0.000000000000000000 ) ) ;
#13965 = CARTESIAN_POINT ( 'NONE',  ( -22.98521553460867750, 150.1595482613961110, -0.3823759483556143368 ) ) ;
#13966 = CIRCLE ( 'NONE', #13276, 0.5080000000000002292 ) ;
#13967 = ORIENTED_EDGE ( 'NONE', *, *, #18043, .F. ) ;
#13968 = CARTESIAN_POINT ( 'NONE',  ( -48.36699572807423664, 24.50126085711046997, -0.4363764532069382973 ) ) ;
#13969 = CARTESIAN_POINT ( 'NONE',  ( 6.787014259399680505, 121.1158114507673531, -0.6846564350370034635 ) ) ;
#13970 = CARTESIAN_POINT ( 'NONE',  ( -8.796322004575976905, 117.7098159678576224, 0.02677737093239071497 ) ) ;
#13971 = ORIENTED_EDGE ( 'NONE', *, *, #633, .F. ) ;
#13972 = CARTESIAN_POINT ( 'NONE',  ( -26.03112572612057818, 72.30369090346633243, 1.269999999999993578 ) ) ;
#13973 = CARTESIAN_POINT ( 'NONE',  ( -8.994301780669152535, 123.6974368934138226, -0.4925676131310582351 ) ) ;
#13974 = CARTESIAN_POINT ( 'NONE',  ( 3.467186027297813666, -14.69398785160878873, 5.340258725024584763 ) ) ;
#13975 = CARTESIAN_POINT ( 'NONE',  ( -14.35401710045877799, 121.2650221238243944, 0.8333810220845707661 ) ) ;
#13976 = DIRECTION ( 'NONE',  ( -0.9816537812491126225, -0.1906721105964872265, -8.537024980200846470E-16 ) ) ;
#13977 = CARTESIAN_POINT ( 'NONE',  ( 4.732570698819401400, 116.7698466342620378, 0.1749797587976940905 ) ) ;
#13978 = VERTEX_POINT ( 'NONE', #28099 ) ;
#13979 = CARTESIAN_POINT ( 'NONE',  ( -4.515506726787251068, -6.291224493951820484, 1.111903093310195212 ) ) ;
#13980 = CARTESIAN_POINT ( 'NONE',  ( -22.75563279970867470, 137.3797884758947703, -0.4783205966563212619 ) ) ;
#13981 = DIRECTION ( 'NONE',  ( -0.8745520943968235761, 0.4849315768086558398, -4.268512490100410909E-16 ) ) ;
#13982 = CARTESIAN_POINT ( 'NONE',  ( -19.15923810799328209, 79.68098548105338352, 1.523999999999996025 ) ) ;
#13983 = VERTEX_POINT ( 'NONE', #9352 ) ;
#13984 = CARTESIAN_POINT ( 'NONE',  ( -4.401808571117955537, 118.5828793204378115, 0.8681470107976926309 ) ) ;
#13985 = ADVANCED_FACE ( 'NONE', ( #11917 ), #12546, .T. ) ;
#13986 = CARTESIAN_POINT ( 'NONE',  ( -0.3558933743640902425, 1.202427940091101100, 4.626034787239965418 ) ) ;
#13987 = CARTESIAN_POINT ( 'NONE',  ( 21.19929070476245059, 136.5942649496780632, 1.819607900871525796 ) ) ;
#13988 = CARTESIAN_POINT ( 'NONE',  ( -57.93805369095603197, 0.6893004133203329831, -1.202053765808154040 ) ) ;
#13989 = CARTESIAN_POINT ( 'NONE',  ( 16.52101850268826055, 153.5550899668227203, -1.581448849539220269 ) ) ;
#13990 = CARTESIAN_POINT ( 'NONE',  ( 3.951836011467571907, -5.044640503713330837, -2.394960105287299523 ) ) ;
#13991 = CARTESIAN_POINT ( 'NONE',  ( -2.005144469771080740, 117.2046888992736200, -0.5340627965622030127 ) ) ;
#13992 = EDGE_CURVE ( 'NONE', #38547, #39868, #10491, .T. ) ;
#13993 = ORIENTED_EDGE ( 'NONE', *, *, #41474, .F. ) ;
#13994 = CARTESIAN_POINT ( 'NONE',  ( -9.248842176950111238, 124.1957968681474824, -0.02334546025992350476 ) ) ;
#13995 = CARTESIAN_POINT ( 'NONE',  ( 6.166227012738786151, -13.75546675568918609, 1.699147612634045235 ) ) ;
#13996 = CYLINDRICAL_SURFACE ( 'NONE', #17920, 0.5080000000000000071 ) ;
#13997 = CARTESIAN_POINT ( 'NONE',  ( -5.045173026404576433, 113.8198996840133930, -1.826729658900504649 ) ) ;
#13999 = ORIENTED_EDGE ( 'NONE', *, *, #5023, .T. ) ;
#13998 = AXIS2_PLACEMENT_3D ( 'NONE', #20155, #27190, #4007 ) ;
#14000 = CARTESIAN_POINT ( 'NONE',  ( 19.51070465195328651, 147.4874203640471535, 2.520207112597399934 ) ) ;
#14001 = FACE_OUTER_BOUND ( 'NONE', #33867, .T. ) ;
#14002 = CARTESIAN_POINT ( 'NONE',  ( 3.682264917456192332, 95.34346620154573770, 0.07358041635423968885 ) ) ;
#14003 = CARTESIAN_POINT ( 'NONE',  ( -2.024878990865745187, 117.2046888992736200, 0.4535333368958822109 ) ) ;
#14004 = CARTESIAN_POINT ( 'NONE',  ( 7.114778624005384522, 4.676967889965610858, -4.534447634950107719 ) ) ;
#14005 = CARTESIAN_POINT ( 'NONE',  ( 10.62861998609533742, 124.7671305375842934, 1.166658412819147950 ) ) ;
#14006 = CYLINDRICAL_SURFACE ( 'NONE', #26741, 13.46199999999999442 ) ;
#14007 = CARTESIAN_POINT ( 'NONE',  ( 4.817281438370265789, 117.0090399748681875, -0.3002870190743004986 ) ) ;
#14008 = CARTESIAN_POINT ( 'NONE',  ( -14.79536922792820697, 61.64024183321802042, -1.904999999999999583 ) ) ;
#14009 = CARTESIAN_POINT ( 'NONE',  ( -53.46379006321816973, 9.876576013476611848, 3.680876057010925795 ) ) ;
#14010 = CARTESIAN_POINT ( 'NONE',  ( -49.18824384045164777, 22.20099125052343680, 1.469723468883180173 ) ) ;
#14011 = CARTESIAN_POINT ( 'NONE',  ( -49.19743978460682143, 17.65503563884207594, 5.190924102448284394 ) ) ;
#14012 = CARTESIAN_POINT ( 'NONE',  ( -58.60445817883077524, -0.2419304147805778904, 0.4480943822351404759 ) ) ;
#14013 = CARTESIAN_POINT ( 'NONE',  ( -4.503997341962783452, 118.1168880179826175, 0.5560608495562332498 ) ) ;
#14014 = CARTESIAN_POINT ( 'NONE',  ( 0.3948153568139246561, 105.8845321910897042, -5.327123519515836847 ) ) ;
#14015 = B_SPLINE_SURFACE_WITH_KNOTS ( 'NONE', 5, 5, ( 
 ( #29259, #36090, #3721, #32889, #41487, #13069 ),
 ( #41275, #22842, #26488, #29684, #39070, #528 ),
 ( #25069, #18455, #35882, #6692, #317, #13284 ),
 ( #35097, #26269, #13500, #26059, #18881, #38286 ),
 ( #22070, #12294, #105, #10298, #16256, #5494 ),
 ( #2304, #31890, #2726, #39279, #19661, #38072 ),
 ( #8888, #32675, #27115, #4355, #7745, #23911 ),
 ( #23693, #30306, #29895, #33943, #732, #33311 ),
 ( #4140, #20494, #1359, #27329, #23479, #20079 ),
 ( #40547, #11134, #40130, #39919, #10921, #40341 ),
 ( #7325, #30519, #14317, #11345, #13913, #20712 ),
 ( #33523, #10713, #17316, #3933, #36927, #943 ),
 ( #17101, #36712, #33736, #7533, #36504, #20920 ),
 ( #1149, #20283, #33102, #30104, #4559, #4774 ),
 ( #13708, #26906, #14118, #17519, #36302, #24121 ),
 ( #37131, #7951, #17723, #30726, #7124, #1575 ),
 ( #14531, #27541, #16892, #26702, #39707, #10509 ),
 ( #17936, #34152, #15375, #8577, #27950, #30939 ),
 ( #14950, #11975, #5190, #1988, #2415, #15160 ),
 ( #25185, #31147, #24754, #34570, #37968, #31359 ),
 ( #14739, #40959, #24968, #41387, #11765, #4979 ),
 ( #18353, #15584, #1778, #41171, #31785, #11549 ),
 ( #27742, #37541, #18775, #40752, #21331, #37753 ),
 ( #21540, #8793, #5397, #24532, #2202, #8364 ),
 ( #34358, #21751, #34999, #38185, #18143, #28166 ),
 ( #34778, #41597, #5612, #18568, #31575, #28380 ),
 ( #12192, #28589, #9002, #21969, #5819, #2625 ),
 ( #24330, #37336, #8154, #21124, #10037, #35830 ),
 ( #6646, #12609, #41813, #22170, #32414, #38604 ),
 ( #12811, #22587, #9410, #25801, #39227, #28799 ),
 ( #9619, #29640, #32208, #35402, #3668, #15791 ),
 ( #28998, #35201, #16633, #3041, #13239, #42015 ),
 ( #23009, #265, #38807, #19200, #15999, #25596 ),
 ( #26223, #35619, #29424, #32838, #36037, #6433 ),
 ( #22795, #22376, #6852, #31993, #38401, #19407 ),
 ( #3244, #26011, #51, #6229, #16203, #29208 ),
 ( #19821, #18989, #13017, #39020, #9828, #19610 ),
 ( #3456, #32623, #9213, #2831, #12407, #25399 ),
 ( #16418, #6027, #4512, #20240, #13658, #36883 ),
 ( #17677, #33266, #14069, #4307, #894, #36669 ),
 ( #1102, #20870, #24076, #4095, #17054, #10876 ),
 ( #20034, #26438, #10666, #33477, #23647, #27073 ),
 ( #16848, #30056, #7490, #36249, #40296, #7070 ),
 ( #686, #39656, #26862, #7701, #33688, #29848 ),
 ( #33053, #4725, #17473, #17270, #13868, #30261 ),
 ( #39870, #26648, #20662, #30471, #477, #20450 ),
 ( #40081, #23864, #1315, #10460, #14272, #10245 ),
 ( #37088, #23216, #23430, #27282, #11089, #7906 ),
 ( #33894, #36459, #13450, #7278, #39442, #3883 ),
 ( #41335, #31516, #37286, #30891, #14690, #11499 ),
 ( #15106, #14898, #24485, #37490, #28109, #21285 ),
 ( #8738, #2361, #34521, #40502, #1732, #31100 ),
 ( #8105, #21489, #28327, #11925, #21914, #24917 ),
 ( #17889, #11297, #8529, #27695, #15320, #1939 ),
 ( #34944, #12138, #8313, #27900, #40908, #2147 ),
 ( #40703, #21079, #34314, #31302, #5554, #5143 ),
 ( #5768, #18097, #25130, #11713, #24700, #38132 ),
 ( #37706, #5347, #18301, #41119, #37914, #8947 ),
 ( #18511, #21699, #34723, #30678, #1526, #14482 ),
 ( #27494, #24281, #34104, #4931, #25341, #22538 ),
 ( #2782, #9362, #32152, #35774, #13186, #15536 ),
 ( #35984, #3187, #2985, #12557, #25546, #16149 ),
 ( #22956, #38549, #3399, #15947, #22325, #32566 ),
 ( #26171, #39175, #16366, #12353, #28538, #9776 ),
 ( #35350, #38344, #28944, #6178, #6383, #41756 ),
 ( #38966, #9567, #18722, #19557, #19147, #41961 ),
 ( #32359, #25749, #28743, #9162, #12760, #19353 ),
 ( #38757, #41545, #9983, #35565, #29372, #29153 ),
 ( #31732, #5973, #22742, #35148, #2575, #42161 ),
 ( #6589, #12965, #25959, #18936, #211, #22119 ),
 ( #31944, #15738, #30004, #36830, #4465, #20606 ),
 ( #20398, #36620, #23164, #36414, #844, #426 ),
 ( #13396, #3834, #7020, #16798, #33217, #14018 ),
 ( #36199, #32788, #26385, #11039, #23809, #10617 ),
 ( #23599, #10827, #26599, #19988, #1054, #27025 ),
 ( #39606, #33426, #7439, #7232, #13816, #33006 ),
 ( #16583, #29799, #4255, #7650, #23381, #29592 ),
 ( #10409, #33638, #20192, #640, #17422, #30420 ),
 ( #13609, #4044, #17005, #26815, #1267, #39823 ),
 ( #27231, #14223, #17217, #30214, #40033, #40245 ),
 ( #39392, #3618, #24022, #6799, #19767, #10194 ),
 ( #24435, #31046, #30630, #34674, #1473, #34054 ),
 ( #4883, #21234, #2094, #28058, #24229, #20818 ),
 ( #41281, #11878, #40859, #40653, #11661, #41068 ),
 ( #8057, #31253, #15058, #12087, #14639, #8481 ),
 ( #37439, #1885, #21031, #37657, #4672, #17838 ),
 ( #17629, #30836, #8262, #5299, #27640, #21437 ),
 ( #11244, #34263, #1685, #33844, #11446, #34466 ),
 ( #37863, #14430, #37239, #5092, #18045, #37039 ),
 ( #14847, #27852, #24647, #18247, #24867, #7857 ),
 ( #21649, #8687, #5503, #18462, #27438, #31467 ),
 ( #2310, #15271, #28276, #40454, #19305, #25288 ),
 ( #34889, #2935, #9110, #38920, #25500, #35304 ),
 ( #38500, #9730, #41494, #25912, #22278, #167 ),
 ( #5924, #16320, #31682, #9316, #15687, #12714 ),
 ( #6132, #19095, #22074, #32104, #22697, #12299 ),
 ( #15897, #25075, #2732, #18887, #29323, #28486 ),
 ( #22486, #38292, #35101, #2524, #28899, #38081 ),
 ( #41914, #32522, #31895, #29107, #28693, #8895 ),
 ( #21863, #16102, #41702, #25704, #12510, #38709 ),
 ( #9519, #35514, #18675, #6335, #12921, #35728 ),
 ( #32310, #3140, #42125, #6539, #19513, #3353 ),
 ( #5719, #15487, #10146, #13345, #23116, #39557 ),
 ( #4201, #379, #39130, #32740, #17376, #30164 ),
 ( #16745, #16954, #17165, #32958, #26334, #7385 ),
 ( #30366, #3785, #26765, #29953, #13561, #7186 ),
 ( #13768, #22906, #39341, #7594, #35940, #36152 ),
 ( #23547, #29750, #39774, #26551, #29544, #10362 ),
 ( #9936, #6969, #10569, #23756, #13969, #19721 ),
 ( #19940, #4418, #3573, #36778, #589, #26973 ),
 ( #6752, #20345, #793, #33369, #39984, #36568 ),
 ( #16534, #20556, #33586, #10775, #23333, #36369 ),
 ( #20145, #33168, #3996, #1005, #13137, #26128 ),
 ( #24386, #10987, #30992, #8008, #1630, #11191 ),
 ( #1832, #4830, #1420, #28006, #14585, #11823 ),
 ( #5037, #24812, #27387, #34000, #27590, #18198 ),
 ( #40192, #24177, #34623, #33794, #37807, #20979 ),
 ( #17782, #23969, #37599, #17994, #21384, #2042 ),
 ( #36988, #14377, #40599, #30581, #20770, #34209 ),
 ( #24592, #5450, #8425, #40397, #37186, #7808 ),
 ( #30781, #15007, #11399, #37391, #8209, #21181 ),
 ( #14796, #27799, #40807, #11608, #34410, #4622 ),
 ( #8632, #5243, #17577, #31199, #41015, #21594 ),
 ( #18410, #1215, #14174, #27178, #35465, #5670 ),
 ( #19045, #28223, #22435, #22026, #25457, #18627 ),
 ( #32267, #31842, #28856, #25023, #12463, #19259 ),
 ( #3097, #15434, #38454, #18838, #12032, #35258 ),
 ( #6288, #22229, #16058, #38025, #41229, #2259 ),
 ( #32050, #41869, #12668, #38869, #2682, #25657 ),
 ( #9272, #15639, #9061, #8846, #35055, #29060 ),
 ( #5875, #42080, #9681, #12873, #38244, #25862 ),
 ( #28644, #35681, #41655, #22647, #6082, #2887 ),
 ( #15221, #6490, #31417, #21810, #34836, #31632 ),
 ( #15850, #38664, #2473, #9472, #28437, #41443 ),
 ( #12248, #25241, #10312, #23706, #20296, #26284 ),
 ( #29698, #33117, #26502, #29490, #9885, #39292 ),
 ( #16906, #35895, #6705, #26075, #13513, #10726 ),
 ( #36317, #26919, #19674, #23492, #32689, #36726 ),
 ( #16270, #10521, #10098, #39506, #3523, #23281 ),
 ( #19888, #29908, #13083, #539, #7338, #17116 ),
 ( #16484, #7136, #6919, #119, #20093, #39934 ),
 ( #30117, #39083, #331, #13297, #23071, #3735 ),
 ( #36519, #36104, #3305, #22858, #19468, #33324 ),
 ( #32904, #3946, #4153, #16693, #746, #13721 ),
 ( #32475, #26715, #39723, #957, #13926, #29272 ),
 ( #8749, #17329, #20725, #2586, #30319, #4574 ),
 ( #18523, #27911, #21711, #8539, #23924, #34532 ),
 ( #33537, #33749, #5567, #18732, #8958, #14128 ),
 ( #17532, #30533, #25352, #34735, #37926, #4369 ),
 ( #40918, #2158, #36940, #11936, #21926, #21499 ) ),
 .UNSPECIFIED., .F., .F., .F.,
 ( 6, 4, 4, 4, 4, 4, 4, 4, 4, 4, 4, 4, 4, 4, 4, 4, 4, 4, 4, 4, 4, 4, 4, 4, 4, 4, 4, 4, 4, 4, 4, 4, 4, 4, 4, 4, 4, 6 ),
 ( 6, 6 ),
 ( 0.000000000000000000, 0.01562500000000000000, 0.02343750000000000000, 0.03125000000000000000, 0.04687500000000000000, 0.06250000000000000000, 0.09375000000000000000, 0.1093750000000000000, 0.1171875000000000000, 0.1250000000000000000, 0.1875000000000000000, 0.2187500000000000000, 0.2500000000000000000, 0.3125000000000000000, 0.3750000000000000000, 0.4062500000000000000, 0.4218750000000000000, 0.4375000000000000000, 0.4687500000000000000, 0.4843750000000000000, 0.4921875000000000000, 0.5000000000000000000, 0.5312500000000000000, 0.5468750000000000000, 0.5625000000000000000, 0.6250000000000000000, 0.6875000000000000000, 0.7500000000000000000, 0.8125000000000000000, 0.8437500000000000000, 0.8750000000000000000, 0.9062500000000000000, 0.9375000000000000000, 0.9531250000000000000, 0.9687500000000000000, 0.9765625000000000000, 0.9843750000000000000, 1.000000000000000000 ),
 ( 0.000000000000000000, 1.000000000000000000 ),
 .UNSPECIFIED. ) ;
#14016 = VERTEX_POINT ( 'NONE', #15311 ) ;
#14017 = CARTESIAN_POINT ( 'NONE',  ( -45.67973391888839529, 25.66060799623228661, 1.523999999999991806 ) ) ;
#14018 = CARTESIAN_POINT ( 'NONE',  ( 8.365669025111728274, 119.9184419981384906, -1.112736592547703962 ) ) ;
#14019 = CARTESIAN_POINT ( 'NONE',  ( -7.474242191267291169, 123.6620266863018855, -0.1838331482465496713 ) ) ;
#14020 = CARTESIAN_POINT ( 'NONE',  ( 4.506509836442742944, 118.1222450895864142, 0.6634770384556544220 ) ) ;
#14021 = CARTESIAN_POINT ( 'NONE',  ( -8.116318325016218083, 154.6259123219959690, -0.9857874811295549433 ) ) ;
#14022 = CARTESIAN_POINT ( 'NONE',  ( 0.03519895179119666290, 115.7029491485446613, -1.761499482103947800 ) ) ;
#14023 = CARTESIAN_POINT ( 'NONE',  ( 2.601312006192598947, 117.9496052548661282, -1.235025137275671536 ) ) ;
#14024 = AXIS2_PLACEMENT_3D ( 'NONE', #10889, #23876, #7714 ) ;
#14025 = DIRECTION ( 'NONE',  ( -4.017660918040594346E-17, 1.000000000000000000, 2.376309959284834438E-19 ) ) ;
#14026 = CARTESIAN_POINT ( 'NONE',  ( -5.138962689587368793, 120.6777149489875569, -0.7548553450424396738 ) ) ;
#14027 = CARTESIAN_POINT ( 'NONE',  ( 16.60960244842765832, -1.890517883502633324E-15, 2.034089647357696937E-15 ) ) ;
#14028 = CARTESIAN_POINT ( 'NONE',  ( -47.84756666395249880, 19.38928433903623016, 5.209054514891913179 ) ) ;
#14029 = VECTOR ( 'NONE', #25845, 1000.000000000000000 ) ;
#14030 = CARTESIAN_POINT ( 'NONE',  ( 8.709803600792051625, 118.1821829479768411, -0.5645179937760026467 ) ) ;
#14031 = CARTESIAN_POINT ( 'NONE',  ( -6.068413115653235046, 121.4395679061438500, -0.1212613406838785185 ) ) ;
#14032 = VECTOR ( 'NONE', #21279, 1000.000000000000000 ) ;
#14033 = DIRECTION ( 'NONE',  ( 5.188838149069472160E-16, -1.699382548006136559E-16, -1.000000000000000000 ) ) ;
#14034 = CARTESIAN_POINT ( 'NONE',  ( 22.80589948333479455, 149.4631731099488832, 1.425235564609340644 ) ) ;
#14035 = CARTESIAN_POINT ( 'NONE',  ( 5.871452009091292723, 88.73331249999999670, -5.016499999999999737 ) ) ;
#14036 = CARTESIAN_POINT ( 'NONE',  ( 3.040187153003802933, -14.59799761600802448, -0.3075781077882258630 ) ) ;
#14037 = CARTESIAN_POINT ( 'NONE',  ( -8.398523874639556297, 120.8878392079396065, 1.065324388190682869 ) ) ;
#14038 = CARTESIAN_POINT ( 'NONE',  ( -0.6988831915142799112, -0.7227331674307564402, 0.6786060147580050828 ) ) ;
#14039 = CARTESIAN_POINT ( 'NONE',  ( -14.89898862929395307, 156.1361208441215922, -1.045442070961571712 ) ) ;
#14040 = CARTESIAN_POINT ( 'NONE',  ( 0.1793159252905947298, -3.154364953387045034, 0.9593126492898319535 ) ) ;
#14041 = ORIENTED_EDGE ( 'NONE', *, *, #34939, .F. ) ;
#14042 = EDGE_CURVE ( 'NONE', #25936, #33599, #17189, .T. ) ;
#14043 = CARTESIAN_POINT ( 'NONE',  ( -49.65974013515536711, 15.91765330076391116, 3.790917083309703006 ) ) ;
#14044 = CARTESIAN_POINT ( 'NONE',  ( 4.746159770738230144, 112.7696648386057632, 2.567419849205245796 ) ) ;
#14045 = ITEM_DEFINED_TRANSFORMATION ( 'NONE', 'NONE', #40696,  #3275 ) ;
#14046 = CARTESIAN_POINT ( 'NONE',  ( -5.231962949222473291, 121.1607713875043117, 0.2380388119251650447 ) ) ;
#14047 = CARTESIAN_POINT ( 'NONE',  ( 4.143153066788715755, -13.73528615761443561, 4.025237717645509861 ) ) ;
#14048 = CARTESIAN_POINT ( 'NONE',  ( 13.47719143446456158, 152.3772590505219569, -1.474657383304484037 ) ) ;
#14049 = ORIENTED_EDGE ( 'NONE', *, *, #41455, .T. ) ;
#14050 = CARTESIAN_POINT ( 'NONE',  ( -17.77132669990263381, 135.5811125208551857, -2.431814553008901481 ) ) ;
#14051 = CARTESIAN_POINT ( 'NONE',  ( 4.696425917067753808, 104.6144662015457811, 1.156094417770676230 ) ) ;
#14052 = CARTESIAN_POINT ( 'NONE',  ( 2.770737963896511946, -14.84290363635286347, 4.452025088638788652 ) ) ;
#14053 = CARTESIAN_POINT ( 'NONE',  ( -4.810636611593423595, 117.4081599864878598, -1.190287313834438532 ) ) ;
#14054 = CARTESIAN_POINT ( 'NONE',  ( 6.023029630344915120, 155.3544091381320982, -0.1360875627331026294 ) ) ;
#14055 = ORIENTED_EDGE ( 'NONE', *, *, #16267, .T. ) ;
#14056 = DIRECTION ( 'NONE',  ( -9.627370216492862708E-17, -1.000000000000000000, 0.000000000000000000 ) ) ;
#14057 = CARTESIAN_POINT ( 'NONE',  ( 1.982478559079971836, 106.5598271223885973, 4.949040049329130220 ) ) ;
#14058 = DIRECTION ( 'NONE',  ( -5.206863593109713045E-17, 1.000000000000000000, -1.077750396879097359E-30 ) ) ;
#14059 = CARTESIAN_POINT ( 'NONE',  ( -5.924740142096584172, 65.21691166894066782, -1.523999999999994026 ) ) ;
#14060 = AXIS2_PLACEMENT_3D ( 'NONE', #30575, #17370, #17160 ) ;
#14061 = CARTESIAN_POINT ( 'NONE',  ( 15.55989727259145816, 120.8127473925414108, 0.08007127899889542044 ) ) ;
#14062 = CARTESIAN_POINT ( 'NONE',  ( -7.772068811996249771, 69.25462295839062676, -1.269999999999995577 ) ) ;
#14063 = CARTESIAN_POINT ( 'NONE',  ( 1.674296855365971837, -15.41063152441347839, 5.809694019739205295 ) ) ;
#14064 = CARTESIAN_POINT ( 'NONE',  ( -8.095114962461808616, 74.19100168833409725, -1.269999999999996687 ) ) ;
#14065 = CARTESIAN_POINT ( 'NONE',  ( -1.606566256928685599, 32.19982401495065716, 1.077694121983207021 ) ) ;
#14066 = CARTESIAN_POINT ( 'NONE',  ( 1.110739552455571877, 158.5855360310326319, 1.562719372149667496 ) ) ;
#14067 = EDGE_LOOP ( 'NONE', ( #19442, #5279, #40268, #24671 ) ) ;
#14068 = CARTESIAN_POINT ( 'NONE',  ( -5.777836206968382626, 13.68815862607732825, 6.147148275823971275 ) ) ;
#14069 = CARTESIAN_POINT ( 'NONE',  ( -2.234004830793105967, 117.0010803218221440, -0.5995543873723633288 ) ) ;
#14070 = CARTESIAN_POINT ( 'NONE',  ( -5.704032853997477837, 123.8402959710505087, -0.1558735912124264156 ) ) ;
#14071 = CARTESIAN_POINT ( 'NONE',  ( 4.770616296362242714, 117.4047743977180431, 1.204058524662376728 ) ) ;
#14072 = DIRECTION ( 'NONE',  ( 1.000000000000000000, 0.000000000000000000, -0.000000000000000000 ) ) ;
#14073 = CARTESIAN_POINT ( 'NONE',  ( -5.219876558649859888, 104.6144662015479554, 1.151217749705495397 ) ) ;
#14074 = TOROIDAL_SURFACE ( 'NONE', #30403, 8.794749999999998735, 0.2540000000000000036 ) ;
#14075 = CARTESIAN_POINT ( 'NONE',  ( 4.574821423538755205, -2.080616851812391310, 0.6590154617212384824 ) ) ;
#14076 = DIRECTION ( 'NONE',  ( 9.627370216492862708E-17, 1.000000000000000000, -0.000000000000000000 ) ) ;
#14077 = CARTESIAN_POINT ( 'NONE',  ( -4.968812502058939984, 56.51947257897013088, -4.801689445541318157 ) ) ;
#14078 = CARTESIAN_POINT ( 'NONE',  ( 3.402052537932679588, -13.50846463298115196, 2.481730329246660371 ) ) ;
#14079 = CARTESIAN_POINT ( 'NONE',  ( 3.788670433418564354, 121.1194860566822626, -0.2213384591549590330 ) ) ;
#14080 = CARTESIAN_POINT ( 'NONE',  ( -19.68299761936910741, 128.7577553591919752, 0.4435077540095087589 ) ) ;
#14081 = EDGE_CURVE ( 'NONE', #22433, #22644, #8459, .T. ) ;
#14082 = CARTESIAN_POINT ( 'NONE',  ( 0.6436272176209127949, 34.89395232701851768, 2.967994052886136824 ) ) ;
#14083 = CARTESIAN_POINT ( 'NONE',  ( -22.95370498042275642, 82.54569470718179502, -1.270000000000005791 ) ) ;
#14084 = CIRCLE ( 'NONE', #28381, 1.905000000000000471 ) ;
#14085 = ORIENTED_EDGE ( 'NONE', *, *, #23404, .T. ) ;
#14086 = DIRECTION ( 'NONE',  ( -0.8745520943968235761, 0.4849315768086558953, -5.361993529360570985E-16 ) ) ;
#14087 = CARTESIAN_POINT ( 'NONE',  ( 4.747814429275453385, -15.55672444834840817, 1.946379828023123482 ) ) ;
#14088 = CARTESIAN_POINT ( 'NONE',  ( -2.589082543892896826, 158.1729697732556588, 1.607049804855985808 ) ) ;
#14089 = CARTESIAN_POINT ( 'NONE',  ( 4.529186081025091681, -11.15152372915077095, -0.9203776863585164669 ) ) ;
#14090 = ADVANCED_FACE ( 'NONE', ( #11704 ), #41374, .T. ) ;
#14091 = ORIENTED_EDGE ( 'NONE', *, *, #39751, .F. ) ;
#14092 = CARTESIAN_POINT ( 'NONE',  ( 16.60960244842765121, 9.026346327358513832, 2.034089647357696543E-15 ) ) ;
#14093 = CIRCLE ( 'NONE', #35880, 0.5079999999999984528 ) ;
#14094 = CARTESIAN_POINT ( 'NONE',  ( 0.7422006451357222589, 119.7070660435176279, 0.6877902101425066306 ) ) ;
#14095 = CARTESIAN_POINT ( 'NONE',  ( -0.007600002268431407110, 120.2037396364829505, 0.3803351912374560162 ) ) ;
#14096 = CARTESIAN_POINT ( 'NONE',  ( -46.58415294817042707, 20.65776983473033823, 4.869103127773887429 ) ) ;
#14097 = CARTESIAN_POINT ( 'NONE',  ( 5.764372972839492348, 156.8407539676644546, -1.669942767410473872 ) ) ;
#14098 = CARTESIAN_POINT ( 'NONE',  ( -19.36210883413068728, 150.5708382285403388, -2.397539767985719994 ) ) ;
#14099 = CARTESIAN_POINT ( 'NONE',  ( -19.33375693323417366, 80.42273151551299293, 1.269999999999995577 ) ) ;
#14100 = CARTESIAN_POINT ( 'NONE',  ( 4.317686572074536322, 118.2120815337069502, -0.3237342310324874961 ) ) ;
#14101 = EDGE_CURVE ( 'NONE', #17420, #18200, #26677, .T. ) ;
#14102 = CARTESIAN_POINT ( 'NONE',  ( 0.009747742627749139341, 156.3581291470199233, -0.4878169013068171522 ) ) ;
#14103 = ORIENTED_EDGE ( 'NONE', *, *, #22477, .T. ) ;
#14104 = CARTESIAN_POINT ( 'NONE',  ( 3.275654002680270960, -14.73162568742410272, 0.7099577593494145189 ) ) ;
#14105 = CARTESIAN_POINT ( 'NONE',  ( -5.007446857918051109, 117.4001727933947450, 0.7824604973016788811 ) ) ;
#14106 = CARTESIAN_POINT ( 'NONE',  ( -58.14608079600216684, 0.1881903270890411539, 0.6509722733310221443 ) ) ;
#14107 = CARTESIAN_POINT ( 'NONE',  ( -2.651420880294951488, 7.049774601622781134, -3.792306073587544901 ) ) ;
#14109 = ADVANCED_FACE ( 'NONE', ( #13174 ), #23385, .F. ) ;
#14108 = CARTESIAN_POINT ( 'NONE',  ( 7.970993357304747562, 121.6949282028273132, 1.099362369368162007 ) ) ;
#14110 = CARTESIAN_POINT ( 'NONE',  ( 2.324208648641447272, 36.38269483203109189, 0.7534968369120438325 ) ) ;
#14111 = CARTESIAN_POINT ( 'NONE',  ( -3.253275476659364784, 108.9521120498200730, 3.903703133364782030 ) ) ;
#14112 = CARTESIAN_POINT ( 'NONE',  ( -4.374560056058969693, 13.03735028915297534, 1.504755201125916875 ) ) ;
#14113 = CARTESIAN_POINT ( 'NONE',  ( 10.40089755570032359, 153.1126597504080280, 0.2539288847195829701 ) ) ;
#14114 = CARTESIAN_POINT ( 'NONE',  ( -0.6577828486943301245, 105.8200195939415238, 5.299418820073016789 ) ) ;
#14115 = EDGE_CURVE ( 'NONE', #6407, #24827, #16582, .T. ) ;
#14116 = VECTOR ( 'NONE', #30071, 1000.000000000000114 ) ;
#14117 = CARTESIAN_POINT ( 'NONE',  ( -54.22787649382025421, 6.886497292746610377, -9.681224659302749425E-15 ) ) ;
#14118 = CARTESIAN_POINT ( 'NONE',  ( -2.159211318501875976, 116.3154634562797156, -0.2664370011832097873 ) ) ;
#14119 = CARTESIAN_POINT ( 'NONE',  ( -29.30569680504977370, 61.36914094216600546, -1.270000000000005347 ) ) ;
#14120 = CARTESIAN_POINT ( 'NONE',  ( -5.377075248297400911, 4.191758615746518757, 6.528609652590111168 ) ) ;
#14121 = EDGE_CURVE ( 'NONE', #10570, #27965, #34307, .T. ) ;
#14122 = CARTESIAN_POINT ( 'NONE',  ( -4.918180946948480070, 56.51500000000000767, 4.748993904427170065 ) ) ;
#14123 = CARTESIAN_POINT ( 'NONE',  ( -58.33482727260577860, 1.278009831242016281, 0.06942977984275174042 ) ) ;
#14124 = CARTESIAN_POINT ( 'NONE',  ( 0.4165637647020300482, 124.3520329708341023, -0.05485040398408827511 ) ) ;
#14125 = CARTESIAN_POINT ( 'NONE',  ( -20.20614143541417107, 128.9119615565081176, -0.01722291150864733306 ) ) ;
#14126 = ORIENTED_EDGE ( 'NONE', *, *, #32350, .F. ) ;
#14127 = CARTESIAN_POINT ( 'NONE',  ( -56.90576330281450623, 4.524090327013369439, -2.207515467630546180 ) ) ;
#14128 = CARTESIAN_POINT ( 'NONE',  ( 7.786259072927051328, 122.6240336679672964, 0.1181640080994604408 ) ) ;
#14129 = VERTEX_POINT ( 'NONE', #26162 ) ;
#14130 = CARTESIAN_POINT ( 'NONE',  ( -47.85244527695899563, 19.39403540832956807, -5.219971639306755229 ) ) ;
#14131 = CARTESIAN_POINT ( 'NONE',  ( -5.300740673260492031, 121.3529869156830046, -0.1337733589788158428 ) ) ;
#14132 = CARTESIAN_POINT ( 'NONE',  ( 4.211475536325941071, -15.04083557003654903, 4.983330352733777779 ) ) ;
#14133 = CARTESIAN_POINT ( 'NONE',  ( -21.33845497820667347, 148.5140355411650717, 1.460612514688959473 ) ) ;
#14134 = CARTESIAN_POINT ( 'NONE',  ( 2.814065556059444528, 116.6946238705719594, 0.3036003272628904348 ) ) ;
#14135 = CARTESIAN_POINT ( 'NONE',  ( 1.552363575376712435, 156.2629490296457107, 0.1466332841606040882 ) ) ;
#14136 = CARTESIAN_POINT ( 'NONE',  ( -0.3239230800893593276, 29.42979164457532804, -4.628216972995994993 ) ) ;
#14137 = CARTESIAN_POINT ( 'NONE',  ( -0.6378939814135665687, 2.446253604616882349, -0.7403349100440516084 ) ) ;
#14138 = CARTESIAN_POINT ( 'NONE',  ( -23.16647984970260765, 149.6103952014060212, -0.7935852015942146398 ) ) ;
#14139 = CARTESIAN_POINT ( 'NONE',  ( -4.645572480595541620, 117.9340260526530813, 0.7769932229682322555 ) ) ;
#14140 = FACE_OUTER_BOUND ( 'NONE', #20678, .T. ) ;
#14141 = ORIENTED_EDGE ( 'NONE', *, *, #12821, .F. ) ;
#14142 = CARTESIAN_POINT ( 'NONE',  ( -2.222944194728036393, 116.2580020178152438, 0.07250321285308233832 ) ) ;
#14143 = CARTESIAN_POINT ( 'NONE',  ( -2.489404145489931608, 119.6096776070104681, 0.6201668936895532447 ) ) ;
#14144 = CARTESIAN_POINT ( 'NONE',  ( -58.30215177840349128, -0.1486083857870257596, -0.3315235503724106580 ) ) ;
#14145 = CARTESIAN_POINT ( 'NONE',  ( 19.37548274631721057, 145.1342744731992127, -1.755133555010167434 ) ) ;
#14146 = CARTESIAN_POINT ( 'NONE',  ( 0.7725963012898818816, -15.30024676335969325, -0.5870848125168374176 ) ) ;
#14147 = CARTESIAN_POINT ( 'NONE',  ( -13.21493909911912823, 121.0513591912305316, -1.522979426720440843 ) ) ;
#14148 = CARTESIAN_POINT ( 'NONE',  ( -47.20791569504334717, 21.28685671521062517, -4.803936552638846891 ) ) ;
#14149 = CARTESIAN_POINT ( 'NONE',  ( 4.504358764033148610, 104.6144662015500444, 2.878036670428496091 ) ) ;
#14150 = CARTESIAN_POINT ( 'NONE',  ( 3.575420174883959135, 120.5283240077024800, -0.4162329711438421675 ) ) ;
#14151 = CARTESIAN_POINT ( 'NONE',  ( -5.959810334499720419, 155.3892724211786742, -0.1190911940436165245 ) ) ;
#14152 = ORIENTED_EDGE ( 'NONE', *, *, #17533, .F. ) ;
#14153 = CARTESIAN_POINT ( 'NONE',  ( -18.35242356974476863, 147.0160646422468744, -2.398428600884452866 ) ) ;
#14154 = CARTESIAN_POINT ( 'NONE',  ( 3.166528004143551289, -15.72052770450255110, 4.635360722337766859 ) ) ;
#14155 = CARTESIAN_POINT ( 'NONE',  ( -5.078986093043186933, 100.6774662015457409, -0.1014902294541231709 ) ) ;
#14156 = CARTESIAN_POINT ( 'NONE',  ( -4.481907290720103632, 118.1292030818244996, -0.6917001881693495280 ) ) ;
#14157 = CARTESIAN_POINT ( 'NONE',  ( -50.78166962549567387, 16.07998339508975860, -4.893817234114181680 ) ) ;
#14158 = EDGE_CURVE ( 'NONE', #41143, #27874, #39765, .T. ) ;
#14159 = CARTESIAN_POINT ( 'NONE',  ( -4.897655256226337350, 56.53910281269283900, -5.081330806033717451 ) ) ;
#14160 = CARTESIAN_POINT ( 'NONE',  ( 17.63007963961410240, 148.6960320134204210, 2.325091492104032653 ) ) ;
#14161 = CARTESIAN_POINT ( 'NONE',  ( 0.02537255736346701387, 39.20946620154573736, -1.269746523260778970 ) ) ;
#14162 = CARTESIAN_POINT ( 'NONE',  ( 14.90010799439742861, 120.3262451489332818, 0.2810636626631670132 ) ) ;
#14163 = CARTESIAN_POINT ( 'NONE',  ( -8.420209349088564110, 12.38497237326411415, -0.2929423126682718648 ) ) ;
#14164 = CARTESIAN_POINT ( 'NONE',  ( 11.96402413561918188, 151.9649008058812569, 0.7942868072307405214 ) ) ;
#14165 = CARTESIAN_POINT ( 'NONE',  ( 5.484805557156704481, 159.0107326448372191, -0.7391455978106865610 ) ) ;
#14166 = ADVANCED_FACE ( 'NONE', ( #12751 ), #22943, .F. ) ;
#14167 = DIRECTION ( 'NONE',  ( 0.7770581983690878491, -0.6294287539883980376, 5.101669463485847584E-16 ) ) ;
#14168 = CARTESIAN_POINT ( 'NONE',  ( 5.586884702347365561, 72.99146620154573384, 0.1116392523995368286 ) ) ;
#14169 = EDGE_CURVE ( 'NONE', #3481, #2591, #6561, .T. ) ;
#14170 = CARTESIAN_POINT ( 'NONE',  ( -57.34787435976329562, 1.552391619547732748, 0.09937746155959813199 ) ) ;
#14171 = CARTESIAN_POINT ( 'NONE',  ( -1.419391870195790162, 159.6052071245950970, 0.01540741456718481076 ) ) ;
#14172 = VERTEX_POINT ( 'NONE', #38746 ) ;
#14173 = CARTESIAN_POINT ( 'NONE',  ( -47.63491852694408379, 24.04202919463459409, -1.290898778641178080 ) ) ;
#14174 = CARTESIAN_POINT ( 'NONE',  ( -5.935837797515413072, 121.3959224772089129, -0.2928876704554002619 ) ) ;
#14175 = CARTESIAN_POINT ( 'NONE',  ( -8.663704466952724559, 118.4235366968212730, 0.7034480781449566900 ) ) ;
#14176 = VERTEX_POINT ( 'NONE', #32777 ) ;
#14177 = CARTESIAN_POINT ( 'NONE',  ( -17.14500000000466784, 71.11999999999886768, 1.269999999999998241 ) ) ;
#14178 = CARTESIAN_POINT ( 'NONE',  ( -5.248704524870183796, 121.2670714900434206, -0.3264022214948025247 ) ) ;
#14179 = CARTESIAN_POINT ( 'NONE',  ( 4.980517673276738222, -11.70649569897110709, 0.6972323075040541829 ) ) ;
#14180 = AXIS2_PLACEMENT_3D ( 'NONE', #27284, #36251, #26440 ) ;
#14181 = CARTESIAN_POINT ( 'NONE',  ( -1.320630737124576903, 159.3505072347868747, 0.9467419726141096392 ) ) ;
#14182 = CARTESIAN_POINT ( 'NONE',  ( -5.652760403059880367, 78.90762248850967353, -4.881857480398479332 ) ) ;
#14183 = CARTESIAN_POINT ( 'NONE',  ( 13.42863190281024011, 156.9273374874128137, 0.3327859972200289396 ) ) ;
#14184 = ORIENTED_EDGE ( 'NONE', *, *, #8919, .T. ) ;
#14185 = CARTESIAN_POINT ( 'NONE',  ( 0.6989348986720191892, -4.029744825116962303, 4.573446973323917142 ) ) ;
#14186 = CARTESIAN_POINT ( 'NONE',  ( -9.819578298036041986, 117.9942579372833933, -0.2115136170467757371 ) ) ;
#14187 = CARTESIAN_POINT ( 'NONE',  ( -13.85159022459153988, 60.48513866567135722, -5.016500000000000625 ) ) ;
#14188 = DIRECTION ( 'NONE',  ( 0.1728608224830406603, -0.000000000000000000, -0.9849462604886047856 ) ) ;
#14189 = EDGE_LOOP ( 'NONE', ( #11922, #16644, #17909, #26794 ) ) ;
#14190 = CARTESIAN_POINT ( 'NONE',  ( -6.548379015483123844, 119.7817990349845587, 0.9906393647722963047 ) ) ;
#14191 = CARTESIAN_POINT ( 'NONE',  ( -2.488979065607898722, -9.142725400274830605, 3.900846118434742493 ) ) ;
#14192 = CARTESIAN_POINT ( 'NONE',  ( 22.06201951068898737, 142.1041199125429557, 1.893492075525809115 ) ) ;
#14193 = CARTESIAN_POINT ( 'NONE',  ( -58.22785051087659980, 0.5684335961349124000, -1.101539904998067865 ) ) ;
#14194 = CARTESIAN_POINT ( 'NONE',  ( 13.26531225419051729, 121.8780043825237982, -1.199064809579205360 ) ) ;
#14195 = CARTESIAN_POINT ( 'NONE',  ( 0.6256056815405413030, -8.068247431453825058, 4.577905309659676014 ) ) ;
#14196 = CARTESIAN_POINT ( 'NONE',  ( -7.599585376671227799, 158.5456267226934131, -1.164890904197547039 ) ) ;
#14197 = ORIENTED_EDGE ( 'NONE', *, *, #33778, .F. ) ;
#14198 = CARTESIAN_POINT ( 'NONE',  ( -15.42372963437265376, 147.8340308814284754, 0.02010286832636639515 ) ) ;
#14200 = CARTESIAN_POINT ( 'NONE',  ( 5.820489720963992752, -14.55473177801069795, 2.572867947693331381 ) ) ;
#14199 = AXIS2_PLACEMENT_3D ( 'NONE', #16142, #25740, #29144 ) ;
#14201 = TOROIDAL_SURFACE ( 'NONE', #15539, 3.683000000000000718, 0.5080000000000000071 ) ;
#14202 = CARTESIAN_POINT ( 'NONE',  ( -47.59458007651505795, 19.66657808744504976, 5.176039278149815459 ) ) ;
#14203 = DIRECTION ( 'NONE',  ( -1.000000000000000000, 1.288607544181256449E-16, 0.000000000000000000 ) ) ;
#14204 = ORIENTED_EDGE ( 'NONE', *, *, #29434, .F. ) ;
#14205 = CARTESIAN_POINT ( 'NONE',  ( 13.91666582400468677, 125.7699432187419575, 2.002145485623347376 ) ) ;
#14206 = CARTESIAN_POINT ( 'NONE',  ( 4.946784285683848204, 117.5302610941451178, 0.9662579091233235440 ) ) ;
#14207 = FACE_OUTER_BOUND ( 'NONE', #41288, .T. ) ;
#14208 = CARTESIAN_POINT ( 'NONE',  ( -17.61824099940339750, 125.1652531886817172, 0.6886689253619218132 ) ) ;
#14209 = CARTESIAN_POINT ( 'NONE',  ( 7.425401986171529245, 12.64277321918224040, 4.020893088955488359 ) ) ;
#14210 = CARTESIAN_POINT ( 'NONE',  ( 4.456531362648481043, 120.8671296916768227, 0.5026912216012411339 ) ) ;
#14211 = FACE_OUTER_BOUND ( 'NONE', #39905, .T. ) ;
#14212 = CARTESIAN_POINT ( 'NONE',  ( 22.91960207526958726, 149.8162411397050278, -0.2683370967508545424 ) ) ;
#14213 = CARTESIAN_POINT ( 'NONE',  ( -57.20840289379589905, 2.209747822858734612, 1.646108566719461042 ) ) ;
#14214 = CARTESIAN_POINT ( 'NONE',  ( -3.682264917456324671, 101.1854662015457365, -0.07358041635423923088 ) ) ;
#14215 = ADVANCED_FACE ( 'NONE', ( #25945 ), #9553, .T. ) ;
#14216 = CARTESIAN_POINT ( 'NONE',  ( -57.85534701229748578, 0.8496279762696679061, 1.203237356453206619 ) ) ;
#14217 = CARTESIAN_POINT ( 'NONE',  ( -57.60391329870441979, 1.913983619093638122, 1.729326818512549657 ) ) ;
#14218 = CARTESIAN_POINT ( 'NONE',  ( -4.507460450193894630, 118.1171274854782212, 0.5525917382868535954 ) ) ;
#14219 = CARTESIAN_POINT ( 'NONE',  ( 0.3831223070221896343, 105.9763118359730214, -5.290145194802176043 ) ) ;
#14220 = ORIENTED_EDGE ( 'NONE', *, *, #18525, .T. ) ;
#14221 = CARTESIAN_POINT ( 'NONE',  ( -43.10982161678889213, 22.52422253607401359, 1.888110242252979631 ) ) ;
#14222 = TOROIDAL_SURFACE ( 'NONE', #2668, 8.794749999999996959, 0.2540000000000000036 ) ;
#14223 = CARTESIAN_POINT ( 'NONE',  ( -6.121904736440446193, 119.5860228115829358, -1.252076594595966652 ) ) ;
#14224 = CIRCLE ( 'NONE', #16255, 0.7620000000000015650 ) ;
#14225 = CARTESIAN_POINT ( 'NONE',  ( -0.6661646497577808912, 105.9485402691003060, -5.310688274649121077 ) ) ;
#14226 = CARTESIAN_POINT ( 'NONE',  ( 4.455728184749551346, 118.1125308307683355, 0.7544055872226939075 ) ) ;
#14227 = CARTESIAN_POINT ( 'NONE',  ( -15.86545709684700256, 148.0001117310855250, -1.424070646214982139 ) ) ;
#14228 = CARTESIAN_POINT ( 'NONE',  ( -0.9216814595139277699, 115.7029463646975245, -1.750463915914598934 ) ) ;
#14229 = CARTESIAN_POINT ( 'NONE',  ( 6.349999999999948130, 83.56599999999998829, 5.803602218936700314E-46 ) ) ;
#14230 = CARTESIAN_POINT ( 'NONE',  ( 5.966545996697649734, 118.9610140496397719, -0.3495452691818399238 ) ) ;
#14231 = CARTESIAN_POINT ( 'NONE',  ( -7.189601074672337333, 121.4526873951801633, -0.9441605179235378342 ) ) ;
#14232 = B_SPLINE_CURVE_WITH_KNOTS ( 'NONE', 3,
 ( #29050, #22844, #19877, #22635, #13286, #32042, #35456, #26271, #2879, #26062, #29686, #41861, #6278, #42068, #16047, #39072, #12864, #25850, #6694, #19663, #29477, #319, #36092, #30521, #4562, #4358, #17725, #20081, #20498, #27117, #14319, #37133, #16894, #17521, #10511, #39710, #33104, #33525, #20922 ),
 .UNSPECIFIED., .F., .F.,
 ( 4, 2, 1, 1, 1, 2, 2, 2, 2, 1, 1, 2, 2, 2, 2, 1, 2, 2, 2, 1, 2, 2, 4 ),
 ( 0.000000000000000000, 0.06250000000019394208, 0.09375000000028790859, 0.1093750000003349682, 0.1171875000003639727, 0.1210937500003731876, 0.1250000000003823886, 0.1875000000005171974, 0.2187500000005817291, 0.2343750000006132317, 0.2421875000006274425, 0.2460937500006222522, 0.2500000000006170620, 0.3750000000004883871, 0.4375000000004232170, 0.4687500000003906320, 0.4843750000003776979, 0.5000000000003647083, 0.6250000000002644551, 0.6875000000002159384, 0.7187500000001945111, 0.7500000000001730838, 1.000000000000000000 ),
 .UNSPECIFIED. ) ;
#14233 = CARTESIAN_POINT ( 'NONE',  ( -5.260208640450895423, 116.0444662015457595, -1.274361246762516942 ) ) ;
#14234 = CARTESIAN_POINT ( 'NONE',  ( -30.28638171898572651, 70.19821000523995735, 1.269999999999990692 ) ) ;
#14235 = CARTESIAN_POINT ( 'NONE',  ( 8.663704466952500738, 118.4235366968211736, -0.7034480781449402587 ) ) ;
#14236 = CARTESIAN_POINT ( 'NONE',  ( -0.6427210712090456468, 156.3034662015459446, 0.05863295770775731747 ) ) ;
#14237 = LINE ( 'NONE', #11258, #10263 ) ;
#14238 = CARTESIAN_POINT ( 'NONE',  ( 13.19686234056486640, 119.7880570645780978, 0.9111371353940663775 ) ) ;
#14239 = CARTESIAN_POINT ( 'NONE',  ( 5.241362157049057835, 65.30181249999998272, -5.310945289804168468 ) ) ;
#14240 = CARTESIAN_POINT ( 'NONE',  ( 2.997986829609769366, -15.20712831582179980, 4.056362312997196184 ) ) ;
#14241 = CARTESIAN_POINT ( 'NONE',  ( -5.876330432687375982, 119.7498067647950961, 0.9241301181796095499 ) ) ;
#14242 = CARTESIAN_POINT ( 'NONE',  ( 0.05045227420522335748, 0.5774631391966889016, 0.9751023907654918776 ) ) ;
#14243 = CARTESIAN_POINT ( 'NONE',  ( -14.97360968503865131, 156.1447123740162226, -0.9344295344441083673 ) ) ;
#14244 = CARTESIAN_POINT ( 'NONE',  ( 0.4410767147925211407, 14.17415678908661469, -0.8685042294053136880 ) ) ;
#14245 = ORIENTED_EDGE ( 'NONE', *, *, #35752, .T. ) ;
#14246 = CARTESIAN_POINT ( 'NONE',  ( -50.02669608763527265, 12.78473261814652773, 0.3947048150275107581 ) ) ;
#14247 = CARTESIAN_POINT ( 'NONE',  ( 7.301789825441145965, 123.0387167848234355, 0.2146691528375952174 ) ) ;
#14248 = CARTESIAN_POINT ( 'NONE',  ( -10.17757484390040545, 124.8647468421599598, 0.4356504197092354591 ) ) ;
#14249 = CARTESIAN_POINT ( 'NONE',  ( 3.112015045868556928, -14.86597822091932564, 5.561823117377171499 ) ) ;
#14250 = CARTESIAN_POINT ( 'NONE',  ( 1.968159265821130877, 156.7095495334699535, -1.232728320231046837 ) ) ;
#14251 = ORIENTED_EDGE ( 'NONE', *, *, #2235, .T. ) ;
#14252 = CARTESIAN_POINT ( 'NONE',  ( 4.497658079560046041, 104.6144662015457243, 1.758835774636801963 ) ) ;
#14253 = CARTESIAN_POINT ( 'NONE',  ( 3.036083976128487016, -13.30543680819082297, 1.158518541688273729 ) ) ;
#14254 = CARTESIAN_POINT ( 'NONE',  ( -4.960352205898358235, 117.4682330514041553, -0.9861013956279517378 ) ) ;
#14255 = CARTESIAN_POINT ( 'NONE',  ( 15.73538347863339482, 145.6958675726371553, 0.1858358763210238851 ) ) ;
#14256 = VECTOR ( 'NONE', #6736, 1000.000000000000114 ) ;
#14257 = EDGE_LOOP ( 'NONE', ( #20749, #12579, #31415, #11209 ) ) ;
#14258 = CARTESIAN_POINT ( 'NONE',  ( 4.088037439073622714, 118.5849532427036905, 0.9900007573961082663 ) ) ;
#14259 = CIRCLE ( 'NONE', #38080, 0.2539999999999956737 ) ;
#14260 =( REPRESENTATION_RELATIONSHIP ('NONE','NONE', #30767, #22056 ) REPRESENTATION_RELATIONSHIP_WITH_TRANSFORMATION ( #1290 )SHAPE_REPRESENTATION_RELATIONSHIP( ) );
#14261 = DIRECTION ( 'NONE',  ( 9.627370216492862708E-17, 1.000000000000000000, -0.000000000000000000 ) ) ;
#14262 = FACE_OUTER_BOUND ( 'NONE', #9377, .T. ) ;
#14263 = CARTESIAN_POINT ( 'NONE',  ( 20.37188742667021657, 129.0035756037533758, 0.2165721192533108241 ) ) ;
#14264 = CARTESIAN_POINT ( 'NONE',  ( 4.825036788390894671, 63.33946620154573282, 0.09641571798141751470 ) ) ;
#14265 = CARTESIAN_POINT ( 'NONE',  ( 1.854099703272072519, -15.70493002892270340, 5.640771195865757370 ) ) ;
#14266 = DIRECTION ( 'NONE',  ( 0.7071067811865465735, -0.7071067811865484609, 0.000000000000000000 ) ) ;
#14267 = CARTESIAN_POINT ( 'NONE',  ( -4.986976911676294755, 117.3993830381834726, -0.9021275479513909401 ) ) ;
#14268 = CARTESIAN_POINT ( 'NONE',  ( 19.16059698253082999, 135.9655892003723636, 2.351238754465550862 ) ) ;
#14269 = ORIENTED_EDGE ( 'NONE', *, *, #22929, .T. ) ;
#14270 = CARTESIAN_POINT ( 'NONE',  ( -7.287282906664737325, 21.23368160547805061, -4.223004820119153457 ) ) ;
#14271 = B_SPLINE_CURVE_WITH_KNOTS ( 'NONE', 3,
 ( #41729, #32335, #32544, #6155 ),
 .UNSPECIFIED., .F., .F.,
 ( 4, 4 ),
 ( 0.000000000000000000, 1.000000000000000000 ),
 .UNSPECIFIED. ) ;
#14272 = CARTESIAN_POINT ( 'NONE',  ( 5.564818521742781243, 117.9257778791303934, -0.8576562958995672670 ) ) ;
#14273 = CARTESIAN_POINT ( 'NONE',  ( -1.673685645604704231, 111.6436615656963909, -3.078281589618439451 ) ) ;
#14274 = CARTESIAN_POINT ( 'NONE',  ( -5.632494751984450154, 78.90911215162431347, 5.063853515468840882 ) ) ;
#14275 = DIRECTION ( 'NONE',  ( -1.000000000000000000, 0.000000000000000000, 0.000000000000000000 ) ) ;
#14276 = FACE_OUTER_BOUND ( 'NONE', #2068, .T. ) ;
#14277 = CARTESIAN_POINT ( 'NONE',  ( -0.9211762648548540433, 10.43857344512876040, -4.529598961101950927 ) ) ;
#14278 = DIRECTION ( 'NONE',  ( -0.8745520943968243532, 0.4849315768086547296, -5.361993529360573944E-16 ) ) ;
#14279 = CARTESIAN_POINT ( 'NONE',  ( -4.844532766435863280, 115.6909491485453003, 1.283482262965630838 ) ) ;
#14280 = CARTESIAN_POINT ( 'NONE',  ( 3.301452709780442252, -13.00349394711965090, 1.536261971075179478 ) ) ;
#14281 = CARTESIAN_POINT ( 'NONE',  ( 1.341555883842814101, 107.4826764677166864, -4.621745984720207368 ) ) ;
#14282 = CIRCLE ( 'NONE', #20385, 12.69999999999999751 ) ;
#14283 = CARTESIAN_POINT ( 'NONE',  ( 1.963896995744959684, 39.20946620154573026, 1.309496863130310329 ) ) ;
#14284 = LINE ( 'NONE', #17068, #14116 ) ;
#14285 = ORIENTED_EDGE ( 'NONE', *, *, #35816, .T. ) ;
#14286 = CARTESIAN_POINT ( 'NONE',  ( -4.689376690405532067, 104.6144662015456959, -1.152304354653030716 ) ) ;
#14287 = CARTESIAN_POINT ( 'NONE',  ( 2.110750219194173827, -15.67940412490098723, 5.433654451060461632 ) ) ;
#14288 = CARTESIAN_POINT ( 'NONE',  ( -19.88689915616629378, 147.6055923437354238, 1.726923636697636599 ) ) ;
#14289 = CARTESIAN_POINT ( 'NONE',  ( -1.504723661876595786, -8.552649586842417051, -4.374500482163298898 ) ) ;
#14290 = ORIENTED_EDGE ( 'NONE', *, *, #1206, .T. ) ;
#14291 = ORIENTED_EDGE ( 'NONE', *, *, #13479, .F. ) ;
#14292 = CARTESIAN_POINT ( 'NONE',  ( -4.468667403750213651, 27.88063884994054220, 0.5133561255362272258 ) ) ;
#14293 = CARTESIAN_POINT ( 'NONE',  ( 1.585818144368541960, 119.1892773189224783, 0.7268676395674206203 ) ) ;
#14294 = CARTESIAN_POINT ( 'NONE',  ( -10.91797240702851290, 124.6990478933366404, 0.8611562105571396453 ) ) ;
#14295 = CARTESIAN_POINT ( 'NONE',  ( -6.484670282503085616E-14, 71.97546620154574271, 3.533028205012241021E-29 ) ) ;
#14296 = CARTESIAN_POINT ( 'NONE',  ( 12.23061257473121088, 124.2599011343719155, -1.262879005329815341 ) ) ;
#14297 = CARTESIAN_POINT ( 'NONE',  ( -13.40750253236534917, 122.4565580348552913, -1.800089891214285531 ) ) ;
#14298 = AXIS2_PLACEMENT_3D ( 'NONE', #24726, #33916, #11522 ) ;
#14299 = CARTESIAN_POINT ( 'NONE',  ( 4.269133473500895448, 118.2238350903788131, -0.2888805705710837946 ) ) ;
#14300 = CARTESIAN_POINT ( 'NONE',  ( 14.89139266796658845, 148.8756053271976327, -0.4181552259878849598 ) ) ;
#14301 = ORIENTED_EDGE ( 'NONE', *, *, #4113, .T. ) ;
#14302 = CARTESIAN_POINT ( 'NONE',  ( 3.047145566129288330, -14.72663143740328806, 3.823360744794035870 ) ) ;
#14303 = AXIS2_PLACEMENT_3D ( 'NONE', #27890, #37077, #11285 ) ;
#14304 = FACE_OUTER_BOUND ( 'NONE', #6560, .T. ) ;
#14305 = CARTESIAN_POINT ( 'NONE',  ( -57.45676042279916373, 1.677525466756688122, 1.437765377952616275 ) ) ;
#14306 = CARTESIAN_POINT ( 'NONE',  ( 4.471266627501615076, -5.469457446779734333, -1.220754042301255948 ) ) ;
#14307 = CARTESIAN_POINT ( 'NONE',  ( 15.77815547270811791, 139.7295799824062499, 1.909820663798255325 ) ) ;
#14308 = CARTESIAN_POINT ( 'NONE',  ( -3.521685918548247418, 29.33394459973516888, 3.031038535435704340 ) ) ;
#14309 = CARTESIAN_POINT ( 'NONE',  ( -4.039333660417916860, 117.0582680968029905, 0.9406562914258045360 ) ) ;
#14310 = CIRCLE ( 'NONE', #8950, 0.3810000000000015041 ) ;
#14311 = ADVANCED_FACE ( 'NONE', ( #17206 ), #20808, .T. ) ;
#14312 = CARTESIAN_POINT ( 'NONE',  ( -1.756104463947763206, 14.33678105357426702, 4.288642365192034234 ) ) ;
#14313 = CARTESIAN_POINT ( 'NONE',  ( 0.6411011158478991945, 120.9975462804897433, 0.03814546805551061875 ) ) ;
#14314 = CARTESIAN_POINT ( 'NONE',  ( -10.28897677580358305, 56.51499999999998636, 4.381499999999999950 ) ) ;
#14315 = ADVANCED_FACE ( 'NONE', ( #33834 ), #13133, .T. ) ;
#14316 = CARTESIAN_POINT ( 'NONE',  ( -55.10067240196883631, 5.634149028679341420, -0.4880682687716038637 ) ) ;
#14317 = CARTESIAN_POINT ( 'NONE',  ( -2.169587742970651156, 116.2588381394661354, -0.2119676221548945638 ) ) ;
#14318 = CARTESIAN_POINT ( 'NONE',  ( 0.003073426023161661153, 123.4679809879534247, -0.1538068059577044622 ) ) ;
#14319 = CARTESIAN_POINT ( 'NONE',  ( -46.87659121548133356, 25.47535466239702728, -1.649981827335061713 ) ) ;
#14320 = CARTESIAN_POINT ( 'NONE',  ( -2.100979515209699944, 106.6614287958282858, 4.900381384812394714 ) ) ;
#14321 = PLANE ( 'NONE',  #11356 ) ;
#14322 = VECTOR ( 'NONE', #28455, 1000.000000000000000 ) ;
#14323 = CARTESIAN_POINT ( 'NONE',  ( 8.429690783291841072, 7.639065531857588631, 0.01617727833786941974 ) ) ;
#14324 = FACE_OUTER_BOUND ( 'NONE', #31158, .T. ) ;
#14325 = CARTESIAN_POINT ( 'NONE',  ( -58.80872392184672037, -0.02106340533553074934, 0.1867271868312104510 ) ) ;
#14326 = CARTESIAN_POINT ( 'NONE',  ( 0.003073426022489101923, 123.4679809879534247, -0.1538068059577179236 ) ) ;
#14327 = CARTESIAN_POINT ( 'NONE',  ( -22.40468623258675507, 137.0915487549672491, 0.1281257692620775268 ) ) ;
#14328 = ORIENTED_EDGE ( 'NONE', *, *, #11061, .F. ) ;
#14329 = CARTESIAN_POINT ( 'NONE',  ( -58.10740272659374739, 1.828491270143103975, -0.5949618876680415891 ) ) ;
#14330 = CYLINDRICAL_SURFACE ( 'NONE', #39847, 2.540000000000000480 ) ;
#14331 = VERTEX_POINT ( 'NONE', #1462 ) ;
#14332 = CARTESIAN_POINT ( 'NONE',  ( -46.36020037344893296, 20.58642004076050469, -4.649377256145048598 ) ) ;
#14334 = CARTESIAN_POINT ( 'NONE',  ( -15.78437780952707215, 146.2378312303354448, -0.3154094333657934679 ) ) ;
#14333 = AXIS2_PLACEMENT_3D ( 'NONE', #17042, #34092, #33677 ) ;
#14335 = CARTESIAN_POINT ( 'NONE',  ( 5.122375111755775201, -14.64399685039916044, 3.991980633533394052 ) ) ;
#14336 = CARTESIAN_POINT ( 'NONE',  ( -20.96550312372672664, 148.3608207065297222, 1.563628808460498787 ) ) ;
#14337 = CARTESIAN_POINT ( 'NONE',  ( 15.50334291652339580, 121.0440340969820596, 0.8284681841690884063 ) ) ;
#14338 = CARTESIAN_POINT ( 'NONE',  ( 12.83198513809769636, 156.8686255264331635, -0.8772202223719092196 ) ) ;
#14339 = CARTESIAN_POINT ( 'NONE',  ( -30.84347056137454146, 55.46442681907723937, 1.269999999999994023 ) ) ;
#14340 = CARTESIAN_POINT ( 'NONE',  ( 0.002459401150240396027, 159.6023738651833810, -0.1230784904792617679 ) ) ;
#14341 = CARTESIAN_POINT ( 'NONE',  ( -48.86598066419526276, 18.03485269033233607, -5.140156453303863948 ) ) ;
#14342 = ORIENTED_EDGE ( 'NONE', *, *, #19024, .F. ) ;
#14343 = CARTESIAN_POINT ( 'NONE',  ( 5.562407744872148285, 116.6996333493949436, 0.1111501445372547886 ) ) ;
#14344 = CARTESIAN_POINT ( 'NONE',  ( -4.309327875669019647, 119.9149831030956932, 0.7077533764146595185 ) ) ;
#14345 = CARTESIAN_POINT ( 'NONE',  ( -58.03609167196196239, 0.4261842582088196107, -0.8102809492608903374 ) ) ;
#14346 = CARTESIAN_POINT ( 'NONE',  ( 18.61143607275140965, 150.2488615152233820, -1.729315005182988196 ) ) ;
#14347 = CARTESIAN_POINT ( 'NONE',  ( -4.583145339711863109, 27.87760190725156662, 0.5120832130453706332 ) ) ;
#14348 = CARTESIAN_POINT ( 'NONE',  ( -10.72975491961958383, 119.6772744462923157, -1.366487948980413147 ) ) ;
#14349 = CARTESIAN_POINT ( 'NONE',  ( -43.10982161678889213, 22.52422253607401359, -1.888110242252992066 ) ) ;
#14350 = EDGE_CURVE ( 'NONE', #26023, #10127, #10394, .T. ) ;
#14351 = CARTESIAN_POINT ( 'NONE',  ( 16.52109770691737722, 146.2355833862463328, -0.9494891650916719161 ) ) ;
#14352 = CARTESIAN_POINT ( 'NONE',  ( -15.72385166996626715, 146.8976323831864477, -0.3141999770531619940 ) ) ;
#14353 = ORIENTED_EDGE ( 'NONE', *, *, #19378, .T. ) ;
#14354 = CARTESIAN_POINT ( 'NONE',  ( -15.37772490044532070, 131.3329289045130679, -2.176645470406190608 ) ) ;
#14355 = CARTESIAN_POINT ( 'NONE',  ( 4.438132741721911856, -15.66483130081081043, 3.040968155030625120 ) ) ;
#14356 = DIRECTION ( 'NONE',  ( 0.8745520943968235761, -0.4849315768086558398, 0.000000000000000000 ) ) ;
#14357 = CARTESIAN_POINT ( 'NONE',  ( -4.291595391187098762, 118.2137919694442019, -0.5063013721726838945 ) ) ;
#14358 = AXIS2_PLACEMENT_3D ( 'NONE', #19177, #5795, #32183 ) ;
#14359 = CARTESIAN_POINT ( 'NONE',  ( -54.97180548219925100, 8.422794459035404913, -3.467293221275798309 ) ) ;
#14360 = CARTESIAN_POINT ( 'NONE',  ( 4.112379816251298337, 118.2429491485453354, 0.3456808358118761970 ) ) ;
#14361 = CARTESIAN_POINT ( 'NONE',  ( -0.01023306027097531379, 119.5380416804913324, 0.5121041807152043601 ) ) ;
#14362 = FACE_OUTER_BOUND ( 'NONE', #38499, .T. ) ;
#14363 = VECTOR ( 'NONE', #36143, 1000.000000000000000 ) ;
#14364 = CARTESIAN_POINT ( 'NONE',  ( 18.86374853661768825, 125.3403196291361610, 0.3769425889880998470 ) ) ;
#14365 = EDGE_CURVE ( 'NONE', #30834, #19419, #16530, .T. ) ;
#14366 = CARTESIAN_POINT ( 'NONE',  ( 4.103208822911150300, 18.85939590645278585, -7.354229849909827088 ) ) ;
#14367 = CARTESIAN_POINT ( 'NONE',  ( 6.089391457280314945, 155.3491548655973133, 0.5861119247043798941 ) ) ;
#14368 = CARTESIAN_POINT ( 'NONE',  ( 22.76023949468076069, 146.4845460041848355, -0.7370798038890573611 ) ) ;
#14369 = CARTESIAN_POINT ( 'NONE',  ( 5.475330206976797953, 57.14999999999998437, 5.107412922131463695 ) ) ;
#14370 = VECTOR ( 'NONE', #18671, 999.9999999999998863 ) ;
#14371 = CARTESIAN_POINT ( 'NONE',  ( 3.195221254476268591, 115.6909491485452435, 1.660623339098961093 ) ) ;
#14372 = CARTESIAN_POINT ( 'NONE',  ( -57.97703582661664967, 0.5002880090035632943, 0.5798895178195145883 ) ) ;
#14373 = EDGE_CURVE ( 'NONE', #22759, #30888, #8358, .T. ) ;
#14374 = CARTESIAN_POINT ( 'NONE',  ( -23.35954322469569178, 148.8716009884483071, -0.3896314068422417898 ) ) ;
#14375 = ORIENTED_EDGE ( 'NONE', *, *, #11343, .F. ) ;
#14376 = CARTESIAN_POINT ( 'NONE',  ( -46.72388148998840762, 26.09838203902186393, -9.431828030254277901E-15 ) ) ;
#14377 = CARTESIAN_POINT ( 'NONE',  ( -6.873076553849402082, 121.7066554103861620, -0.6264859833759695018 ) ) ;
#14378 = CARTESIAN_POINT ( 'NONE',  ( -17.64950171984354199, 84.16951713491046405, 1.523999999999996247 ) ) ;
#14379 = VERTEX_POINT ( 'NONE', #832 ) ;
#14380 = CARTESIAN_POINT ( 'NONE',  ( 4.459091033076425070, 115.6909491485368306, -1.361484950952978279 ) ) ;
#14381 = CARTESIAN_POINT ( 'NONE',  ( -10.44459398727727262, 153.0728660266736370, -0.5066767128784233076 ) ) ;
#14382 = CARTESIAN_POINT ( 'NONE',  ( 4.035643413487081332, -14.09208526182970189, 4.581805149448960002 ) ) ;
#14383 = AXIS2_PLACEMENT_3D ( 'NONE', #10416, #36204, #3839 ) ;
#14384 = CARTESIAN_POINT ( 'NONE',  ( -21.39260515875404778, 150.3702682424204511, 1.149856210633945830 ) ) ;
#14385 = CARTESIAN_POINT ( 'NONE',  ( -41.06677624538416183, 23.07857903911245501, 1.524000000000167221 ) ) ;
#14386 = AXIS2_PLACEMENT_3D ( 'NONE', #16478, #26067, #20086 ) ;
#14387 = CARTESIAN_POINT ( 'NONE',  ( 18.76446887325675661, 125.2887878443791294, 0.4910110098351363472 ) ) ;
#14388 = CARTESIAN_POINT ( 'NONE',  ( 1.558509422354653839, 156.2601852824606681, 0.06968051580646485166 ) ) ;
#14389 = VERTEX_POINT ( 'NONE', #4871 ) ;
#14390 = CARTESIAN_POINT ( 'NONE',  ( 0.8728101606606677443, 18.85996454746999618, -0.4358653558870161926 ) ) ;
#14391 = CARTESIAN_POINT ( 'NONE',  ( -23.34271727006419539, 149.0672090665632936, -0.4921983935722529235 ) ) ;
#14392 = AXIS2_PLACEMENT_3D ( 'NONE', #916, #36062, #26244 ) ;
#14393 = CARTESIAN_POINT ( 'NONE',  ( -41.25198945386213722, 23.25239630053127016, -1.523999999999987587 ) ) ;
#14394 = CARTESIAN_POINT ( 'NONE',  ( 16.60960244842765832, 17.14499999999999957, 2.034089647357696937E-15 ) ) ;
#14395 = ORIENTED_EDGE ( 'NONE', *, *, #18291, .T. ) ;
#14396 = CARTESIAN_POINT ( 'NONE',  ( 4.555470457886838354, 118.7543979957781488, 1.067760081256754034 ) ) ;
#14397 = CARTESIAN_POINT ( 'NONE',  ( -3.769861741716944881, -2.021032284792064093, -2.673854242032364326 ) ) ;
#14398 = CARTESIAN_POINT ( 'NONE',  ( 2.976591712665050515, 117.3922842568077698, 0.6615242749010382672 ) ) ;
#14399 = CARTESIAN_POINT ( 'NONE',  ( -58.41257333834580834, 0.1697474083101613296, -0.8453419536803969958 ) ) ;
#14400 = CARTESIAN_POINT ( 'NONE',  ( 19.52548538990935612, 136.0480396440595996, -1.529100095608182608 ) ) ;
#14401 = CARTESIAN_POINT ( 'NONE',  ( -4.540528814728789442, -1.371322978654152092, -0.8806307088788817294 ) ) ;
#14402 = CARTESIAN_POINT ( 'NONE',  ( -6.873244579178622082, 117.6856483911789581, -0.8154597436780148811 ) ) ;
#14403 = EDGE_CURVE ( 'NONE', #10127, #38754, #30141, .T. ) ;
#14404 = ORIENTED_EDGE ( 'NONE', *, *, #15368, .F. ) ;
#14405 = CARTESIAN_POINT ( 'NONE',  ( -14.24343488940578162, 138.9464670490549452, -0.05414037600900920011 ) ) ;
#14406 = EDGE_CURVE ( 'NONE', #10361, #40008, #24802, .T. ) ;
#14407 = CARTESIAN_POINT ( 'NONE',  ( 4.690731670358166738, -15.11132977793584686, 4.439372980131230939 ) ) ;
#14408 = CARTESIAN_POINT ( 'NONE',  ( 5.012350601733652766, 115.6909491485453145, 1.400347971660041990 ) ) ;
#14409 = EDGE_CURVE ( 'NONE', #38197, #4283, #36404, .T. ) ;
#14410 = CARTESIAN_POINT ( 'NONE',  ( 0.01782677789211616418, 118.1651005001175889, -0.8921251404964753995 ) ) ;
#14411 = ORIENTED_EDGE ( 'NONE', *, *, #37367, .F. ) ;
#14412 = CARTESIAN_POINT ( 'NONE',  ( 3.256054338613350474, 118.9727644790723531, 0.9029027703446365072 ) ) ;
#14413 = FACE_OUTER_BOUND ( 'NONE', #14257, .T. ) ;
#14414 = CARTESIAN_POINT ( 'NONE',  ( -29.50088714511802834, 67.43771171077483473, -1.270000000000005569 ) ) ;
#14415 = AXIS2_PLACEMENT_3D ( 'NONE', #26913, #35207, #5618 ) ;
#14416 = CARTESIAN_POINT ( 'NONE',  ( -22.39452804842998646, 149.5981344557702641, 0.8550856607202137472 ) ) ;
#14417 = CARTESIAN_POINT ( 'NONE',  ( 4.653112868187331941, 2.303567304790777648, 7.043327697551765354 ) ) ;
#14418 = CARTESIAN_POINT ( 'NONE',  ( 14.76847666019552463, 139.2804412874323248, 1.275673245633013542 ) ) ;
#14419 = DIRECTION ( 'NONE',  ( -0.1565721916418034432, -0.9876665170007953298, 8.659954811667511346E-17 ) ) ;
#14420 = EDGE_CURVE ( 'NONE', #18326, #8589, #40643, .T. ) ;
#14421 = CARTESIAN_POINT ( 'NONE',  ( 1.919474982883598191, 116.7789519286944966, -0.2705014076049041538 ) ) ;
#14422 = CARTESIAN_POINT ( 'NONE',  ( -57.77486378051489169, 0.9916650371046533685, 1.126111947105124189 ) ) ;
#14423 =( NAMED_UNIT ( * ) PLANE_ANGLE_UNIT ( ) SI_UNIT ( $, .RADIAN. ) );
#14424 = CARTESIAN_POINT ( 'NONE',  ( -58.33777482027510786, 1.113448835244251756, 1.208045587469420701 ) ) ;
#14425 = CARTESIAN_POINT ( 'NONE',  ( -58.62423747511084571, -0.2805004185027809571, 0.3924598736681575439 ) ) ;
#14426 = CARTESIAN_POINT ( 'NONE',  ( -4.172365507229960357, 118.2392283616613042, 0.2172622651388938786 ) ) ;
#14427 = CARTESIAN_POINT ( 'NONE',  ( 2.005054034524792694, 106.7498038803853291, -4.871448594665350740 ) ) ;
#14428 = ORIENTED_EDGE ( 'NONE', *, *, #5832, .F. ) ;
#14429 = CARTESIAN_POINT ( 'NONE',  ( -48.53848336910535011, 19.22582880449973075, 5.323527254358031868 ) ) ;
#14430 = CARTESIAN_POINT ( 'NONE',  ( -6.231363852629784539, 119.8171196943256405, -1.230295645515693481 ) ) ;
#14431 = CARTESIAN_POINT ( 'NONE',  ( -5.166232791442098460, 115.4535745449993982, -1.513138011745335909 ) ) ;
#14432 = CARTESIAN_POINT ( 'NONE',  ( 4.388083867990050457, 118.1817479911534861, 0.5768821283915082088 ) ) ;
#14433 = CARTESIAN_POINT ( 'NONE',  ( 0.01341678693497577735, 156.4123495908283985, -0.6714308817992609146 ) ) ;
#14434 =( LENGTH_UNIT ( ) NAMED_UNIT ( * ) SI_UNIT ( .MILLI., .METRE. ) );
#14435 = CARTESIAN_POINT ( 'NONE',  ( 5.772319165917887851, 116.9338547871927858, 0.1153446742911717476 ) ) ;
#14436 = ORIENTED_EDGE ( 'NONE', *, *, #13568, .T. ) ;
#14437 = CARTESIAN_POINT ( 'NONE',  ( 2.184544675937996061, 106.6795586461009009, -4.886581511092879637 ) ) ;
#14438 = CARTESIAN_POINT ( 'NONE',  ( -3.555938004931326724, 120.5283240077024800, -0.5587344792657804593 ) ) ;
#14439 = CARTESIAN_POINT ( 'NONE',  ( -41.05193670661653016, 23.09446788613700363, -1.270000000071892066 ) ) ;
#14440 = CARTESIAN_POINT ( 'NONE',  ( -44.18728704178793265, 21.36917510656546781, 3.097942224162542058 ) ) ;
#14441 = ADVANCED_FACE ( 'NONE', ( #7221 ), #29992, .T. ) ;
#14442 = LINE ( 'NONE', #27451, #41258 ) ;
#14443 = CARTESIAN_POINT ( 'NONE',  ( -12.77395747310483642, 133.6867917047960930, -0.07034420110178993268 ) ) ;
#14444 = DIRECTION ( 'NONE',  ( -0.9454731675810330582, 0.3256999990547865265, -7.568290090144850389E-15 ) ) ;
#14445 = CARTESIAN_POINT ( 'NONE',  ( 4.811924804297746938, 117.0737178285515654, 0.5427311436463463368 ) ) ;
#14446 = CARTESIAN_POINT ( 'NONE',  ( 14.39766717389551864, 57.78500000000000369, -1.904999999999999583 ) ) ;
#14448 = CARTESIAN_POINT ( 'NONE',  ( 21.81117068996439556, 146.0876064316611860, -1.285479812297503743 ) ) ;
#14447 = CARTESIAN_POINT ( 'NONE',  ( 2.567065079198288746, -15.08448375773686934, 4.691402903081304920 ) ) ;
#14449 = CARTESIAN_POINT ( 'NONE',  ( -3.371641211477255151, 119.4525916976722897, 0.7211689390744321360 ) ) ;
#14450 = CARTESIAN_POINT ( 'NONE',  ( 0.3265437062995015238, -4.820036860806069967, -0.9201843903956486992 ) ) ;
#14451 = CARTESIAN_POINT ( 'NONE',  ( -2.866641708098142338, 116.8851979753409580, -0.4370437109847168378 ) ) ;
#14452 = CONICAL_SURFACE ( 'NONE', #29417, 2.540000000000002256, 0.7853981633974523868 ) ;
#14453 = CARTESIAN_POINT ( 'NONE',  ( -0.4694259674403166716, 18.92165170904731397, 0.8533247626313392731 ) ) ;
#14454 = ORIENTED_EDGE ( 'NONE', *, *, #25944, .F. ) ;
#14455 = CARTESIAN_POINT ( 'NONE',  ( -51.26804087848103819, 14.04722136430348201, 4.535752393750700939 ) ) ;
#14456 = CARTESIAN_POINT ( 'NONE',  ( -5.892782515047567671, 121.3091694753028520, 0.3064017138515003902 ) ) ;
#14457 = CARTESIAN_POINT ( 'NONE',  ( 4.939475803799734166, -12.60685243851100701, 2.184682653711520040 ) ) ;
#14458 = CARTESIAN_POINT ( 'NONE',  ( 3.514252322483260471, 120.2313485970928326, -0.5318214084310806111 ) ) ;
#14459 = ORIENTED_EDGE ( 'NONE', *, *, #19393, .T. ) ;
#14460 = CARTESIAN_POINT ( 'NONE',  ( 1.647191010927073762, 104.6144662015456532, 4.545328324975800527 ) ) ;
#14461 = ADVANCED_FACE ( 'NONE', ( #17618 ), #25362, .T. ) ;
#14462 = CARTESIAN_POINT ( 'NONE',  ( 3.250423480262735421, -14.11372661294146802, 3.006569077614236196 ) ) ;
#14463 = CARTESIAN_POINT ( 'NONE',  ( -4.804485507087670193, 117.6428313260155960, -1.111657494208010188 ) ) ;
#14464 = CARTESIAN_POINT ( 'NONE',  ( 7.558302675500184087, 122.4263405438208991, 0.1204446389788525473 ) ) ;
#14465 = AXIS2_PLACEMENT_3D ( 'NONE', #38595, #22367, #6221 ) ;
#14466 = EDGE_CURVE ( 'NONE', #15919, #14963, #29665, .T. ) ;
#14467 = VERTEX_POINT ( 'NONE', #33412 ) ;
#14468 = CARTESIAN_POINT ( 'NONE',  ( 1.082660538731414990, 158.4310823543925721, 1.603207764552047054 ) ) ;
#14469 = CARTESIAN_POINT ( 'NONE',  ( 3.583481579166091446, 109.6950698699342865, 3.736516032388299546 ) ) ;
#14470 =( BOUNDED_CURVE ( )  B_SPLINE_CURVE ( 3, ( #16540, #6756, #25503, #6135 ),
 .UNSPECIFIED., .F., .F. ) 
 B_SPLINE_CURVE_WITH_KNOTS ( ( 4, 4 ),
 ( 1.570796326794894782, 2.532278806861536946 ),
 .UNSPECIFIED. ) 
 CURVE ( )  GEOMETRIC_REPRESENTATION_ITEM ( )  RATIONAL_B_SPLINE_CURVE ( ( 1.000000000000000000, 0.9244349266169026302, 0.9244349266169026302, 1.000000000000000000 ) ) 
 REPRESENTATION_ITEM ( '' )  );
#14471 = DIRECTION ( 'NONE',  ( -9.627370216492862708E-17, -1.000000000000000000, 0.000000000000000000 ) ) ;
#14472 = LINE ( 'NONE', #40693, #29978 ) ;
#14473 = CARTESIAN_POINT ( 'NONE',  ( 9.797860116729928848, 118.0024801742749929, 0.05693907317356660530 ) ) ;
#14474 = DIRECTION ( 'NONE',  ( -4.017660918040594346E-17, 1.000000000000000000, 2.376309959284834438E-19 ) ) ;
#14475 = CIRCLE ( 'NONE', #32870, 3.175000000000001155 ) ;
#14476 = CARTESIAN_POINT ( 'NONE',  ( 2.041957097679553801, -15.35386704983179840, 5.998528387730076794 ) ) ;
#14477 = CARTESIAN_POINT ( 'NONE',  ( 11.11710224466980712, 56.30409367656758235, 5.016500000000000625 ) ) ;
#14478 = CARTESIAN_POINT ( 'NONE',  ( -21.32888081312385253, 55.91420173801096638, 1.523999999999999133 ) ) ;
#14479 = CARTESIAN_POINT ( 'NONE',  ( -4.801861765505079482, 117.8465146159224588, 0.7715805027661067905 ) ) ;
#14480 = VERTEX_POINT ( 'NONE', #10817 ) ;
#14481 = CARTESIAN_POINT ( 'NONE',  ( -7.546363725996330984, 11.73557930518083303, -3.739946900464478752 ) ) ;
#14482 = CARTESIAN_POINT ( 'NONE',  ( 8.455193764574449489, 119.4765705532822722, -1.058376901205021259 ) ) ;
#14483 = CARTESIAN_POINT ( 'NONE',  ( -2.616318351458581937, 112.7379566594982663, -2.676765618731039797 ) ) ;
#14484 = CARTESIAN_POINT ( 'NONE',  ( 4.744914421628031675, 117.7318590736328758, 1.087530422288184528 ) ) ;
#14485 = CARTESIAN_POINT ( 'NONE',  ( -11.08653569745421308, 56.26057688450604388, -4.438844214435591518 ) ) ;
#14486 = CARTESIAN_POINT ( 'NONE',  ( -4.808149584360944750, 104.6144662015457527, 0.4147572885131461939 ) ) ;
#14487 = CARTESIAN_POINT ( 'NONE',  ( -4.550674770548566173, 2.667180226961371137, -0.8080508602523945871 ) ) ;
#14488 = FACE_OUTER_BOUND ( 'NONE', #30843, .T. ) ;
#14489 = CARTESIAN_POINT ( 'NONE',  ( -5.277380552522624946, 115.6909491485453003, 0.8071570353046304547 ) ) ;
#14490 = CARTESIAN_POINT ( 'NONE',  ( 3.093634585129180881, -14.37226628243755400, 4.703574289890697813 ) ) ;
#14491 = CARTESIAN_POINT ( 'NONE',  ( 4.257294657327800103, 122.9893884486272526, -0.03029934543357437962 ) ) ;
#14492 = CARTESIAN_POINT ( 'NONE',  ( 0.2644822807012546795, 35.23508677173605719, 3.013287348562808443 ) ) ;
#14493 = CARTESIAN_POINT ( 'NONE',  ( -2.065088524322160612, 115.7028725816649057, 1.634879246183956081 ) ) ;
#14494 = VERTEX_POINT ( 'NONE', #27221 ) ;
#14495 = FACE_OUTER_BOUND ( 'NONE', #7462, .T. ) ;
#14496 = CARTESIAN_POINT ( 'NONE',  ( 2.260827880841108417, -15.68886294521955271, 5.354637041555423416 ) ) ;
#14497 = CARTESIAN_POINT ( 'NONE',  ( -12.76794581240270254, 122.4237789811383550, 1.308419224297318051 ) ) ;
#14498 = CARTESIAN_POINT ( 'NONE',  ( -0.8176680875534481086, 23.83313504737664346, 0.5327793711180701663 ) ) ;
#14499 = ORIENTED_EDGE ( 'NONE', *, *, #39197, .T. ) ;
#14500 = ORIENTED_EDGE ( 'NONE', *, *, #4704, .F. ) ;
#14501 = CARTESIAN_POINT ( 'NONE',  ( -4.469853575504566301, 31.48943071249222214, -0.6923489671027511783 ) ) ;
#14502 = CARTESIAN_POINT ( 'NONE',  ( -0.02647280040265726289, 106.0860833631645193, 5.252669131072540409 ) ) ;
#14503 = SHAPE_REPRESENTATION_RELATIONSHIP ( 'NONE' , 'NONE' ,  #19076, #22381 ) ;
#14504 = CARTESIAN_POINT ( 'NONE',  ( -2.657114488131365970, 120.4390018212493914, 0.3871174720959881244 ) ) ;
#14505 = DIRECTION ( 'NONE',  ( -0.9998004120163609398, 0.000000000000000000, -0.01997839162482749689 ) ) ;
#14506 = EDGE_CURVE ( 'NONE', #25488, #2275, #234, .T. ) ;
#14507 = CARTESIAN_POINT ( 'NONE',  ( 4.623422138725822528, 118.0605935606111672, -0.5413340251631463262 ) ) ;
#14508 = CARTESIAN_POINT ( 'NONE',  ( 2.165411683282626232, 157.1282018749678002, -1.500011447693321065 ) ) ;
#14509 = AXIS2_PLACEMENT_3D ( 'NONE', #2528, #41286, #28063 ) ;
#14510 = CARTESIAN_POINT ( 'NONE',  ( -6.672308397275299896, 157.8130281244853279, -1.874701415657104242 ) ) ;
#14511 = FACE_BOUND ( 'NONE', #13673, .T. ) ;
#14512 = ADVANCED_FACE ( 'NONE', ( #7847 ), #7040, .T. ) ;
#14513 = ORIENTED_EDGE ( 'NONE', *, *, #12874, .T. ) ;
#14514 = CARTESIAN_POINT ( 'NONE',  ( 4.411902438606213117, 118.1805500072961337, -0.3959976634185874422 ) ) ;
#14515 = AXIS2_PLACEMENT_3D ( 'NONE', #8874, #11221, #11640 ) ;
#14516 = CARTESIAN_POINT ( 'NONE',  ( 9.094799215789642233, 123.6795089456687577, -0.2292421281602768091 ) ) ;
#14517 = ORIENTED_EDGE ( 'NONE', *, *, #11052, .F. ) ;
#14518 = CARTESIAN_POINT ( 'NONE',  ( 3.198896590522081862, -14.38863201745455100, 2.123570546440393780 ) ) ;
#14519 = CARTESIAN_POINT ( 'NONE',  ( -4.997723913362575487, 117.4043970260275813, 0.8231665828273773133 ) ) ;
#14520 = VECTOR ( 'NONE', #14786, 1000.000000000000227 ) ;
#14521 = CARTESIAN_POINT ( 'NONE',  ( -58.45640570440981065, -0.4407481023139777632, 0.3169051027096812523 ) ) ;
#14522 = CARTESIAN_POINT ( 'NONE',  ( -4.627572956979934204, -1.171460759993483647, -0.2796867628226345492 ) ) ;
#14523 = CARTESIAN_POINT ( 'NONE',  ( 17.23442203377886628, 146.5563353440282981, 2.056614067264090906 ) ) ;
#14524 = CARTESIAN_POINT ( 'NONE',  ( -1.788360971357598750, 31.32134090374974633, 3.767248576702360907 ) ) ;
#14525 = CARTESIAN_POINT ( 'NONE',  ( -4.753511127315711349, 115.8251506319059843, 1.256829922054842008 ) ) ;
#14526 = B_SPLINE_CURVE_WITH_KNOTS ( 'NONE', 3,
 ( #13356, #7396, #11003, #36792, #20358, #17388 ),
 .UNSPECIFIED., .F., .F.,
 ( 4, 2, 4 ),
 ( 0.0008205648557148674267, 0.001333860798246176271, 0.001847156740777485115 ),
 .UNSPECIFIED. ) ;
#14527 = CARTESIAN_POINT ( 'NONE',  ( 1.068493265602401987, 5.690783753869971484, 4.496582723949734017 ) ) ;
#14528 = CARTESIAN_POINT ( 'NONE',  ( 9.566940353391197860, 124.8108731098830049, 0.2265937611309802591 ) ) ;
#14529 = CARTESIAN_POINT ( 'NONE',  ( -10.63219908769220901, 56.50600268266015291, 5.016499999998452530 ) ) ;
#14530 = CARTESIAN_POINT ( 'NONE',  ( -57.66977034847604955, 1.126272260461025354, -0.8071799157849589568 ) ) ;
#14531 = CARTESIAN_POINT ( 'NONE',  ( -8.781393967084220264, 117.7409677532042735, -0.4282185732264804368 ) ) ;
#14532 = DIRECTION ( 'NONE',  ( 4.017660918040594346E-17, -1.000000000000000000, -2.376309959284834438E-19 ) ) ;
#14533 = CIRCLE ( 'NONE', #7057, 0.2539999999999973390 ) ;
#14534 = DIRECTION ( 'NONE',  ( -0.8745520943968250194, 0.4849315768086532863, -5.361993529360574930E-16 ) ) ;
#14535 = CARTESIAN_POINT ( 'NONE',  ( -0.1058213901578662491, 105.9761915687788587, 5.295735085525936192 ) ) ;
#14536 = DIRECTION ( 'NONE',  ( -0.8745520943968344563, 0.4849315768086362999, -6.829619984160689601E-16 ) ) ;
#14537 = CARTESIAN_POINT ( 'NONE',  ( -8.022552064266685434, 3.315157024569945765, 2.561087356634513590 ) ) ;
#14538 = FACE_OUTER_BOUND ( 'NONE', #30739, .T. ) ;
#14539 = FACE_OUTER_BOUND ( 'NONE', #6992, .T. ) ;
#14540 = CARTESIAN_POINT ( 'NONE',  ( 1.824654213811243819, -15.25386490109567639, 5.420715704377902178 ) ) ;
#14541 = CARTESIAN_POINT ( 'NONE',  ( 0.003708075273124115685, 123.1683257372384901, -0.1855672496570449914 ) ) ;
#14542 = CARTESIAN_POINT ( 'NONE',  ( -0.004913308686094480619, 116.7872217978203224, 0.2458820580207660422 ) ) ;
#14543 = ORIENTED_EDGE ( 'NONE', *, *, #2714, .T. ) ;
#14544 = CARTESIAN_POINT ( 'NONE',  ( -57.66243511465492588, 3.255537196535582378, -0.1194500880619697308 ) ) ;
#14545 = EDGE_LOOP ( 'NONE', ( #29352, #24019, #1029, #23087 ) ) ;
#14546 = DIRECTION ( 'NONE',  ( -9.627370216492862708E-17, -1.000000000000000000, 0.000000000000000000 ) ) ;
#14547 = CARTESIAN_POINT ( 'NONE',  ( -12.85860202769644545, 133.7716054015561156, -0.2569454702854386263 ) ) ;
#14548 = CARTESIAN_POINT ( 'NONE',  ( 5.819126084642364916, -14.14507005385615201, 2.709888076677010371 ) ) ;
#14549 = CARTESIAN_POINT ( 'NONE',  ( -20.91036014055508829, 148.6614476615901594, 1.563091210272363307 ) ) ;
#14550 = AXIS2_PLACEMENT_3D ( 'NONE', #2913, #22460, #15875 ) ;
#14551 = CARTESIAN_POINT ( 'NONE',  ( 22.60445334873316270, 148.5212373274837319, -0.8566365145943198867 ) ) ;
#14552 = CARTESIAN_POINT ( 'NONE',  ( -2.029258473809828711, 23.83235028914373288, 4.157303687431403993 ) ) ;
#14553 = CARTESIAN_POINT ( 'NONE',  ( -8.021187395864899372, 158.6806155330135084, -0.3964977924059485126 ) ) ;
#14554 = CARTESIAN_POINT ( 'NONE',  ( -53.52914546082846670, 10.14270320506335210, -3.905849526455717147 ) ) ;
#14555 = ORIENTED_EDGE ( 'NONE', *, *, #11284, .F. ) ;
#14556 = CARTESIAN_POINT ( 'NONE',  ( 6.059261036834407754, 56.58343591620776891, 4.712961528314683513 ) ) ;
#14557 = CARTESIAN_POINT ( 'NONE',  ( -11.89126842552456509, 124.3826620800890339, 1.187748846906861777 ) ) ;
#14558 = CARTESIAN_POINT ( 'NONE',  ( -51.17288806236419418, 14.15688068541630429, -4.489013846348126613 ) ) ;
#14559 = CARTESIAN_POINT ( 'NONE',  ( 18.94087081963948549, 148.8558894138562039, -1.735487911102014946 ) ) ;
#14560 = TOROIDAL_SURFACE ( 'NONE', #303, 5.080000000000005400, 0.5080000000000000071 ) ;
#14561 = CARTESIAN_POINT ( 'NONE',  ( -6.809904206821648209, 118.2876074772933492, -1.086328812139342848 ) ) ;
#14562 = B_SPLINE_CURVE_WITH_KNOTS ( 'NONE', 5,
 ( #17481, #30478, #14905, #28334, #35155, #18729, #28751, #31739 ),
 .UNSPECIFIED., .F., .F.,
 ( 6, 2, 6 ),
 ( -5.999999999880332237E-08, 0.0004919218780628848613, 0.0009839037561257684989 ),
 .UNSPECIFIED. ) ;
#14563 = CARTESIAN_POINT ( 'NONE',  ( -42.33919149967392315, 22.05006338260229271, -1.842566675324098568 ) ) ;
#14564 = CARTESIAN_POINT ( 'NONE',  ( 2.684237737021673453, 120.5579296053302727, -0.3360084551914348516 ) ) ;
#14565 = ORIENTED_EDGE ( 'NONE', *, *, #30470, .F. ) ;
#14566 = CARTESIAN_POINT ( 'NONE',  ( -18.05261769607656319, 144.6555253171603397, -2.402359405240794832 ) ) ;
#14567 = CARTESIAN_POINT ( 'NONE',  ( 4.028426573186930426, -15.65323953938244017, 3.316845843096514201 ) ) ;
#14568 = AXIS2_PLACEMENT_3D ( 'NONE', #32918, #12682, #13310 ) ;
#14569 = CARTESIAN_POINT ( 'NONE',  ( -4.296542858503126006, 118.2130224152798945, -0.5011208106148314911 ) ) ;
#14570 = CARTESIAN_POINT ( 'NONE',  ( -56.78650302187183740, 3.241477563879227475, -2.205756828360271093 ) ) ;
#14571 = LINE ( 'NONE', #25008, #40201 ) ;
#14572 = CARTESIAN_POINT ( 'NONE',  ( 10.13131171838191413, 122.2967958330617648, 1.512676856611740783 ) ) ;
#14573 = CARTESIAN_POINT ( 'NONE',  ( 3.682264917456192777, 82.13546620154573930, 0.07358041635423970273 ) ) ;
#14574 = CARTESIAN_POINT ( 'NONE',  ( 0.2965531742115425917, 116.4333835968663919, -0.03207532894271091645 ) ) ;
#14575 = CARTESIAN_POINT ( 'NONE',  ( 3.113543590025587005, -0.1312883392403825233, -7.836836066719057747 ) ) ;
#14576 = CARTESIAN_POINT ( 'NONE',  ( 11.46436990449499760, 128.2561452373498980, 0.7395913538610451310 ) ) ;
#14577 = CARTESIAN_POINT ( 'NONE',  ( 3.879144173866336143, 118.0219252979734677, -0.8163251714509417445 ) ) ;
#14578 = FACE_OUTER_BOUND ( 'NONE', #10313, .T. ) ;
#14579 = CARTESIAN_POINT ( 'NONE',  ( 1.176010826768138173, 105.9617161350778787, -5.207309035134176867 ) ) ;
#14580 = CARTESIAN_POINT ( 'NONE',  ( -8.060487153020286399, 121.1729579957945901, -1.292971159565753148 ) ) ;
#14581 = CARTESIAN_POINT ( 'NONE',  ( -57.60038635073813396, 1.097546858218847898, 0.08229580080364437555 ) ) ;
#14582 = CARTESIAN_POINT ( 'NONE',  ( -14.84180086987441172, 120.3134675335783754, -0.1939203138368897072 ) ) ;
#14583 = ORIENTED_EDGE ( 'NONE', *, *, #33678, .F. ) ;
#14584 = CARTESIAN_POINT ( 'NONE',  ( -47.29848140234559395, 25.70219632838243484, -9.636386808203001053E-15 ) ) ;
#14585 = CARTESIAN_POINT ( 'NONE',  ( 6.878842811470913254, 121.5723321815868871, -0.4547243280587507375 ) ) ;
#14586 = CARTESIAN_POINT ( 'NONE',  ( -7.819596425554085073, 122.5025573185424435, 0.1851470016872596713 ) ) ;
#14587 = ORIENTED_EDGE ( 'NONE', *, *, #24172, .F. ) ;
#14588 = CARTESIAN_POINT ( 'NONE',  ( 0.4158179766845868097, 118.7629491485454025, -1.264088747447795980 ) ) ;
#14589 = CARTESIAN_POINT ( 'NONE',  ( -9.737435037572492291, 124.8671652961716489, -0.4371131421146304818 ) ) ;
#14590 = CARTESIAN_POINT ( 'NONE',  ( 2.601617458372238900, -15.08031326607275879, 5.801161347629554044 ) ) ;
#14591 = CARTESIAN_POINT ( 'NONE',  ( -12.29982474031040596, 156.6574886424908470, 1.289654987246354079 ) ) ;
#14592 = CARTESIAN_POINT ( 'NONE',  ( 5.600204413206903986, 78.91171765783749947, -5.075433163388857416 ) ) ;
#14593 = CARTESIAN_POINT ( 'NONE',  ( 16.10347893962645216, 121.2391669109744186, 0.4275719782727096518 ) ) ;
#14594 = CARTESIAN_POINT ( 'NONE',  ( 7.544955551308853536, 122.4259255053487436, 0.1906877313379402028 ) ) ;
#14595 = ORIENTED_EDGE ( 'NONE', *, *, #39114, .F. ) ;
#14596 = CARTESIAN_POINT ( 'NONE',  ( 0.9036657058557058253, 17.56215383894848614, 0.3677562154327245758 ) ) ;
#14597 = CARTESIAN_POINT ( 'NONE',  ( -15.54780490071038024, 120.7212560704218589, -0.3275748350740994019 ) ) ;
#14598 = CARTESIAN_POINT ( 'NONE',  ( -45.77009211284281776, 21.09669927562158165, -4.287731556584716941 ) ) ;
#14599 = EDGE_CURVE ( 'NONE', #34680, #16326, #37607, .T. ) ;
#14600 = ORIENTED_EDGE ( 'NONE', *, *, #41193, .F. ) ;
#14601 = DIRECTION ( 'NONE',  ( -5.188838149069471174E-16, 1.699382548006136313E-16, 1.000000000000000000 ) ) ;
#14602 = ORIENTED_EDGE ( 'NONE', *, *, #37416, .F. ) ;
#14603 = CARTESIAN_POINT ( 'NONE',  ( 8.390685855369055091, 119.5507258284018093, 1.408871319322181792 ) ) ;
#14604 = CARTESIAN_POINT ( 'NONE',  ( 3.174366308151880034, 97.37546620154573418, 0.06343139340882766875 ) ) ;
#14605 = CARTESIAN_POINT ( 'NONE',  ( 2.957233306982478105, 159.1263692740743068, 1.212116333074086283 ) ) ;
#14606 = CARTESIAN_POINT ( 'NONE',  ( -58.54549369845722850, -0.1193337916018388789, -0.6006683616744088461 ) ) ;
#14607 = CARTESIAN_POINT ( 'NONE',  ( 17.80465198604232313, 131.6735282812448986, -1.559227381006986990 ) ) ;
#14608 = CARTESIAN_POINT ( 'NONE',  ( -8.365627035046871995, 27.56796056798338057, -1.282220400777004388 ) ) ;
#14609 = CARTESIAN_POINT ( 'NONE',  ( -3.104962560943469896, 159.3365417412370562, -0.8543937160244109430 ) ) ;
#14610 = CARTESIAN_POINT ( 'NONE',  ( 4.942462214789340891, 117.6285031199090412, -0.7735160008196966253 ) ) ;
#14611 = EDGE_CURVE ( 'NONE', #21468, #27342, #19937, .T. ) ;
#14612 = EDGE_LOOP ( 'NONE', ( #18673, #41522, #16768, #9442, #26471 ) ) ;
#14613 = CARTESIAN_POINT ( 'NONE',  ( -0.003550340867792285433, 156.3099534201614631, 0.1776735749810083032 ) ) ;
#14614 = CARTESIAN_POINT ( 'NONE',  ( 4.127870218248371970, -15.50624122109489633, 4.747786349039386344 ) ) ;
#14615 = LINE ( 'NONE', #34032, #39719 ) ;
#14616 = CARTESIAN_POINT ( 'NONE',  ( -0.3814255583757257817, 118.1651003383654768, -0.8943798372417751663 ) ) ;
#14617 = ADVANCED_FACE ( 'NONE', ( #12292 ), #27843, .F. ) ;
#14618 = VERTEX_POINT ( 'NONE', #15479 ) ;
#14619 = B_SPLINE_SURFACE_WITH_KNOTS ( 'NONE', 3, 3, ( 
 ( #14683, #5137, #18088, #31093, #14892 ),
 ( #27894, #40902, #3179, #15731, #32145 ),
 ( #28736, #6375, #35345, #38750, #32558 ),
 ( #35765, #22315, #16143, #15529, #8942 ),
 ( #29145, #12958, #18716, #28533, #21907 ),
 ( #2570, #6582, #2775, #19141, #2977 ),
 ( #9155, #35559, #12132, #34937, #12550 ),
 ( #5763, #19548, #31725, #25540, #41539 ),
 ( #19345, #25741, #12346, #18929, #32352 ),
 ( #15314, #41954, #28319, #41329, #25123 ),
 ( #38125, #41749, #25335, #25952, #9770 ),
 ( #15941, #38959, #22734, #38541, #6172 ),
 ( #28936, #9356, #38337, #12755, #22112 ),
 ( #35141, #5968, #31939, #22318, #9559 ),
 ( #22530, #23157, #13389, #16791, #1048 ),
 ( #3611, #14011, #27018, #36823, #26809 ),
 ( #7641, #10610, #7433, #39385, #23803 ),
 ( #10820, #20600, #9975, #36193, #26376 ),
 ( #40027, #3393, #16574, #16359, #39600 ),
 ( #7014, #29365, #32781, #13811, #23592 ),
 ( #29792, #39817, #36614, #20391, #13601 ),
 ( #29585, #419, #13179, #26591, #204 ),
 ( #26166, #33417, #4248, #10187, #10403 ),
 ( #39168, #19759, #19982, #33211, #32999 ),
 ( #631, #23375, #17210, #3827, #36408 ),
 ( #7226, #30208, #20185, #4036, #22949 ),
 ( #35975, #16997, #6792, #29997, #836 ),
 ( #15426, #9262, #1467, #12454, #18829 ),
 ( #33837, #27225, #15213, #22017, #31834 ),
 ( #4665, #40238, #1261, #20811, #25448 ),
 ( #34046, #31625, #28427, #8839, #38446 ),
 ( #31410, #41435, #24014, #33631, #11033 ),
 ( #37033, #7850, #25232, #2463, #17622 ),
 ( #38236, #4459, #17416, #18619, #30413 ),
 ( #14216, #2251, #30624, #21023, #14424 ),
 ( #28635, #2673, #27431, #40445, #11237 ),
 ( #24221, #12240, #37232, #41222, #9052 ),
 ( #35046, #5867, #28215, #41647, #8050 ),
 ( #21802, #15631, #4876, #18403, #12024 ) ),
 .UNSPECIFIED., .F., .F., .F.,
 ( 4, 1, 1, 1, 1, 1, 1, 1, 1, 1, 1, 2, 1, 1, 1, 1, 1, 1, 1, 1, 1, 1, 1, 1, 1, 1, 1, 1, 1, 1, 1, 1, 1, 1, 1, 4 ),
 ( 4, 1, 4 ),
 ( 0.000000000000000000, 0.01653533301974152367, 0.03307066603948304734, 0.04960599905922460223, 0.06614133207896609468, 0.08267666509870763569, 0.09921199811844919059, 0.1322826641579321894, 0.1653533301974152714, 0.1984239962368983812, 0.2314946622763813522, 0.2645653283158643787, 0.3105299952961229071, 0.3335123287862520880, 0.3564946622763812689, 0.4024593292566397418, 0.4484239962368982702, 0.4943886632171566875, 0.5403533301974150493, 0.5863179971776735222, 0.6322826641579321061, 0.6782473311381906900, 0.7242119981184491628, 0.7701766650987074136, 0.8161413320789658865, 0.8621059990592241373, 0.8735971658042887000, 0.8850883325493537068, 0.8965794992944182695, 0.9080706660394826102, 0.9195618327845473949, 0.9310529995296121797, 0.9425441662746769644, 0.9540353330197415271, 0.9770176665098706525, 1.000000000000000000 ),
 ( 0.000000000000000000, 0.5000000000000000000, 1.000000000000000000 ),
 .UNSPECIFIED. ) ;
#14620 = CARTESIAN_POINT ( 'NONE',  ( 0.9722352627952559612, 157.7941190989783991, 1.644571785473256220 ) ) ;
#14621 = DIRECTION ( 'NONE',  ( 0.9998004120163608288, 0.000000000000000000, 0.01997839162482749342 ) ) ;
#14622 = DIRECTION ( 'NONE',  ( 0.3256999990547780333, 0.9454731675810359448, 8.328397965203031669E-18 ) ) ;
#14623 = CARTESIAN_POINT ( 'NONE',  ( -1.626581124784322929, 119.3928400758114918, 0.6183738137425960346 ) ) ;
#14624 = CARTESIAN_POINT ( 'NONE',  ( 6.022233187337456606, 12.22246943312702427, 5.887876567768997482 ) ) ;
#14625 = CARTESIAN_POINT ( 'NONE',  ( 8.219871311007414860, 154.6505398758502849, 1.119353551822957149 ) ) ;
#14626 = FACE_OUTER_BOUND ( 'NONE', #14612, .T. ) ;
#14627 = PRESENTATION_LAYER_ASSIGNMENT (  '', '', ( #41885 ) ) ;
#14628 = CARTESIAN_POINT ( 'NONE',  ( 15.52406334459478465, 121.0440340969820596, -0.2084667659489262137 ) ) ;
#14629 = EDGE_CURVE ( 'NONE', #2316, #41065, #8473, .T. ) ;
#14630 = DIRECTION ( 'NONE',  ( -5.206863593109713661E-17, 1.000000000000000000, -1.077750396879097183E-30 ) ) ;
#14631 = CARTESIAN_POINT ( 'NONE',  ( -57.68540670336199128, 1.184946625668306330, 1.219309026451214306 ) ) ;
#14632 = CARTESIAN_POINT ( 'NONE',  ( -54.22048251907422411, 8.823772151126235030, 3.634456437801601325 ) ) ;
#14633 = EDGE_CURVE ( 'NONE', #27648, #19349, #29464, .T. ) ;
#14634 = CARTESIAN_POINT ( 'NONE',  ( 2.071654280177505303, -15.34349575202162974, 5.977339193430268871 ) ) ;
#14635 = CARTESIAN_POINT ( 'NONE',  ( -4.313832278175046220, 118.2128970912768438, 0.3282138498878479638 ) ) ;
#14636 = ORIENTED_EDGE ( 'NONE', *, *, #20675, .F. ) ;
#14637 = CARTESIAN_POINT ( 'NONE',  ( -49.13940628111213016, 17.59503125033257120, 5.062072503518671773 ) ) ;
#14638 = EDGE_CURVE ( 'NONE', #32933, #29748, #41696, .T. ) ;
#14639 = CARTESIAN_POINT ( 'NONE',  ( 6.198907113810094849, 119.6457338356565430, -1.000577012762424944 ) ) ;
#14640 = CARTESIAN_POINT ( 'NONE',  ( -6.937169949972989080, 121.8132169909553966, -0.2949249740950673493 ) ) ;
#14641 = CARTESIAN_POINT ( 'NONE',  ( 4.252925440392405498, 118.2240520237851626, 0.4605658090341683275 ) ) ;
#14642 = CARTESIAN_POINT ( 'NONE',  ( -3.037839899926094489, 156.1243923452879017, -0.6481072647156851385 ) ) ;
#14643 = CARTESIAN_POINT ( 'NONE',  ( -28.95189557068615116, 64.41341631820179714, 1.523999999999993582 ) ) ;
#14644 = FACE_OUTER_BOUND ( 'NONE', #14920, .T. ) ;
#14645 = ORIENTED_EDGE ( 'NONE', *, *, #8517, .T. ) ;
#14646 = CARTESIAN_POINT ( 'NONE',  ( -1.932895124392534303, 20.38400505531995321, -4.219463811995566083 ) ) ;
#14647 = CARTESIAN_POINT ( 'NONE',  ( -16.29178962149237009, 143.9496486471311698, -1.781768755694404849 ) ) ;
#14648 = DIRECTION ( 'NONE',  ( -0.8745520943968244643, 0.4849315768086544520, -4.268512490100399076E-16 ) ) ;
#14649 = CARTESIAN_POINT ( 'NONE',  ( -3.148524768479886937, 30.89467502894792972, -0.4672404312464801812 ) ) ;
#14650 = DIRECTION ( 'NONE',  ( 5.463695987328526437E-16, -1.000000000000000000, -1.672774450599033775E-31 ) ) ;
#14651 = CARTESIAN_POINT ( 'NONE',  ( 6.989538638170239793, 121.9084849004810138, 0.3647075761099029534 ) ) ;
#14652 = DIRECTION ( 'NONE',  ( -0.01997839162482761832, -1.040247600000950455E-18, 0.9998004120163610509 ) ) ;
#14653 = CARTESIAN_POINT ( 'NONE',  ( 22.71086789718616572, 148.5871737753741115, 1.637050152828072314 ) ) ;
#14654 = LINE ( 'NONE', #17438, #17797 ) ;
#14656 = CARTESIAN_POINT ( 'NONE',  ( 5.066682439019537298, 158.5910778905036977, -1.349075717862105561 ) ) ;
#14655 = CARTESIAN_POINT ( 'NONE',  ( 3.117629155811438402, -14.23119940253145188, 1.544136867890079090 ) ) ;
#14657 = CARTESIAN_POINT ( 'NONE',  ( -6.663576545388717243, 119.9895581359321994, 0.9799952387295398637 ) ) ;
#14658 = CARTESIAN_POINT ( 'NONE',  ( -0.6014681082635296994, -0.5174402789662015945, 0.7683055774679631300 ) ) ;
#14659 = CARTESIAN_POINT ( 'NONE',  ( -22.23561040172140579, 150.7043692363948537, -1.289434558007279685 ) ) ;
#14660 = CARTESIAN_POINT ( 'NONE',  ( -0.7801697309092696653, 18.27050645547500451, 0.5824522774875325881 ) ) ;
#14661 = ORIENTED_EDGE ( 'NONE', *, *, #22509, .T. ) ;
#14662 = CARTESIAN_POINT ( 'NONE',  ( -51.32320689156235005, 13.70825103427969438, 4.126761985266667487 ) ) ;
#14663 = CIRCLE ( 'NONE', #26936, 6.349999999999999645 ) ;
#14664 = CARTESIAN_POINT ( 'NONE',  ( -9.384706802269613846, 123.8909350679826815, 0.3250447036211730478 ) ) ;
#14665 = CARTESIAN_POINT ( 'NONE',  ( 3.194768752100229925, -14.65262985833884457, 5.377959301279905624 ) ) ;
#14666 = CARTESIAN_POINT ( 'NONE',  ( 0.008945177887880035456, 119.9096241394016715, -0.4476532798976761707 ) ) ;
#14667 = ORIENTED_EDGE ( 'NONE', *, *, #37313, .F. ) ;
#14668 = CARTESIAN_POINT ( 'NONE',  ( 0.3866447666624587276, 115.7034473292545584, 1.763797082902897495 ) ) ;
#14669 = ORIENTED_EDGE ( 'NONE', *, *, #20953, .F. ) ;
#14670 = CARTESIAN_POINT ( 'NONE',  ( 3.154677723130417277, -14.38507846778283650, 3.622984934187011952 ) ) ;
#14671 = CARTESIAN_POINT ( 'NONE',  ( -4.760401155226894332, 117.7660915045744190, -1.056044474819750834 ) ) ;
#14672 = CARTESIAN_POINT ( 'NONE',  ( 9.614588335866148583, 124.8310256250372277, 0.1039111448415540317 ) ) ;
#14673 = ORIENTED_EDGE ( 'NONE', *, *, #23185, .F. ) ;
#14674 = CARTESIAN_POINT ( 'NONE',  ( 20.31017440411229202, 148.4497675966422889, 2.477828910454907607 ) ) ;
#14675 = CARTESIAN_POINT ( 'NONE',  ( 13.85159022459153988, 59.63164443796365077, -5.016499999999999737 ) ) ;
#14676 = DIRECTION ( 'NONE',  ( -0.000000000000000000, 0.000000000000000000, -1.000000000000000000 ) ) ;
#14677 = CARTESIAN_POINT ( 'NONE',  ( 0.01341678693497577735, 156.4123495908283985, -0.6714308817992609146 ) ) ;
#14678 = ADVANCED_FACE ( 'NONE', ( #37648 ), #18668, .F. ) ;
#14679 = CARTESIAN_POINT ( 'NONE',  ( 22.59814275696091812, 137.2245694613254443, 0.1355511068837784994 ) ) ;
#14680 = ADVANCED_FACE ( 'NONE', ( #38070 ), #13608, .T. ) ;
#14681 = DIRECTION ( 'NONE',  ( 0.9816537812491107351, 0.1906721105964981344, -6.949828216605166964E-15 ) ) ;
#14682 = CARTESIAN_POINT ( 'NONE',  ( 2.099639488158107081, -15.34085824818334842, 5.967397557607278635 ) ) ;
#14683 = CARTESIAN_POINT ( 'NONE',  ( -41.05189575270516400, 23.09451173561986081, 1.523999999999992472 ) ) ;
#14684 = CARTESIAN_POINT ( 'NONE',  ( -4.957032329879782040, 117.5911933634104543, -0.8969954988694857079 ) ) ;
#14685 = CARTESIAN_POINT ( 'NONE',  ( -4.623803002916879734, 117.9758317316280198, 0.7387004689016926084 ) ) ;
#14686 = AXIS2_PLACEMENT_3D ( 'NONE', #6477, #29046, #32461 ) ;
#14687 = VERTEX_POINT ( 'NONE', #39335 ) ;
#14688 = CARTESIAN_POINT ( 'NONE',  ( 4.854633716284414646, 115.7029491485453292, -1.279498648767039448 ) ) ;
#14689 = EDGE_CURVE ( 'NONE', #29613, #11330, #29414, .T. ) ;
#14690 = CARTESIAN_POINT ( 'NONE',  ( 5.606335446380697363, 118.1214203281341781, -0.9042019091217482485 ) ) ;
#14691 = CARTESIAN_POINT ( 'NONE',  ( -2.486440349385922843, 120.2382744777187611, -0.5044468955786924891 ) ) ;
#14692 = CARTESIAN_POINT ( 'NONE',  ( 4.830107420232238269, 117.5457777486666089, 1.145229895618746774 ) ) ;
#14693 = CARTESIAN_POINT ( 'NONE',  ( -12.21488373879589062, 55.24499999999998323, -5.016499999999999737 ) ) ;
#14694 = CARTESIAN_POINT ( 'NONE',  ( -0.1065646865916158176, 105.8844662015456919, 5.332932678536313809 ) ) ;
#14695 = CARTESIAN_POINT ( 'NONE',  ( 4.326043401919948295, 8.289558097378858292, -1.648119079657388353 ) ) ;
#14696 = ADVANCED_FACE ( 'NONE', ( #19299 ), #19935, .T. ) ;
#14697 = DIRECTION ( 'NONE',  ( -0.8745520943968243532, 0.4849315768086547296, -6.829619984160642269E-16 ) ) ;
#14698 = CARTESIAN_POINT ( 'NONE',  ( -0.4455429663221430192, 105.8200183450921941, -5.321466673365036648 ) ) ;
#14699 = CARTESIAN_POINT ( 'NONE',  ( 3.944052607038018632, -12.86033490357471543, 2.408110524499547100 ) ) ;
#14700 = CARTESIAN_POINT ( 'NONE',  ( 5.282628607151995226, 116.7267603939287426, -0.8077565746219077525 ) ) ;
#14701 = CARTESIAN_POINT ( 'NONE',  ( -3.938977128594350230, 28.07268674286775578, 0.7495841607770368231 ) ) ;
#14702 = CARTESIAN_POINT ( 'NONE',  ( -2.050006216300763739, 115.7029491482434622, 1.635993916937294568 ) ) ;
#14703 = CARTESIAN_POINT ( 'NONE',  ( -1.287880193524239658, 20.15907059199006923, -4.440276399826991849 ) ) ;
#14704 = ORIENTED_EDGE ( 'NONE', *, *, #7896, .F. ) ;
#14705 = CARTESIAN_POINT ( 'NONE',  ( -4.835487464103170652, 104.6144662015457527, 0.09712566206071873709 ) ) ;
#14706 = CARTESIAN_POINT ( 'NONE',  ( 3.179180861052679052, -15.64967171142420099, 4.365151252316144870 ) ) ;
#14707 = CARTESIAN_POINT ( 'NONE',  ( -1.263959281924281752, 118.7146927282448132, 0.6429003683496403720 ) ) ;
#14708 = EDGE_CURVE ( 'NONE', #26023, #33608, #22274, .T. ) ;
#14709 = CARTESIAN_POINT ( 'NONE',  ( -0.9756124605737610533, 22.95965383878278843, 0.006055453616918176837 ) ) ;
#14710 = EDGE_LOOP ( 'NONE', ( #39754, #15436, #39640 ) ) ;
#14711 = ORIENTED_EDGE ( 'NONE', *, *, #14926, .F. ) ;
#14712 = CARTESIAN_POINT ( 'NONE',  ( -6.707568152035292797E-14, 117.3144662015457271, 2.632902133564923224E-18 ) ) ;
#14713 = CARTESIAN_POINT ( 'NONE',  ( 4.134812325681913592, 122.5143120247930142, 0.2378952825278687622 ) ) ;
#14714 = FILL_AREA_STYLE ('',( #1755 ) ) ;
#14715 = CARTESIAN_POINT ( 'NONE',  ( -1.496072496114464911, 120.3785564700922492, 0.3614901595391031286 ) ) ;
#14716 = DIRECTION ( 'NONE',  ( 0.7071067811865483499, -0.7071067811865465735, 0.000000000000000000 ) ) ;
#14717 =( BOUNDED_CURVE ( )  B_SPLINE_CURVE ( 3, ( #16545, #23126, #14187, #7197 ),
 .UNSPECIFIED., .F., .T. ) 
 B_SPLINE_CURVE_WITH_KNOTS ( ( 4, 4 ),
 ( 1.570796326794895670, 2.532278806861539611 ),
 .UNSPECIFIED. ) 
 CURVE ( )  GEOMETRIC_REPRESENTATION_ITEM ( )  RATIONAL_B_SPLINE_CURVE ( ( 1.000000000000000000, 0.9244349266169025192, 0.9244349266169025192, 1.000000000000000000 ) ) 
 REPRESENTATION_ITEM ( '' )  );
#14718 = CARTESIAN_POINT ( 'NONE',  ( 4.590055535865089631, 118.0156062071498297, -0.6989146611030767620 ) ) ;
#14719 = CARTESIAN_POINT ( 'NONE',  ( 0.9532528233479417024, 157.3234082283764792, -1.521469375400507307 ) ) ;
#14720 = CARTESIAN_POINT ( 'NONE',  ( -18.81387422072304361, 135.8679125664981484, -2.390408806419126009 ) ) ;
#14721 = CARTESIAN_POINT ( 'NONE',  ( -18.32410244842765934, 17.14500000000000313, 0.000000000000000000 ) ) ;
#14722 = VECTOR ( 'NONE', #40466, 1000.000000000000000 ) ;
#14723 = CARTESIAN_POINT ( 'NONE',  ( 4.115781193554201245, 118.2429491485453354, -0.1890479318226853389 ) ) ;
#14724 = CARTESIAN_POINT ( 'NONE',  ( 9.339416610757361070, 123.9819092696984910, -0.2335442159362872416 ) ) ;
#14725 = AXIS2_PLACEMENT_3D ( 'NONE', #35245, #3290, #29472 ) ;
#14726 = ORIENTED_EDGE ( 'NONE', *, *, #12028, .T. ) ;
#14727 = CARTESIAN_POINT ( 'NONE',  ( 3.205116352530840373, -14.62692654125133451, 3.000134484400556190 ) ) ;
#14728 = CARTESIAN_POINT ( 'NONE',  ( 4.942575927434568861, 117.5943726187274194, 0.9708222732221650775 ) ) ;
#14729 = CARTESIAN_POINT ( 'NONE',  ( -58.54486130997005233, -0.6084878433727288760, 0.2286541811371931576 ) ) ;
#14730 = CARTESIAN_POINT ( 'NONE',  ( -1.722957355399680202, -2.895624787512894649, -4.295268622497145472 ) ) ;
#14731 = CARTESIAN_POINT ( 'NONE',  ( 17.21112184089930963, 146.3482411845097886, 2.056990446313781362 ) ) ;
#14732 = CARTESIAN_POINT ( 'NONE',  ( 0.9496290232869858405, 34.46945342146898383, 2.665853779434302684 ) ) ;
#14733 = CARTESIAN_POINT ( 'NONE',  ( -3.998592866256331035, 116.4303826247378026, 1.177299868075282641 ) ) ;
#14734 = AXIS2_PLACEMENT_3D ( 'NONE', #23675, #13897, #17299 ) ;
#14735 = CARTESIAN_POINT ( 'NONE',  ( -4.476207883417873568, -7.053342675672244155, -1.178223045331058705 ) ) ;
#14736 = CARTESIAN_POINT ( 'NONE',  ( 5.939593986634037925, 121.5467800236367424, 0.1471147542197156211 ) ) ;
#14737 = CARTESIAN_POINT ( 'NONE',  ( 7.154006291674216200, 2.952895779142483246, 4.500751621275830061 ) ) ;
#14738 = CARTESIAN_POINT ( 'NONE',  ( -57.53554607470949378, 1.398951746849091959, -0.8928682508385608063 ) ) ;
#14739 = CARTESIAN_POINT ( 'NONE',  ( -8.771200022011038655, 117.7827218713625115, -0.5098789378553986174 ) ) ;
#14740 = VECTOR ( 'NONE', #10599, 1000.000000000000000 ) ;
#14741 = CARTESIAN_POINT ( 'NONE',  ( 17.14499999999999957, 71.11999999999999034, -5.016499999999999737 ) ) ;
#14742 = LINE ( 'NONE', #5821, #35528 ) ;
#14743 = CARTESIAN_POINT ( 'NONE',  ( -17.31000046771894318, 62.32679794340116786, -1.269999999999999352 ) ) ;
#14744 = CARTESIAN_POINT ( 'NONE',  ( -5.871471797037544071, 31.01275966357848901, 2.875548327037550589 ) ) ;
#14745 = CARTESIAN_POINT ( 'NONE',  ( 6.515560366292186600, -0.8950661730705262720, -5.416678580889517924 ) ) ;
#14746 = EDGE_CURVE ( 'NONE', #13325, #10933, #29537, .T. ) ;
#14747 = CARTESIAN_POINT ( 'NONE',  ( 1.940878836488825643, 118.1588881878910939, 0.8639920667537415166 ) ) ;
#14748 = DIRECTION ( 'NONE',  ( 5.188838149069472160E-16, -1.699382548006136559E-16, -1.000000000000000000 ) ) ;
#14749 = CARTESIAN_POINT ( 'NONE',  ( -58.83227707057485389, -0.08366279997994163775, -1.544404338758123352E-14 ) ) ;
#14750 = CARTESIAN_POINT ( 'NONE',  ( -58.83227707057486811, -0.08366279997995551554, -1.995625700055530397E-14 ) ) ;
#14751 = CARTESIAN_POINT ( 'NONE',  ( -3.811114225546910816, 116.8316721669309572, 0.2429903670874780930 ) ) ;
#14752 = AXIS2_PLACEMENT_3D ( 'NONE', #11978, #8158, #25187 ) ;
#14753 = VERTEX_POINT ( 'NONE', #15891 ) ;
#14754 = DIRECTION ( 'NONE',  ( -0.8745520943968250194, 0.4849315768086532863, -5.361993529360574930E-16 ) ) ;
#14755 = ORIENTED_EDGE ( 'NONE', *, *, #6452, .F. ) ;
#14756 = CARTESIAN_POINT ( 'NONE',  ( -43.44488126592453625, 21.78892034651219944, -2.392822157540683836 ) ) ;
#14757 = CARTESIAN_POINT ( 'NONE',  ( -5.318614220644641399, 121.3518964346359468, -0.06992023047444935469 ) ) ;
#14758 = CARTESIAN_POINT ( 'NONE',  ( 3.388119949408427978, -15.58183483456807039, 5.324763925812813881 ) ) ;
#14759 = CARTESIAN_POINT ( 'NONE',  ( -0.4390033025491983376, 118.1045761740670201, 0.5613618447453817550 ) ) ;
#14760 = CARTESIAN_POINT ( 'NONE',  ( 3.102616959202278757, 159.2904672602661549, -0.8345756338990467649 ) ) ;
#14761 = CARTESIAN_POINT ( 'NONE',  ( 2.584458374606236841, 15.83607344512877368, 3.832284875798456447 ) ) ;
#14762 = CARTESIAN_POINT ( 'NONE',  ( -9.754222058523323469, 118.0373187826741486, -0.4689489433136687646 ) ) ;
#14763 = CARTESIAN_POINT ( 'NONE',  ( -50.28518799591763866, 15.83636413734068249, -4.862251023740228995 ) ) ;
#14764 = CARTESIAN_POINT ( 'NONE',  ( -8.796213517692432760, 117.7094638964744320, -0.009884658790045439819 ) ) ;
#14765 = CARTESIAN_POINT ( 'NONE',  ( -10.93398011767285460, 82.89560043784887000, 1.269999999999999574 ) ) ;
#14766 = CARTESIAN_POINT ( 'NONE',  ( -3.718565865972091267, 156.7231754051992425, 1.451222330515915093 ) ) ;
#14767 = CARTESIAN_POINT ( 'NONE',  ( -53.66072396849355641, 9.491867573702387872, -3.600208096711306816 ) ) ;
#14768 = CARTESIAN_POINT ( 'NONE',  ( 1.305241956589648034, 119.0230276286704054, -0.6306560096549495009 ) ) ;
#14769 = CARTESIAN_POINT ( 'NONE',  ( -13.68454576465616590, 121.6032371815301900, -1.618700059879337072 ) ) ;
#14770 = CARTESIAN_POINT ( 'NONE',  ( -47.35944255389382107, 21.37623662739424191, -4.722871667523179440 ) ) ;
#14771 = AXIS2_PLACEMENT_3D ( 'NONE', #6931, #36738, #26934 ) ;
#14772 = B_SPLINE_CURVE_WITH_KNOTS ( 'NONE', 5,
 ( #36448, #40285, #11077, #5332, #41106, #27679, #5538, #24686 ),
 .UNSPECIFIED., .F., .F.,
 ( 6, 2, 6 ),
 ( 0.000000000000000000, 0.0004921095964230306607, 0.0009842191928460613214 ),
 .UNSPECIFIED. ) ;
#14773 = CARTESIAN_POINT ( 'NONE',  ( 0.005430166084257035536, 120.5648899400503069, -0.2717477157510631014 ) ) ;
#14774 = EDGE_LOOP ( 'NONE', ( #4737, #15848, #5162, #15777 ) ) ;
#14775 = CARTESIAN_POINT ( 'NONE',  ( -12.61679319894190598, 153.7453525671159298, -2.178569956567484756 ) ) ;
#14776 = CARTESIAN_POINT ( 'NONE',  ( 3.308369008328103433, -15.71782228035249673, 4.479361047165574483 ) ) ;
#14777 = CARTESIAN_POINT ( 'NONE',  ( -4.439283198886601944, 118.1598961654773632, -0.6091820576028420531 ) ) ;
#14778 = CARTESIAN_POINT ( 'NONE',  ( -57.83637253161431602, 2.237724655402451024, -1.757929103219309397 ) ) ;
#14779 = VECTOR ( 'NONE', #41609, 1000.000000000000114 ) ;
#14780 = DIRECTION ( 'NONE',  ( -0.8745520943968245753, 0.4849315768086539524, -5.691349986800526185E-16 ) ) ;
#14781 = CARTESIAN_POINT ( 'NONE',  ( 11.36144155339839656, 123.3954635094115702, 1.633191427152098418 ) ) ;
#14782 = FACE_OUTER_BOUND ( 'NONE', #35086, .T. ) ;
#14783 = CARTESIAN_POINT ( 'NONE',  ( 2.068261358883969780, 0.06400946394871305511, -8.190863557276260920 ) ) ;
#14784 = CARTESIAN_POINT ( 'NONE',  ( 13.22128265123318691, 134.0707761029912035, 0.8398552229569322680 ) ) ;
#14785 = CARTESIAN_POINT ( 'NONE',  ( -56.80697847991661575, 4.636179106009441497, -2.484889565616585472 ) ) ;
#14787 = ORIENTED_EDGE ( 'NONE', *, *, #1891, .F. ) ;
#14786 = DIRECTION ( 'NONE',  ( -0.4849315768086534528, -0.8745520943968250194, -1.030032898892974942E-16 ) ) ;
#14788 = CARTESIAN_POINT ( 'NONE',  ( 3.104280510418153671, 107.6125246504606281, -4.328335581088759376 ) ) ;
#14789 = CARTESIAN_POINT ( 'NONE',  ( 1.060420246909465236, 118.7629491485454025, 1.261316868433438376 ) ) ;
#14790 = AXIS2_PLACEMENT_3D ( 'NONE', #6050, #38211, #19012 ) ;
#14791 = CARTESIAN_POINT ( 'NONE',  ( -57.48728866487982714, 1.341405240446180702, 0.2210608495301386867 ) ) ;
#14792 = CARTESIAN_POINT ( 'NONE',  ( -48.56815661899839398, 19.24492339269599839, 5.224590812749970503 ) ) ;
#14793 = CARTESIAN_POINT ( 'NONE',  ( -22.53108783561251371, 150.7873321363286152, -0.2974592429706744423 ) ) ;
#14794 = ORIENTED_EDGE ( 'NONE', *, *, #8763, .T. ) ;
#14795 = CARTESIAN_POINT ( 'NONE',  ( -48.81380759447691275, 19.38479668107215304, -4.754960688114476142 ) ) ;
#14796 = CARTESIAN_POINT ( 'NONE',  ( -7.846638837763108221, 122.2680111424683957, -0.7500643504151511820 ) ) ;
#14797 = CARTESIAN_POINT ( 'NONE',  ( -7.991391493690929160, 121.7106681566311579, 0.7744224044266007079 ) ) ;
#14798 = ORIENTED_EDGE ( 'NONE', *, *, #14466, .F. ) ;
#14799 = CARTESIAN_POINT ( 'NONE',  ( 2.253168137283801276, 115.6909491485452577, -1.622715864987487544 ) ) ;
#14800 = CARTESIAN_POINT ( 'NONE',  ( -1.586003330670630485, 156.2604006213118453, -0.2328413704193781908 ) ) ;
#14801 = CARTESIAN_POINT ( 'NONE',  ( 2.771648496353774860, -15.01054376081380148, 5.729243832102374867 ) ) ;
#14802 = CARTESIAN_POINT ( 'NONE',  ( -0.008945125900505456612, 117.5133074443058945, 0.4476506782301717946 ) ) ;
#14803 = ADVANCED_FACE ( 'NONE', ( #373 ), #38912, .T. ) ;
#14804 = DIRECTION ( 'NONE',  ( -4.017660918040594346E-17, 1.000000000000000000, 2.376309959284834438E-19 ) ) ;
#14805 = CARTESIAN_POINT ( 'NONE',  ( 11.68195978820569536, 118.7263634577040676, 0.3785536984881910372 ) ) ;
#14806 = CARTESIAN_POINT ( 'NONE',  ( 15.64207015331054862, 147.2204672151589193, 0.3125657877211908686 ) ) ;
#14807 = FACE_OUTER_BOUND ( 'NONE', #32490, .T. ) ;
#14808 = CARTESIAN_POINT ( 'NONE',  ( 0.6634555152105963138, 29.00466287695533296, -0.7151348822165174424 ) ) ;
#14809 = CARTESIAN_POINT ( 'NONE',  ( -23.28768492013425018, 149.3500807853454546, -0.5424486132203800715 ) ) ;
#14810 = FACE_OUTER_BOUND ( 'NONE', #31197, .T. ) ;
#14811 = ORIENTED_EDGE ( 'NONE', *, *, #2912, .F. ) ;
#14812 = CARTESIAN_POINT ( 'NONE',  ( 1.248107678658480997E-15, 12.96416000000000146, 0.000000000000000000 ) ) ;
#14813 = ORIENTED_EDGE ( 'NONE', *, *, #5353, .T. ) ;
#14814 = CARTESIAN_POINT ( 'NONE',  ( 5.927595846997289364, 118.6114240595178018, 1.195360803812330452 ) ) ;
#14815 = CARTESIAN_POINT ( 'NONE',  ( -9.909999474182706436, 76.95545850745379823, -1.523999999999998023 ) ) ;
#14816 = CARTESIAN_POINT ( 'NONE',  ( 14.57523308444390686, 121.8773232776577942, 1.525373117076484153 ) ) ;
#14817 = CARTESIAN_POINT ( 'NONE',  ( -57.87993506102255736, 0.7648122704444343389, -1.011066771892038085 ) ) ;
#14818 = CARTESIAN_POINT ( 'NONE',  ( 19.90609901365546364, 149.5711785761137662, -1.665592367946398422 ) ) ;
#14819 = CARTESIAN_POINT ( 'NONE',  ( 1.173990663012069113, -13.46572784750561880, -4.469126434461346165 ) ) ;
#14820 = CARTESIAN_POINT ( 'NONE',  ( -16.15135472115380111, 155.1612327564137388, -1.525667687477715084 ) ) ;
#14821 = CARTESIAN_POINT ( 'NONE',  ( 4.947454507184974482, 117.6245515869850919, -0.7568747717558176324 ) ) ;
#14822 = ORIENTED_EDGE ( 'NONE', *, *, #7655, .T. ) ;
#14823 = CARTESIAN_POINT ( 'NONE',  ( -9.177823364990569388, 124.0935018032023436, -0.02293427522457971990 ) ) ;
#14824 = CARTESIAN_POINT ( 'NONE',  ( 0.01147819631900381422, 118.8623374019222894, -0.5744158801423950855 ) ) ;
#14825 = CARTESIAN_POINT ( 'NONE',  ( 2.462693652799142541, -15.54209007114785912, 5.820364621994587040 ) ) ;
#14826 = CARTESIAN_POINT ( 'NONE',  ( 20.83467972660109524, 65.95194780259438971, -1.904999999999999583 ) ) ;
#14827 = CARTESIAN_POINT ( 'NONE',  ( -1.083479109511653826, 117.9496054725919123, -1.389487458230839190 ) ) ;
#14828 = ORIENTED_EDGE ( 'NONE', *, *, #3265, .F. ) ;
#14829 = CARTESIAN_POINT ( 'NONE',  ( 6.637665810843221159, 119.8184877057495754, 1.268479684707346511 ) ) ;
#14830 = CARTESIAN_POINT ( 'NONE',  ( -5.586884702347496123, 98.39146620154573952, -0.1116392523995361624 ) ) ;
#14831 = ADVANCED_FACE ( 'NONE', ( #16739 ), #19716, .T. ) ;
#14832 = CARTESIAN_POINT ( 'NONE',  ( -2.686747594420624718, 118.0959492836583422, -0.9542362816721940977 ) ) ;
#14833 = CARTESIAN_POINT ( 'NONE',  ( -2.504607545376518640, 120.2382744777187611, 0.4047138806074999096 ) ) ;
#14834 = CARTESIAN_POINT ( 'NONE',  ( -3.184215270518052421, -12.39116543543024562, -7.798991864805400631 ) ) ;
#14835 = CARTESIAN_POINT ( 'NONE',  ( 16.14702439603928141, 146.0959698922748942, 1.294960982472433741 ) ) ;
#14836 = CARTESIAN_POINT ( 'NONE',  ( -4.800388046790427410, 115.6909491485453003, -1.474219336065222041 ) ) ;
#14837 = CARTESIAN_POINT ( 'NONE',  ( 1.937878880890121058, 116.8467566806161386, -0.3061478142745880371 ) ) ;
#14838 = DIRECTION ( 'NONE',  ( -5.188838149069472160E-16, 1.699382548006136559E-16, 1.000000000000000000 ) ) ;
#14839 = CARTESIAN_POINT ( 'NONE',  ( -58.04313065737859745, 0.4109646669389979134, 0.8003343135030365207 ) ) ;
#14840 = CARTESIAN_POINT ( 'NONE',  ( -29.02482657613216332, 65.73348897311474559, -1.524000000000006905 ) ) ;
#14841 = EDGE_CURVE ( 'NONE', #21058, #42038, #12914, .T. ) ;
#14842 = CARTESIAN_POINT ( 'NONE',  ( 2.037655544652285933, -15.20941935993469940, 5.943311982828842766 ) ) ;
#14843 = CARTESIAN_POINT ( 'NONE',  ( -4.119060676135726240, 118.2429491485453354, 0.1854733653491233702 ) ) ;
#14844 = CARTESIAN_POINT ( 'NONE',  ( 4.686997755226863127, 113.9923204192467523, -1.949621542610482372 ) ) ;
#14845 = ORIENTED_EDGE ( 'NONE', *, *, #17814, .F. ) ;
#14846 = CARTESIAN_POINT ( 'NONE',  ( -53.00789483126595769, 12.40033530745290236, 4.180047681284801975 ) ) ;
#14847 = CARTESIAN_POINT ( 'NONE',  ( -8.226885276541187508, 120.3464503904280321, -1.440290466561924498 ) ) ;
#14848 = DIRECTION ( 'NONE',  ( 0.9998004120163608288, 0.000000000000000000, 0.01997839162482749342 ) ) ;
#14849 = CARTESIAN_POINT ( 'NONE',  ( 4.223530570022107966, 118.2238270089485184, 0.4905371497760634969 ) ) ;
#14850 = CARTESIAN_POINT ( 'NONE',  ( -1.530927031713913866, 120.6610732671444595, -0.3086461854719843578 ) ) ;
#14851 = CARTESIAN_POINT ( 'NONE',  ( -4.618747647011250734, 118.0632304573675810, 0.5484251646978447470 ) ) ;
#14852 = CARTESIAN_POINT ( 'NONE',  ( -20.79116009376201646, 79.67004825550966984, -1.270000000000004015 ) ) ;
#14853 = FACE_OUTER_BOUND ( 'NONE', #16533, .T. ) ;
#14854 = ORIENTED_EDGE ( 'NONE', *, *, #27682, .F. ) ;
#14855 = CARTESIAN_POINT ( 'NONE',  ( -3.562413952978887632, 23.18266144714348798, 2.948169924785601470 ) ) ;
#14856 = CARTESIAN_POINT ( 'NONE',  ( -16.54853992722335931, 147.5857818452174115, -1.770514083359864044 ) ) ;
#14857 = DIRECTION ( 'NONE',  ( 0.9454731675810332803, -0.3256999990547855828, 8.537024980200802097E-16 ) ) ;
#14858 = CARTESIAN_POINT ( 'NONE',  ( -42.18385791109447780, 22.43440044418187185, 1.696665287888085460 ) ) ;
#14859 = LINE ( 'NONE', #24447, #5906 ) ;
#14860 = CARTESIAN_POINT ( 'NONE',  ( -6.066676402028498671, 121.4189492134451029, 0.06607077281897212606 ) ) ;
#14861 = VECTOR ( 'NONE', #42067, 1000.000000000000114 ) ;
#14862 = CARTESIAN_POINT ( 'NONE',  ( 4.064150447026247726, 23.66704930264554818, -2.198397014704132513 ) ) ;
#14863 = CARTESIAN_POINT ( 'NONE',  ( 5.835170694357040055, 117.3723397083485622, 0.6929373658347461884 ) ) ;
#14864 = CARTESIAN_POINT ( 'NONE',  ( 1.757780374235184739, 104.6144662015457243, -4.503817898648089901 ) ) ;
#14866 = CARTESIAN_POINT ( 'NONE',  ( 20.65103440377610866, 150.0789294893613999, -1.463288793709878632 ) ) ;
#14865 = CARTESIAN_POINT ( 'NONE',  ( 3.198896590522081862, -14.38863201745455100, 2.123570546440393780 ) ) ;
#14867 = CARTESIAN_POINT ( 'NONE',  ( -14.85905242749878497, 128.5561590274816126, 1.519445497462470485 ) ) ;
#14868 = AXIS2_PLACEMENT_3D ( 'NONE', #12044, #25033, #38036 ) ;
#14869 = CARTESIAN_POINT ( 'NONE',  ( -3.633452533992191036, 26.69063122243967712, -2.854640957048627747 ) ) ;
#14870 = CARTESIAN_POINT ( 'NONE',  ( -18.16683071450857412, 125.1529741258727597, -1.044517495177846422 ) ) ;
#14871 = CARTESIAN_POINT ( 'NONE',  ( -0.9510052327539034733, 17.61975311242802533, 0.2078495401503242801 ) ) ;
#14872 = ORIENTED_EDGE ( 'NONE', *, *, #29749, .F. ) ;
#14873 = CARTESIAN_POINT ( 'NONE',  ( -53.01551111795198068, 8.729259440421092364, 0.3204493394367104453 ) ) ;
#14874 = CARTESIAN_POINT ( 'NONE',  ( -16.08279055836844051, 146.6973543426590254, 0.5313625374031881732 ) ) ;
#14875 = CARTESIAN_POINT ( 'NONE',  ( 5.114911232981273592, -13.88689734646693452, 3.682185042294812582 ) ) ;
#14876 = CARTESIAN_POINT ( 'NONE',  ( 14.11650378654203664, 131.1061190467503934, -1.279305142450559707 ) ) ;
#14877 = EDGE_LOOP ( 'NONE', ( #40031, #26421, #40601, #6047 ) ) ;
#14878 = CARTESIAN_POINT ( 'NONE',  ( 1.071098897595643473, 115.7029399971135319, 1.745873157700803757 ) ) ;
#14879 = CARTESIAN_POINT ( 'NONE',  ( 3.236250843111535769, -14.18372432684703099, 3.165927027233770286 ) ) ;
#14880 = CARTESIAN_POINT ( 'NONE',  ( -4.899907873566092142, 117.6566817052388245, -0.9515826219193989077 ) ) ;
#14881 = EDGE_CURVE ( 'NONE', #6467, #24193, #513, .T. ) ;
#14882 = CARTESIAN_POINT ( 'NONE',  ( 9.191399985966370423, 124.2403664864748549, 0.1492717680338160047 ) ) ;
#14883 = ORIENTED_EDGE ( 'NONE', *, *, #8685, .T. ) ;
#14884 = CARTESIAN_POINT ( 'NONE',  ( 20.38365538121562892, 147.8414448467482600, 2.482674703111231285 ) ) ;
#14885 = CARTESIAN_POINT ( 'NONE',  ( 0.6412933796112577634, 156.3034662015457741, 0.01281456791805622546 ) ) ;
#14886 = CARTESIAN_POINT ( 'NONE',  ( -11.05715273818225164, 82.67346420587206524, 1.524000000000000021 ) ) ;
#14887 = CARTESIAN_POINT ( 'NONE',  ( 0.0002734175338603746100, 159.6054662015457382, -0.01368293144939978188 ) ) ;
#14888 = CARTESIAN_POINT ( 'NONE',  ( 15.48609530480946894, 120.8153160915142337, -0.009749853210865230824 ) ) ;
#14889 = AXIS2_PLACEMENT_3D ( 'NONE', #40753, #30307, #21125 ) ;
#14890 = CARTESIAN_POINT ( 'NONE',  ( 0.09221630143774380006, 107.6766875080336376, -4.614880812453306724 ) ) ;
#14891 = CARTESIAN_POINT ( 'NONE',  ( 1.759666435841401810, -15.35400245117242513, 5.409080988316447680 ) ) ;
#14892 = CARTESIAN_POINT ( 'NONE',  ( -46.60530155212503445, 26.17382724835477958, 1.523999999999991140 ) ) ;
#14893 = DIRECTION ( 'NONE',  ( -0.1715592850456333085, -0.1224830539174543292, -0.9775302108976914317 ) ) ;
#14894 = CARTESIAN_POINT ( 'NONE',  ( -4.704233533693831681, 117.8349189730105309, 0.8529071958809373299 ) ) ;
#14895 = EDGE_LOOP ( 'NONE', ( #14500, #12391, #22139, #8650 ) ) ;
#14896 = ORIENTED_EDGE ( 'NONE', *, *, #9552, .T. ) ;
#14897 = CARTESIAN_POINT ( 'NONE',  ( -5.078986093043186045, 94.83546620154572793, -0.1014902294541231709 ) ) ;
#14898 = CARTESIAN_POINT ( 'NONE',  ( -5.583873019120129122, 118.2001624726323854, -1.144883371530341254 ) ) ;
#14899 = CARTESIAN_POINT ( 'NONE',  ( -4.531575537552095412, 119.7344140837147819, -0.5249638875923485770 ) ) ;
#14900 = CARTESIAN_POINT ( 'NONE',  ( 4.943796685340839936, 117.5327713888434431, 0.9784953665843204584 ) ) ;
#14901 = CARTESIAN_POINT ( 'NONE',  ( -4.731399709915055318, 117.6315807060625929, -1.144721263631117703 ) ) ;
#14902 = CARTESIAN_POINT ( 'NONE',  ( -0.4040709798586945567, 123.7646714092001190, 0.1152108919326052111 ) ) ;
#14903 = FACE_OUTER_BOUND ( 'NONE', #27203, .T. ) ;
#14904 = CARTESIAN_POINT ( 'NONE',  ( -56.01560174880540188, 6.374421267034191985, 2.942705720416951110 ) ) ;
#14905 = CARTESIAN_POINT ( 'NONE',  ( -5.305748947172282293, 57.14999999999997016, -5.247078976224250013 ) ) ;
#14906 = CARTESIAN_POINT ( 'NONE',  ( 3.514454466653502251, -13.37942318924494067, 2.559657187549406299 ) ) ;
#14907 = CARTESIAN_POINT ( 'NONE',  ( 1.225173952871632332, 106.6134986179334589, -4.982835752217485314 ) ) ;
#14908 = EDGE_CURVE ( 'NONE', #37389, #22515, #6126, .T. ) ;
#14909 = CARTESIAN_POINT ( 'NONE',  ( -3.890668369019033790, 28.55756886444901710, 1.917437575001415651 ) ) ;
#14910 = CARTESIAN_POINT ( 'NONE',  ( -1.199145814505997665, 115.7029469948677018, 1.697500384976515564 ) ) ;
#14911 = CARTESIAN_POINT ( 'NONE',  ( -2.406711483539481389, 4.503775517365914638, 3.979180414515509412 ) ) ;
#14912 = ORIENTED_EDGE ( 'NONE', *, *, #18525, .F. ) ;
#14913 = CARTESIAN_POINT ( 'NONE',  ( 3.957041461616310762, 104.6144662015457811, -2.768236986571138480 ) ) ;
#14914 = CARTESIAN_POINT ( 'NONE',  ( 1.897852064921616622, -15.54654116324019597, 5.408738352340563438 ) ) ;
#14915 = CARTESIAN_POINT ( 'NONE',  ( -19.86924145434966960, 147.9128418260961837, 1.725515945229960657 ) ) ;
#14916 = CARTESIAN_POINT ( 'NONE',  ( -0.6881565663083963891, 18.49284505249605459, 0.6899137464212180548 ) ) ;
#14917 = CARTESIAN_POINT ( 'NONE',  ( -0.9731698936423014423, 13.46246454747003618, 0.06867709314994872860 ) ) ;
#14918 = ORIENTED_EDGE ( 'NONE', *, *, #24523, .T. ) ;
#14919 = CIRCLE ( 'NONE', #31247, 0.2540000000000000036 ) ;
#14920 = EDGE_LOOP ( 'NONE', ( #41142, #40216 ) ) ;
#14921 = DIRECTION ( 'NONE',  ( -4.017660918040594346E-17, 1.000000000000000000, 2.376309959284834438E-19 ) ) ;
#14922 = CARTESIAN_POINT ( 'NONE',  ( 2.416298757281802434, 119.8248006784163380, 0.5703471319689770169 ) ) ;
#14923 =( NAMED_UNIT ( * ) PLANE_ANGLE_UNIT ( ) SI_UNIT ( $, .RADIAN. ) );
#14924 = EDGE_CURVE ( 'NONE', #32706, #39773, #36254, .T. ) ;
#14925 = CARTESIAN_POINT ( 'NONE',  ( -10.06202586252270770, 123.8737202207250618, 0.7052144931501602709 ) ) ;
#14926 = EDGE_CURVE ( 'NONE', #8022, #33026, #17868, .T. ) ;
#14927 = FACE_OUTER_BOUND ( 'NONE', #39173, .T. ) ;
#14928 = AXIS2_PLACEMENT_3D ( 'NONE', #26608, #4054, #17015 ) ;
#14929 = CARTESIAN_POINT ( 'NONE',  ( 3.297440819997984107, -14.19009280176566890, 4.446257544676719853 ) ) ;
#14930 = CARTESIAN_POINT ( 'NONE',  ( 18.08730999440950882, 147.8422069945528108, -1.617706263729447702 ) ) ;
#14931 = CARTESIAN_POINT ( 'NONE',  ( -19.70389350229454095, 149.1964539096042870, -2.489783701940901484 ) ) ;
#14932 = DIRECTION ( 'NONE',  ( -1.000000000000000000, -0.000000000000000000, -0.000000000000000000 ) ) ;
#14933 = CARTESIAN_POINT ( 'NONE',  ( -6.497774333512897904, 30.00467535414699327, 0.6616146369854277731 ) ) ;
#14934 = CARTESIAN_POINT ( 'NONE',  ( 8.172795105213573663, 122.8283871457973362, -0.1257892658093056615 ) ) ;
#14935 = ORIENTED_EDGE ( 'NONE', *, *, #40941, .T. ) ;
#14936 = CARTESIAN_POINT ( 'NONE',  ( 2.667920334613889555, -13.82128762729334426, -0.01087480101406306660 ) ) ;
#14937 = EDGE_CURVE ( 'NONE', #31748, #35799, #19256, .T. ) ;
#14938 = EDGE_CURVE ( 'NONE', #23948, #40785, #9512, .T. ) ;
#14939 = CARTESIAN_POINT ( 'NONE',  ( -58.34279097978161133, -0.2008976519008942030, 0.5874393231764968304 ) ) ;
#14940 = CARTESIAN_POINT ( 'NONE',  ( 4.571311019248293306, -6.119132638730012452, 0.7325351754658009362 ) ) ;
#14941 = CARTESIAN_POINT ( 'NONE',  ( 16.67506696845903846, 147.9788754379930822, 1.914365833524547478 ) ) ;
#14942 = CARTESIAN_POINT ( 'NONE',  ( -1.655660646363030786, 31.15378821692802802, 3.245565323402777480 ) ) ;
#14943 = CARTESIAN_POINT ( 'NONE',  ( -3.444826702830499965, 112.1633951907056996, 2.719597167543061467 ) ) ;
#14944 = CARTESIAN_POINT ( 'NONE',  ( 4.440276399826426967, -1.430929408009915083, -1.287880193523989636 ) ) ;
#14945 = CARTESIAN_POINT ( 'NONE',  ( 15.21351360038791789, 143.4186079242267340, 0.3040022078858843346 ) ) ;
#14946 = AXIS2_PLACEMENT_3D ( 'NONE', #32396, #19807, #7056 ) ;
#14947 = EDGE_CURVE ( 'NONE', #14129, #27965, #35587, .T. ) ;
#14948 = CARTESIAN_POINT ( 'NONE',  ( -8.308456333890557488, -0.7205321100333081930, 1.466575456822119206 ) ) ;
#14949 = CARTESIAN_POINT ( 'NONE',  ( -56.90063064090522715, 2.680628813859151194, -1.231466298089203937 ) ) ;
#14950 = CARTESIAN_POINT ( 'NONE',  ( -8.775520152584638467, 117.7647785482566576, -0.4778187140148553724 ) ) ;
#14951 = LINE ( 'NONE', #23694, #27828 ) ;
#14952 = LINE ( 'NONE', #5399, #8758 ) ;
#14953 = CARTESIAN_POINT ( 'NONE',  ( -6.446885413170102552, 29.42808026494702389, 0.2842954123359194840 ) ) ;
#14954 = CARTESIAN_POINT ( 'NONE',  ( -8.418590987418564708, -6.603242653765095227, 0.8142584484527041200 ) ) ;
#14955 = CARTESIAN_POINT ( 'NONE',  ( 17.14499999999999957, 71.11999999999999034, -5.016499999999999737 ) ) ;
#14956 = CARTESIAN_POINT ( 'NONE',  ( -41.28107547821694112, 23.22158991241130011, 1.523999999999988475 ) ) ;
#14957 = CARTESIAN_POINT ( 'NONE',  ( -58.83227707057489653, -0.08366279998001102669, -1.541589583118017482E-14 ) ) ;
#14958 = CARTESIAN_POINT ( 'NONE',  ( 0.8647483397478292755, 121.9014879524050343, -0.2897378433829551625 ) ) ;
#14959 = CARTESIAN_POINT ( 'NONE',  ( -7.966904459259942506, 158.6775731370129279, 0.2701962758350455185 ) ) ;
#14960 = ORIENTED_EDGE ( 'NONE', *, *, #730, .T. ) ;
#14961 = CARTESIAN_POINT ( 'NONE',  ( -58.33777482027512207, 1.113448835244237767, -1.208045587469442017 ) ) ;
#14962 =( BOUNDED_SURFACE ( )  B_SPLINE_SURFACE ( 3, 2, ( 
 ( #37758, #21973, #40758 ),
 ( #41176, #9008, #34363 ),
 ( #40964, #41392, #2630 ),
 ( #1993, #5617, #5824 ),
 ( #27956, #24759, #11555 ),
 ( #12197, #18780, #9218 ),
 ( #15165, #11769, #2420 ),
 ( #21545, #37547, #15380 ),
 ( #38407, #2207, #18573 ),
 ( #31581, #28172, #28594 ),
 ( #35206, #8798, #15589 ),
 ( #31791, #12413, #34575 ),
 ( #8370, #5402, #14747 ),
 ( #25405, #18358, #21336 ),
 ( #28386, #25189, #22175 ),
 ( #38192, #37973, #6032 ),
 ( #35005, #18994, #1785 ),
 ( #11980, #31364, #5195 ),
 ( #24974, #24539, #31153 ),
 ( #19829, #12818, #25806 ) ),
 .UNSPECIFIED., .F., .F., .T. ) 
 B_SPLINE_SURFACE_WITH_KNOTS ( ( 4, 2, 2, 2, 2, 2, 2, 2, 2, 4 ),
 ( 3, 3 ),
 ( -3.903127820947815962E-18, 0.0002906707827382450766, 0.0004360061741073695393, 0.0005813415654764940562, 0.0008720123482147429817, 0.001162683130952992016, 0.002325366261905987934, 0.002906707827382486002, 0.003488049392858983636, 0.004650732523811979338 ),
 ( 0.000000000000000000, 0.7006112354927811481 ),
 .UNSPECIFIED. ) 
 GEOMETRIC_REPRESENTATION_ITEM ( )  RATIONAL_B_SPLINE_SURFACE ( (
 ( 1.000000000000000000, 0.8321377275423429420, 0.8994878432830558657),
 ( 1.000000000000000000, 0.8321377275423429420, 0.8994878432830558657),
 ( 1.000000000000000000, 0.8321378623915750561, 0.8994879240277457999),
 ( 1.000000000000000000, 0.8321376435713845332, 0.8994877930031328628),
 ( 1.000000000000000000, 0.8321373692613844852, 0.8994876287524689040),
 ( 1.000000000000000000, 0.8321375004543833942, 0.8994877073078884067),
 ( 1.000000000000000000, 0.8321376855588478172, 0.8994878181442822473),
 ( 1.000000000000000000, 0.8321378848318423671, 0.8994879374644735304),
 ( 1.000000000000000000, 0.8321377198722352819, 0.8994878386903677470),
 ( 1.000000000000000000, 0.8321377383289947360, 0.8994878497418605789),
 ( 1.000000000000000000, 0.8321377253651141004, 0.8994878419793801427),
 ( 1.000000000000000000, 0.8321377372094624914, 0.8994878490715096930),
 ( 1.000000000000000000, 0.8321377976487042138, 0.8994878852611696285),
 ( 1.000000000000000000, 0.8321376953121012443, 0.8994878239843113743),
 ( 1.000000000000000000, 0.8321372635390859029, 0.8994875654483320826),
 ( 1.000000000000000000, 0.8321371748454207129, 0.8994875123405583484),
 ( 1.000000000000000000, 0.8321377042314352934, 0.8994878293250081480),
 ( 1.000000000000000000, 0.8321377726643398587, 0.8994878703010936727),
 ( 1.000000000000000000, 0.8321377275429439058, 0.8994878432834155779),
 ( 1.000000000000000000, 0.8321377275429439058, 0.8994878432834155779) ) ) 
 REPRESENTATION_ITEM ( '' )  SURFACE ( )  );
#14963 = VERTEX_POINT ( 'NONE', #6963 ) ;
#14964 = CARTESIAN_POINT ( 'NONE',  ( -4.085839532347240066, 71.06758511999679229, 1.270000000000005125 ) ) ;
#14965 = CARTESIAN_POINT ( 'NONE',  ( -0.6412933796113865492, 156.3034662015457741, -0.01281456791805603290 ) ) ;
#14966 = CARTESIAN_POINT ( 'NONE',  ( 6.104261451579751530, -14.47397795074312299, 1.449478640324443290 ) ) ;
#14967 = CARTESIAN_POINT ( 'NONE',  ( -20.99182874412630184, 148.0559997909317644, 1.564581863923973470 ) ) ;
#14968 = CARTESIAN_POINT ( 'NONE',  ( 17.77240244235137112, 153.9999837190418930, -1.018827867329159531 ) ) ;
#14969 = CARTESIAN_POINT ( 'NONE',  ( -4.544942180623752215, 12.81246518813932589, 0.8472608254572608910 ) ) ;
#14970 = CARTESIAN_POINT ( 'NONE',  ( -3.764301891765764463, 116.7207137014398626, -0.2841661138181404977 ) ) ;
#14971 = EDGE_CURVE ( 'NONE', #17471, #25107, #24678, .T. ) ;
#14972 = CARTESIAN_POINT ( 'NONE',  ( -50.15850345609781158, 16.04140918442848829, -4.890455600740700959 ) ) ;
#14973 = ORIENTED_EDGE ( 'NONE', *, *, #27398, .T. ) ;
#14974 = CARTESIAN_POINT ( 'NONE',  ( 5.555698890664002576, 116.7273188082384081, 0.2769282034075690180 ) ) ;
#14975 = CARTESIAN_POINT ( 'NONE',  ( -8.761523658392190939, 74.56051954986229191, 1.524000000000002242 ) ) ;
#14976 = CARTESIAN_POINT ( 'NONE',  ( -8.163394002857751630, 121.3802920439979118, 0.9196017894915151647 ) ) ;
#14977 = CARTESIAN_POINT ( 'NONE',  ( -48.97240568284989592, 17.83076478022523048, -5.072389016522397931 ) ) ;
#14978 = CARTESIAN_POINT ( 'NONE',  ( 1.064682733363894407, 157.9544661020348997, -1.608744340525367633 ) ) ;
#14979 = AXIS2_PLACEMENT_3D ( 'NONE', #30661, #40484, #37269 ) ;
#14980 = CARTESIAN_POINT ( 'NONE',  ( -21.10297322700582257, 148.1333099715771766, -2.360403108977008557 ) ) ;
#14981 = CARTESIAN_POINT ( 'NONE',  ( -52.26939619200407350, 13.58078015197115818, -4.476849201000089096 ) ) ;
#14982 = CARTESIAN_POINT ( 'NONE',  ( 7.149839403334782517, 121.7184703992695773, -0.4778388566947553984 ) ) ;
#14983 = ORIENTED_EDGE ( 'NONE', *, *, #38817, .F. ) ;
#14984 = CARTESIAN_POINT ( 'NONE',  ( -13.99859221269053222, 128.5416456306063253, -1.961142612884885450 ) ) ;
#14985 = CARTESIAN_POINT ( 'NONE',  ( 4.167245103190982292, -15.48560191675932352, 1.819225864046467356 ) ) ;
#14986 = CARTESIAN_POINT ( 'NONE',  ( -4.500643392528203890, 118.1244706977970793, -0.6706124182329965544 ) ) ;
#14987 = EDGE_CURVE ( 'NONE', #20566, #36869, #4587, .T. ) ;
#14988 = AXIS2_PLACEMENT_3D ( 'NONE', #23649, #40298, #24079 ) ;
#14989 = CARTESIAN_POINT ( 'NONE',  ( -57.69570286664291103, 2.558035660193719529, -1.875687456014384802 ) ) ;
#14990 = CARTESIAN_POINT ( 'NONE',  ( -4.865551005416930863, 117.4776490099701505, 0.9870761551034079595 ) ) ;
#14991 = CARTESIAN_POINT ( 'NONE',  ( 17.64033768477175101, 147.6919162452172145, 2.236185705752640640 ) ) ;
#14992 = CARTESIAN_POINT ( 'NONE',  ( -6.505112547751767921E-14, 75.78546620154573077, -1.207165459009924652E-19 ) ) ;
#14993 = TOROIDAL_SURFACE ( 'NONE', #18394, 3.683000000000000718, 0.5080000000000000071 ) ;
#14994 = CARTESIAN_POINT ( 'NONE',  ( -1.112825283668275045, 5.041181605477844663, 8.348645504544187190 ) ) ;
#14995 = CARTESIAN_POINT ( 'NONE',  ( 0.6635084510828398452, 156.3292479207028407, 0.3574603001491371002 ) ) ;
#14996 = CARTESIAN_POINT ( 'NONE',  ( 3.108425975021062992, 118.0774503567615028, -0.8384703576004943759 ) ) ;
#14998 = ORIENTED_EDGE ( 'NONE', *, *, #7896, .T. ) ;
#14997 = LINE ( 'NONE', #2249, #14520 ) ;
#14999 = CARTESIAN_POINT ( 'NONE',  ( -4.812631915126818427, 117.9394518360245172, 0.9265897817142734194 ) ) ;
#15000 = TOROIDAL_SURFACE ( 'NONE', #17740, 17.68910244842765778, 0.6350000000000000089 ) ;
#15001 = DIRECTION ( 'NONE',  ( 0.7770581983690836303, -0.6294287539884032556, 5.101669463485833779E-16 ) ) ;
#15002 = CARTESIAN_POINT ( 'NONE',  ( -58.16721443865020547, 0.09938604254088045931, 0.2878065994479881429 ) ) ;
#15003 = CARTESIAN_POINT ( 'NONE',  ( -51.09183723991096571, 15.73968240350219538, 4.743875354842988834 ) ) ;
#15004 = CARTESIAN_POINT ( 'NONE',  ( -13.40764007945161218, 156.9487217736090940, -0.07645926402191043081 ) ) ;
#15005 = ORIENTED_EDGE ( 'NONE', *, *, #6873, .F. ) ;
#15006 = CARTESIAN_POINT ( 'NONE',  ( -51.38196307734524737, 20.99359796827592817, -0.3730309213897348153 ) ) ;
#15007 = CARTESIAN_POINT ( 'NONE',  ( -6.881936038377706844, 121.7539469809695873, -0.5834300994894434655 ) ) ;
#15008 = CARTESIAN_POINT ( 'NONE',  ( -8.207314164617301344, 120.6877426416252490, 1.076149196205786085 ) ) ;
#15009 = ORIENTED_EDGE ( 'NONE', *, *, #4291, .T. ) ;
#15010 = CARTESIAN_POINT ( 'NONE',  ( 0.5120572057462492443, 118.7629491485454025, -1.259108956518884881 ) ) ;
#15011 = CARTESIAN_POINT ( 'NONE',  ( 0.004910621514677531059, 156.3161161488371533, -0.2457475809811480449 ) ) ;
#15012 = CARTESIAN_POINT ( 'NONE',  ( 5.306636623844629419, -13.66766582561489152, 3.280230747366464694 ) ) ;
#15013 = CARTESIAN_POINT ( 'NONE',  ( -17.54374246740532683, 153.9260871938423065, 1.166327135487699618 ) ) ;
#15014 = CARTESIAN_POINT ( 'NONE',  ( -21.91949108387693457, 59.24500507708427932, -1.270000000000001128 ) ) ;
#15015 = CARTESIAN_POINT ( 'NONE',  ( 3.288660796955097609, 159.4686222989141697, 0.1587487428767535014 ) ) ;
#15016 = CARTESIAN_POINT ( 'NONE',  ( 9.081988434275306332, 124.1603627706468842, 0.2262077945552918301 ) ) ;
#15017 = LINE ( 'NONE', #34848, #2652 ) ;
#15018 = CARTESIAN_POINT ( 'NONE',  ( -0.6497956273327881727, 21.66276798020532013, -0.7290388503713802759 ) ) ;
#15019 = CARTESIAN_POINT ( 'NONE',  ( -22.53260066761450631, 150.7862151120626777, -0.5269028172337438809 ) ) ;
#15020 = CARTESIAN_POINT ( 'NONE',  ( -17.09258512000246100, 84.17916046765628835, -1.524000000000002908 ) ) ;
#15021 = CARTESIAN_POINT ( 'NONE',  ( -8.857543928232141539, 74.53795647042551309, 1.270000000000002016 ) ) ;
#15022 = ORIENTED_EDGE ( 'NONE', *, *, #6991, .F. ) ;
#15023 = CARTESIAN_POINT ( 'NONE',  ( 5.825538371254951997, 118.3804061813496276, 1.156786149343531411 ) ) ;
#15024 = CARTESIAN_POINT ( 'NONE',  ( -14.38915334913366806, 80.27078028363496287, -1.270000000000000906 ) ) ;
#15025 = CARTESIAN_POINT ( 'NONE',  ( 1.253347288035624674, 159.2526592949493534, 1.130111582746273990 ) ) ;
#15026 = CARTESIAN_POINT ( 'NONE',  ( -57.74058121727584592, 1.065718057878028979, -1.162857118035388160 ) ) ;
#15027 = CARTESIAN_POINT ( 'NONE',  ( 3.179094171403590963, 118.3302933575512412, -0.7469981754565536702 ) ) ;
#15028 = CARTESIAN_POINT ( 'NONE',  ( 8.327223946240280839, 23.24253473731531727, -1.329248712143314748 ) ) ;
#15029 = CARTESIAN_POINT ( 'NONE',  ( -14.51227343941619274, 121.4416029531759591, -1.418621967605989909 ) ) ;
#15030 = CARTESIAN_POINT ( 'NONE',  ( 4.880012207426760895, 117.7310911472439017, -0.7975209570774519641 ) ) ;
#15031 = VECTOR ( 'NONE', #31333, 999.9999999999998863 ) ;
#15032 = CARTESIAN_POINT ( 'NONE',  ( 5.366896802164511371, 117.1940586887245388, 0.8977625253398615612 ) ) ;
#15033 = VERTEX_POINT ( 'NONE', #26759 ) ;
#15034 = CARTESIAN_POINT ( 'NONE',  ( -9.048378227557902775, 123.9859359328134190, -0.09628433740681502373 ) ) ;
#15035 = CARTESIAN_POINT ( 'NONE',  ( -5.003445044761956950, 119.2220797256985350, -1.100019038710256192 ) ) ;
#15036 = CARTESIAN_POINT ( 'NONE',  ( 4.578653272329702872, -15.42525073102989097, 4.254151796826286969 ) ) ;
#15037 = AXIS2_PLACEMENT_3D ( 'NONE', #16566, #32341, #3170 ) ;
#15038 = CARTESIAN_POINT ( 'NONE',  ( 1.247998466936323035E-15, 12.96302561210691806, 0.000000000000000000 ) ) ;
#15039 = DIRECTION ( 'NONE',  ( -5.188838149069472160E-16, 1.699382548006136066E-16, 1.000000000000000000 ) ) ;
#15040 = ORIENTED_EDGE ( 'NONE', *, *, #31380, .F. ) ;
#15041 = CARTESIAN_POINT ( 'NONE',  ( 12.01154561878600546, 123.1955650103826798, 1.772196977085516378 ) ) ;
#15042 = CARTESIAN_POINT ( 'NONE',  ( -5.276425599434919178, 115.6909491485453003, 0.8138454675774937641 ) ) ;
#15043 = CARTESIAN_POINT ( 'NONE',  ( -0.1065646865916159425, 105.8844662015457203, 5.332932678536313809 ) ) ;
#15044 = CARTESIAN_POINT ( 'NONE',  ( 4.050812540078617019, -7.421221357003889629, 7.384888961799156881 ) ) ;
#15045 = CARTESIAN_POINT ( 'NONE',  ( 1.710293758672529751, 156.3676537730497387, 0.7734167093480265320 ) ) ;
#15046 = DIRECTION ( 'NONE',  ( -0.1469470846586743706, 0.000000000000000000, 0.9891443546370348727 ) ) ;
#15047 = CARTESIAN_POINT ( 'NONE',  ( 15.52007106302753492, 121.3130774642648220, -0.3850180365863630216 ) ) ;
#15048 = DIRECTION ( 'NONE',  ( 0.4849315768086426282, 0.8745520943968309036, 1.030032898892908135E-16 ) ) ;
#15049 = CARTESIAN_POINT ( 'NONE',  ( -57.97682026406428690, 0.5548386587714120299, 0.8895012536376524226 ) ) ;
#15050 = DIRECTION ( 'NONE',  ( 4.017660918040594346E-17, -1.000000000000000000, -2.376309959284834438E-19 ) ) ;
#15051 = AXIS2_PLACEMENT_3D ( 'NONE', #27749, #17526, #40759 ) ;
#15052 = B_SPLINE_CURVE_WITH_KNOTS ( 'NONE', 3,
 ( #28954, #12770, #10, #13197, #38356, #5984, #25760, #31953, #28754, #15749, #25969, #41767, #38977, #12568 ),
 .UNSPECIFIED., .F., .F.,
 ( 4, 1, 1, 1, 2, 1, 1, 1, 1, 1, 4 ),
 ( 0.2031000000004874739, 0.2063375000004613602, 0.2095750000004352187, 0.2128125000004091050, 0.2160500000003829635, 0.2667374999999738705, 0.3174249999995648053, 0.3681124999991557400, 0.4187999999987466193, 0.5201749999979283778, 0.6215499999971101364 ),
 .UNSPECIFIED. ) ;
#15053 = CARTESIAN_POINT ( 'NONE',  ( -21.18564099849817239, 70.71717898851710515, -1.270000000000002682 ) ) ;
#15054 = CARTESIAN_POINT ( 'NONE',  ( -4.172034051875796123, 118.2392512717115665, 0.2176196316604530057 ) ) ;
#15055 = CARTESIAN_POINT ( 'NONE',  ( -23.42514220146296111, 142.8382549601284097, -0.4680900899253088721 ) ) ;
#15056 = ORIENTED_EDGE ( 'NONE', *, *, #34053, .F. ) ;
#15057 = CARTESIAN_POINT ( 'NONE',  ( -54.39768377094780760, 8.094885465611476150, 3.421923752996821833 ) ) ;
#15058 = CARTESIAN_POINT ( 'NONE',  ( -4.035982701929945016, 119.1815125624980425, -0.9242715903990733617 ) ) ;
#15059 = CARTESIAN_POINT ( 'NONE',  ( -4.333424916720135300, 104.6144662015457243, 3.954443799498177370 ) ) ;
#15061 = CARTESIAN_POINT ( 'NONE',  ( 4.301387610206993450, 118.2120950049252315, 0.4959387244165239794 ) ) ;
#15060 = AXIS2_PLACEMENT_3D ( 'NONE', #27064, #7059, #39218 ) ;
#15062 = CARTESIAN_POINT ( 'NONE',  ( -15.56852431296078976, 143.6313904367523833, -1.174399326838564184 ) ) ;
#15063 = CARTESIAN_POINT ( 'NONE',  ( -6.422645615570758970, 77.88548590848095898, -1.523999999999996469 ) ) ;
#15064 = DIRECTION ( 'NONE',  ( -1.000000000000000000, 0.000000000000000000, 0.000000000000000000 ) ) ;
#15065 = ORIENTED_EDGE ( 'NONE', *, *, #26982, .F. ) ;
#15066 = CARTESIAN_POINT ( 'NONE',  ( 3.465721614298269415, 18.43485028915299750, -3.064284189100199729 ) ) ;
#15067 = CARTESIAN_POINT ( 'NONE',  ( -32.57684172266954903, 51.47351799184504273, 1.270000000001143992 ) ) ;
#15068 = FACE_OUTER_BOUND ( 'NONE', #23922, .T. ) ;
#15069 = CARTESIAN_POINT ( 'NONE',  ( -42.66890350025247614, 21.80565315997285225, 1.797223148894693034 ) ) ;
#15070 = CARTESIAN_POINT ( 'NONE',  ( -28.92060043785469503, 77.33101988233063651, -1.524000000000008015 ) ) ;
#15071 = CARTESIAN_POINT ( 'NONE',  ( -6.996998182677447886, 121.8717014067360651, 0.1556392694547679423 ) ) ;
#15072 = CARTESIAN_POINT ( 'NONE',  ( -4.556403025205056245, 17.84477460162305107, -0.8067276567318153457 ) ) ;
#15073 = CARTESIAN_POINT ( 'NONE',  ( 1.957152676258774981, 116.9869758084673208, 0.4489687564533214603 ) ) ;
#15074 = CARTESIAN_POINT ( 'NONE',  ( -4.518622368304341386, 75.45558079800476037, -1.269999999999994911 ) ) ;
#15076 = CARTESIAN_POINT ( 'NONE',  ( 0.009931510163619200818, 117.7854482299006378, -0.4970133802592049954 ) ) ;
#15075 = CARTESIAN_POINT ( 'NONE',  ( 2.568134854143032442, -15.02010252187911554, 4.714990346623905815 ) ) ;
#15077 = CARTESIAN_POINT ( 'NONE',  ( -18.32188643113677884, 147.9371514012413229, 1.660510838394361866 ) ) ;
#15078 = CARTESIAN_POINT ( 'NONE',  ( 0.6341690014321406110, -14.98600045789189394, -0.7374838701073263003 ) ) ;
#15079 = CARTESIAN_POINT ( 'NONE',  ( -18.03394523526743143, 125.1493905788104684, -1.135097528960560265 ) ) ;
#15080 = CARTESIAN_POINT ( 'NONE',  ( 0.3717569628964236816, 23.89034148085472964, -0.9007439114964531646 ) ) ;
#15081 = VERTEX_POINT ( 'NONE', #10770 ) ;
#15082 = CARTESIAN_POINT ( 'NONE',  ( -56.37071950982826252, 3.976973756211601874, 2.203872415222109193 ) ) ;
#15083 = CARTESIAN_POINT ( 'NONE',  ( -15.94455450784152895, 146.9815093338748966, 0.4077454470555677002 ) ) ;
#15084 = CARTESIAN_POINT ( 'NONE',  ( 3.797208283716756227, -14.50848223276941873, 5.080264250175951624 ) ) ;
#15085 = CARTESIAN_POINT ( 'NONE',  ( 3.484775907859185562, 120.0787590019544098, -0.5801956493991065056 ) ) ;
#15086 = ORIENTED_EDGE ( 'NONE', *, *, #4976, .T. ) ;
#15087 = CARTESIAN_POINT ( 'NONE',  ( 1.824384274485360447, 115.7028213362407456, 1.722094561094771326 ) ) ;
#15088 = AXIS2_PLACEMENT_3D ( 'NONE', #2789, #22125, #1946 ) ;
#15089 = ORIENTED_EDGE ( 'NONE', *, *, #30807, .T. ) ;
#15090 = CARTESIAN_POINT ( 'NONE',  ( -4.720466306959788305, 117.9455647699196561, -0.8231657741585700627 ) ) ;
#15091 = CARTESIAN_POINT ( 'NONE',  ( 9.234582554329392678, 124.2544328994657405, 0.09881537413615872067 ) ) ;
#15092 = ORIENTED_EDGE ( 'NONE', *, *, #5930, .F. ) ;
#15093 = CARTESIAN_POINT ( 'NONE',  ( -0.01133701039344599780, 118.4098733054621277, 0.5673503590873753000 ) ) ;
#15094 = DIRECTION ( 'NONE',  ( -0.4849315768086480127, -0.8745520943968279060, -1.030032898892941415E-16 ) ) ;
#15095 = DIRECTION ( 'NONE',  ( -4.017660918040594346E-17, 1.000000000000000000, 2.376309959284834438E-19 ) ) ;
#15096 = DIRECTION ( 'NONE',  ( 5.188838149069472160E-16, -1.699382548006136559E-16, -1.000000000000000000 ) ) ;
#15097 = CARTESIAN_POINT ( 'NONE',  ( 15.14699153459420877, 156.1345691653134509, 0.01578391296358650636 ) ) ;
#15098 = VECTOR ( 'NONE', #31788, 1000.000000000000000 ) ;
#15099 = CARTESIAN_POINT ( 'NONE',  ( 0.1058213901577000071, 105.9761915687834772, -5.295735085524063024 ) ) ;
#15100 = CARTESIAN_POINT ( 'NONE',  ( 1.702391130740982028, -15.21670867692809281, 5.525181492016910667 ) ) ;
#15101 = CARTESIAN_POINT ( 'NONE',  ( 4.936888680085094627, 117.4097579285739954, 1.082126315060445876 ) ) ;
#15102 = CARTESIAN_POINT ( 'NONE',  ( -17.14499999999999957, 71.11999999999999034, -5.016499999999999737 ) ) ;
#15103 = CARTESIAN_POINT ( 'NONE',  ( -4.720046991804483838, 117.9726138801407274, 0.6354067178298792307 ) ) ;
#15104 = ORIENTED_EDGE ( 'NONE', *, *, #15920, .F. ) ;
#15105 = DIRECTION ( 'NONE',  ( -4.017660918040594346E-17, 1.000000000000000000, 2.376309959284834438E-19 ) ) ;
#15106 = CARTESIAN_POINT ( 'NONE',  ( -8.541944604652830009, 118.8311428792084712, -1.223721217923770199 ) ) ;
#15107 = CARTESIAN_POINT ( 'NONE',  ( -4.699507673534897734, 115.8251506319059843, -1.445723734630263824 ) ) ;
#15108 = CARTESIAN_POINT ( 'NONE',  ( 4.876145371826403618, 117.7132259977969539, 0.9242780742304819164 ) ) ;
#15109 = CARTESIAN_POINT ( 'NONE',  ( -4.612406548220088887, 117.9315729849519840, -0.9640725417016516863 ) ) ;
#15110 = CARTESIAN_POINT ( 'NONE',  ( -0.4234688608140231847, 124.8375573595198063, 0.002553167718424102610 ) ) ;
#15111 = CIRCLE ( 'NONE', #13794, 0.5080000000000002292 ) ;
#15112 = CARTESIAN_POINT ( 'NONE',  ( -1.251853189678833411, -4.679435864505671283, 4.458631606201990394 ) ) ;
#15113 = CARTESIAN_POINT ( 'NONE',  ( 11.66725022231030984, 17.14499999999999957, -5.016499999999999737 ) ) ;
#15114 = DIRECTION ( 'NONE',  ( 0.1728608224830406603, 1.098208118798718614E-16, -0.9849462604886047856 ) ) ;
#15115 = CARTESIAN_POINT ( 'NONE',  ( 3.292060170515798578, -12.34027101600769427, 0.7492661515550719242 ) ) ;
#15116 = CARTESIAN_POINT ( 'NONE',  ( 5.007645675277571762, 117.8491495069952748, -0.5952962186315862159 ) ) ;
#15117 = CARTESIAN_POINT ( 'NONE',  ( -17.14723838084594121, 144.2986879860016529, -2.167616513504174502 ) ) ;
#15118 = CARTESIAN_POINT ( 'NONE',  ( 5.091522377831856794, 117.1430865926791967, -0.3977369347680486666 ) ) ;
#15119 = CARTESIAN_POINT ( 'NONE',  ( -1.811248613112315553, 35.20749351892636980, 3.351885823999401381 ) ) ;
#15120 = CARTESIAN_POINT ( 'NONE',  ( -1.218981586993044042, 115.7029483214412693, 1.696095298325300593 ) ) ;
#15121 = CARTESIAN_POINT ( 'NONE',  ( -4.151662239014343392, 13.23730288530712862, 2.070234887608822572 ) ) ;
#15123 = ORIENTED_EDGE ( 'NONE', *, *, #41507, .T. ) ;
#15122 = CARTESIAN_POINT ( 'NONE',  ( 16.90643861817980209, 122.6916909566506320, 0.7822879649369941513 ) ) ;
#15124 = CARTESIAN_POINT ( 'NONE',  ( -1.823742538767885613, 105.1241012944524442, -5.023058958505786542 ) ) ;
#15125 = CARTESIAN_POINT ( 'NONE',  ( 3.762885361805711870, -15.68952731832974656, 3.843115198823321865 ) ) ;
#15126 = CARTESIAN_POINT ( 'NONE',  ( -18.33246729151856869, 150.1405190176936344, 1.740612831648467917 ) ) ;
#15127 = CARTESIAN_POINT ( 'NONE',  ( 0.8451309169872193161, 21.29487494764119759, 0.4837088869917456346 ) ) ;
#15128 = CARTESIAN_POINT ( 'NONE',  ( -0.9703616065139187841, 22.75662690174698355, -0.1248384507273650884 ) ) ;
#15129 = ORIENTED_EDGE ( 'NONE', *, *, #14947, .F. ) ;
#15130 = AXIS2_PLACEMENT_3D ( 'NONE', #39064, #9255, #12447 ) ;
#15131 = VERTEX_POINT ( 'NONE', #1000 ) ;
#15132 = CARTESIAN_POINT ( 'NONE',  ( -27.10368288468284348, 75.59070314479281194, -1.270000000000006679 ) ) ;
#15133 = CARTESIAN_POINT ( 'NONE',  ( 3.156357112953781741, 123.6198120039584154, 0.1457842492014824465 ) ) ;
#15134 = SURFACE_STYLE_USAGE ( .BOTH. , #18750 ) ;
#15135 = CARTESIAN_POINT ( 'NONE',  ( -16.75300165896971549, 146.9696287467501179, 1.108775417838743005 ) ) ;
#15136 = CARTESIAN_POINT ( 'NONE',  ( -6.654617103318593247E-14, 104.6144662015457243, 1.534725424433578570E-31 ) ) ;
#15137 = CARTESIAN_POINT ( 'NONE',  ( 3.514454466653502251, -13.37942318924494067, 2.559657187549406299 ) ) ;
#15138 = CARTESIAN_POINT ( 'NONE',  ( 5.507840079722706506, 156.5946142756450570, -1.582329182567087766 ) ) ;
#15139 = CARTESIAN_POINT ( 'NONE',  ( -10.11172965818669134, 120.4647147465577461, -1.576227610178517979 ) ) ;
#15140 = DIRECTION ( 'NONE',  ( -5.188838149069472160E-16, 1.699382548006136559E-16, 1.000000000000000000 ) ) ;
#15141 = EDGE_CURVE ( 'NONE', #909, #30579, #4312, .T. ) ;
#15142 = CARTESIAN_POINT ( 'NONE',  ( -15.26262975079004569, 148.0175730704188481, -0.3049836654608575892 ) ) ;
#15143 = CARTESIAN_POINT ( 'NONE',  ( -6.158966240078259879, 30.49883854570459718, 2.286114001711006871 ) ) ;
#15144 = CARTESIAN_POINT ( 'NONE',  ( 3.695597174621954029, 120.9852966486377710, -0.1212977071129681950 ) ) ;
#15145 = VERTEX_POINT ( 'NONE', #4822 ) ;
#15146 = CARTESIAN_POINT ( 'NONE',  ( 2.671714809844681238, -14.97371442308345380, 4.574436322856921144 ) ) ;
#15147 = FACE_OUTER_BOUND ( 'NONE', #41445, .T. ) ;
#15148 = CARTESIAN_POINT ( 'NONE',  ( -3.748619050207897985, 28.91994025391836942, 2.520532616727765518 ) ) ;
#15149 = CARTESIAN_POINT ( 'NONE',  ( -57.79605042197209031, 0.9991760233552228199, 1.356629168144736441 ) ) ;
#15150 = EDGE_CURVE ( 'NONE', #20685, #39579, #9726, .T. ) ;
#15151 = CARTESIAN_POINT ( 'NONE',  ( 3.793251108634954516, -14.54000584982637001, -2.652246991476435056 ) ) ;
#15152 = CARTESIAN_POINT ( 'NONE',  ( 13.40915985073331562, 130.9706359334022920, 1.586196205478585419 ) ) ;
#15153 = CARTESIAN_POINT ( 'NONE',  ( -2.549105041318592946, 30.42860202397990221, 3.618266982626868522 ) ) ;
#15154 = CARTESIAN_POINT ( 'NONE',  ( -3.079207415998597153, 107.8364052097302306, 4.350788137014373724 ) ) ;
#15155 = AXIS2_PLACEMENT_3D ( 'NONE', #10564, #20340, #23539 ) ;
#15156 = CARTESIAN_POINT ( 'NONE',  ( -1.825063964020108065, -4.879331645356781877, 4.256838567046823840 ) ) ;
#15157 = CARTESIAN_POINT ( 'NONE',  ( 8.981069108608807028, 123.9698733229553937, 0.1794631345465902139 ) ) ;
#15158 = CARTESIAN_POINT ( 'NONE',  ( 5.926391002875100789, -6.993723907645660098, 5.986726992520772228 ) ) ;
#15159 = CARTESIAN_POINT ( 'NONE',  ( -57.89731077922513691, 0.5615449381113218896, -1.034775302914740585E-14 ) ) ;
#15160 = CARTESIAN_POINT ( 'NONE',  ( 8.787644062751441609, 117.7645083475051422, -0.1261381370569843452 ) ) ;
#15161 = CARTESIAN_POINT ( 'NONE',  ( -0.4140400251256791120, 124.3520329708341023, -0.07144784443200472013 ) ) ;
#15162 = DIRECTION ( 'NONE',  ( 9.627370216492862708E-17, 1.000000000000000000, -0.000000000000000000 ) ) ;
#15163 = DIRECTION ( 'NONE',  ( -0.4849315768086535083, -0.8745520943968250194, -1.030032898892974695E-16 ) ) ;
#15164 = CARTESIAN_POINT ( 'NONE',  ( -0.8828713250188725548, -8.991384785216279596, -8.412059017423759499 ) ) ;
#15165 = CARTESIAN_POINT ( 'NONE',  ( 0.5456427185285884773, 117.3993834314738933, 1.492634212376517056 ) ) ;
#15166 = DIRECTION ( 'NONE',  ( -0.8745520943968249084, 0.4849315768086534528, -5.361993529360573944E-16 ) ) ;
#15167 = CARTESIAN_POINT ( 'NONE',  ( -6.639407854763120941E-14, 101.6934662015457320, 3.307182826377456566E-30 ) ) ;
#15168 = EDGE_CURVE ( 'NONE', #500, #9109, #33561, .T. ) ;
#15169 = CARTESIAN_POINT ( 'NONE',  ( 0.7687070661361545820, 118.7604188656930120, -0.8775891873661259002 ) ) ;
#15170 = CARTESIAN_POINT ( 'NONE',  ( -22.79600589338280514, 150.0845277111093310, 0.2694608383616130531 ) ) ;
#15171 = ORIENTED_EDGE ( 'NONE', *, *, #7183, .T. ) ;
#15172 = CARTESIAN_POINT ( 'NONE',  ( -58.05614784158871799, 2.052449344323428626, -0.2046694337772892169 ) ) ;
#15173 = ADVANCED_FACE ( 'NONE', ( #36563 ), #38989, .T. ) ;
#15174 = EDGE_LOOP ( 'NONE', ( #30115, #14673, #23645, #11852 ) ) ;
#15175 = FACE_OUTER_BOUND ( 'NONE', #29291, .T. ) ;
#15176 = AXIS2_PLACEMENT_3D ( 'NONE', #37243, #36835, #4049 ) ;
#15177 = CARTESIAN_POINT ( 'NONE',  ( -6.508431974736152092, 121.7798191570849440, -0.09215171978640852857 ) ) ;
#15178 = CARTESIAN_POINT ( 'NONE',  ( 5.947420766284201576, -14.61438673846185488, 1.993024607196187459 ) ) ;
#15179 = CARTESIAN_POINT ( 'NONE',  ( -14.68166051447203913, 123.3142630313093377, 1.213898157370195463 ) ) ;
#15180 = EDGE_CURVE ( 'NONE', #18529, #41231, #8629, .T. ) ;
#15181 = CARTESIAN_POINT ( 'NONE',  ( 22.12005076447803731, 142.1041199125429557, -1.010629163944517517 ) ) ;
#15182 = CARTESIAN_POINT ( 'NONE',  ( -3.640175008984333882, 11.51306413504884318, -2.862805987297033727 ) ) ;
#15183 = CARTESIAN_POINT ( 'NONE',  ( -13.33768363058614881, 156.9675713949798421, -0.6438986485269783122 ) ) ;
#15184 = CARTESIAN_POINT ( 'NONE',  ( -58.47923685707677777, 0.02532785185772538222, -0.7272094296869233698 ) ) ;
#15185 = CIRCLE ( 'NONE', #29931, 0.7620000000000000107 ) ;
#15186 = ORIENTED_EDGE ( 'NONE', *, *, #36531, .F. ) ;
#15187 = CARTESIAN_POINT ( 'NONE',  ( 2.184484440002603556, 116.2008805095703963, 0.07056628417267586661 ) ) ;
#15188 = CARTESIAN_POINT ( 'NONE',  ( -5.719305292821792008, 76.92870498041706639, -1.269999999999995799 ) ) ;
#15189 = CARTESIAN_POINT ( 'NONE',  ( -0.9105297513474850390, 157.1001331247151143, 1.431354397858309868 ) ) ;
#15190 = CARTESIAN_POINT ( 'NONE',  ( -48.88984042444451461, 17.95628636586173599, -5.089849583058218663 ) ) ;
#15191 = CARTESIAN_POINT ( 'NONE',  ( 13.67124846526806614, 154.1626644387825991, -1.747499485815532161 ) ) ;
#15192 = CARTESIAN_POINT ( 'NONE',  ( -13.72122979561089195, 121.8522644830672590, -1.670245716993636442 ) ) ;
#15193 = CARTESIAN_POINT ( 'NONE',  ( -55.73247374733729487, 5.492406230130003841, -2.854677165782116610 ) ) ;
#15194 = AXIS2_PLACEMENT_3D ( 'NONE', #24950, #23518, #24154 ) ;
#15195 = CARTESIAN_POINT ( 'NONE',  ( 9.374368624788175453, 123.5785764018267514, -0.4819391486299055560 ) ) ;
#15196 = ORIENTED_EDGE ( 'NONE', *, *, #18535, .F. ) ;
#15197 = CARTESIAN_POINT ( 'NONE',  ( -14.87841870982569148, 131.2528086460777388, -2.073644862699850933 ) ) ;
#15198 = CARTESIAN_POINT ( 'NONE',  ( 2.152540537132713538, -15.51301927577993034, 5.194954439406326507 ) ) ;
#15199 = CARTESIAN_POINT ( 'NONE',  ( -4.264711614227720382, 118.2128497746131330, -0.5330956542091240813 ) ) ;
#15200 = CARTESIAN_POINT ( 'NONE',  ( -58.11258158571958177, 1.603013069906233934, -1.501710181103033781 ) ) ;
#15201 = CARTESIAN_POINT ( 'NONE',  ( -10.15441061790785682, 81.86333342972157823, -1.269999999999998908 ) ) ;
#15202 = CARTESIAN_POINT ( 'NONE',  ( 5.349253755625428042, 156.5090806470891209, 1.752114854137454714 ) ) ;
#15203 = DIRECTION ( 'NONE',  ( 4.017660918040594346E-17, -1.000000000000000000, -2.376309959284834438E-19 ) ) ;
#15204 = CIRCLE ( 'NONE', #41745, 5.080000000000006288 ) ;
#15205 = CARTESIAN_POINT ( 'NONE',  ( -2.857158067608712493, -4.877720491018326499, 7.942258620001617864 ) ) ;
#15206 = CARTESIAN_POINT ( 'NONE',  ( 15.67344897587543251, 147.2319784351455780, 0.6427785636300454852 ) ) ;
#15207 = CARTESIAN_POINT ( 'NONE',  ( 0.7907840460254358383, 118.1535584534380661, -0.8818625303437642726 ) ) ;
#15208 = B_SPLINE_CURVE_WITH_KNOTS ( 'NONE', 3,
 ( #28795, #38802, #31782, #2827 ),
 .UNSPECIFIED., .F., .F.,
 ( 4, 4 ),
 ( 0.02831029896240152416, 1.000000000000000000 ),
 .UNSPECIFIED. ) ;
#15209 =( BOUNDED_CURVE ( )  B_SPLINE_CURVE ( 3, ( #14675, #28311, #40691, #18707 ),
 .UNSPECIFIED., .F., .T. ) 
 B_SPLINE_CURVE_WITH_KNOTS ( ( 4, 4 ),
 ( 0.6093138467282536164, 1.570796326794897002 ),
 .UNSPECIFIED. ) 
 CURVE ( )  GEOMETRIC_REPRESENTATION_ITEM ( )  RATIONAL_B_SPLINE_CURVE ( ( 1.000000000000000000, 0.9244349266169026302, 0.9244349266169026302, 1.000000000000000000 ) ) 
 REPRESENTATION_ITEM ( '' )  );
#15211 = EDGE_CURVE ( 'NONE', #3899, #22816, #7588, .T. ) ;
#15210 = CARTESIAN_POINT ( 'NONE',  ( 1.248107678658480997E-15, 12.96416000000000146, 0.000000000000000000 ) ) ;
#15212 = CARTESIAN_POINT ( 'NONE',  ( -0.7495039368703291238, 117.9394521389051249, 1.374537209560392936 ) ) ;
#15213 = CARTESIAN_POINT ( 'NONE',  ( -57.39043856515510811, 2.569568763584578974, 1.997829887931748427 ) ) ;
#15214 = CARTESIAN_POINT ( 'NONE',  ( -7.825995833725252204, 122.3857360859386461, -0.6413020235143477299 ) ) ;
#15215 = AXIS2_PLACEMENT_3D ( 'NONE', #12898, #38894, #9705 ) ;
#15216 = CARTESIAN_POINT ( 'NONE',  ( -58.37241122568484286, -0.2962816677227336770, -1.039428729632916517E-14 ) ) ;
#15217 = CARTESIAN_POINT ( 'NONE',  ( -51.24266872689721453, 19.11669921072455836, 1.581762766848667123 ) ) ;
#15218 = CARTESIAN_POINT ( 'NONE',  ( -23.35661798279360113, 142.7586093370927074, -0.2368412396931507957 ) ) ;
#15219 = ORIENTED_EDGE ( 'NONE', *, *, #3029, .T. ) ;
#15220 = CARTESIAN_POINT ( 'NONE',  ( -48.88162864671050301, 20.15829640254822408, -3.957548906738506123 ) ) ;
#15221 = CARTESIAN_POINT ( 'NONE',  ( -7.799325083925558566, 122.5293066583467834, -0.4363886786053240430 ) ) ;
#15222 = DIRECTION ( 'NONE',  ( -0.000000000000000000, 1.000000000000000000, 0.000000000000000000 ) ) ;
#15223 = CIRCLE ( 'NONE', #20664, 0.2540000000000038338 ) ;
#15224 = ORIENTED_EDGE ( 'NONE', *, *, #26070, .F. ) ;
#15225 = CARTESIAN_POINT ( 'NONE',  ( 2.969299016715368111, 115.7030432460468177, -1.557441274767545680 ) ) ;
#15227 = AXIS2_PLACEMENT_3D ( 'NONE', #15923, #35127, #12535 ) ;
#15226 = CARTESIAN_POINT ( 'NONE',  ( -4.562414174745367035, 121.1702857069421100, -0.2029539227048860195 ) ) ;
#15228 = CARTESIAN_POINT ( 'NONE',  ( 2.095434763668091005, -15.29852786734210746, 5.959135360315205077 ) ) ;
#15229 = CARTESIAN_POINT ( 'NONE',  ( -10.00431039430844038, 157.6892375622926181, 1.152258088200127872 ) ) ;
#15230 = CARTESIAN_POINT ( 'NONE',  ( -3.743815577281074614, 31.31851751214970037, -0.6207396561878217867 ) ) ;
#15231 = CARTESIAN_POINT ( 'NONE',  ( 1.414297571701309320, 159.6040221172770259, 0.1149235736256736529 ) ) ;
#15232 = EDGE_CURVE ( 'NONE', #1811, #5717, #33579, .T. ) ;
#15233 = CARTESIAN_POINT ( 'NONE',  ( 0.6461735126227318160, 120.9973616882760723, 0.04597716564786796106 ) ) ;
#15234 = CARTESIAN_POINT ( 'NONE',  ( 17.14499999999999957, 71.11999999999999034, 1.904999999999989146 ) ) ;
#15235 = CARTESIAN_POINT ( 'NONE',  ( -0.7403349074254782503, 24.03625360216656404, 0.6378939806667418555 ) ) ;
#15236 = CARTESIAN_POINT ( 'NONE',  ( -22.73177750447378642, 137.3553536570635742, -0.5243227317837020340 ) ) ;
#15237 = CARTESIAN_POINT ( 'NONE',  ( -41.28107547821697665, 23.22158991241121129, -1.524000000000029775 ) ) ;
#15238 = CARTESIAN_POINT ( 'NONE',  ( -10.28897677580358305, 57.14999999999998437, 4.381499999999999950 ) ) ;
#15239 = VERTEX_POINT ( 'NONE', #27173 ) ;
#15240 = CARTESIAN_POINT ( 'NONE',  ( -6.235261774140225199, 119.1541313481671551, 1.003364376444240813 ) ) ;
#15241 = DIRECTION ( 'NONE',  ( 0.9998004120163609398, 4.016384292689130894E-17, 0.01997839162482749689 ) ) ;
#15242 = CARTESIAN_POINT ( 'NONE',  ( 21.77023485109854306, 148.7205309135917730, 2.145821470179948953 ) ) ;
#15243 = CARTESIAN_POINT ( 'NONE',  ( 13.04666149862676860, 122.0079276396459704, -1.242691380407616286 ) ) ;
#15244 = CARTESIAN_POINT ( 'NONE',  ( -4.534963259934312596, 26.26729952004485824, -7.114490783490484027 ) ) ;
#15245 = CARTESIAN_POINT ( 'NONE',  ( -14.37796933089572171, 121.0470547900126519, -1.299527359048518793 ) ) ;
#15246 = CARTESIAN_POINT ( 'NONE',  ( 4.924141663657016110, 117.6632128302819780, -0.7819755836232500368 ) ) ;
#15247 = CARTESIAN_POINT ( 'NONE',  ( 0.6688473404177899262, 105.9455060897651748, 5.311925200740537534 ) ) ;
#15248 = CARTESIAN_POINT ( 'NONE',  ( -12.91960671971527042, 133.8340822528099636, -0.1412842392263897739 ) ) ;
#15249 = CARTESIAN_POINT ( 'NONE',  ( -5.835242038117813834, 119.5807162246413498, -1.179424802705185238 ) ) ;
#15250 = CARTESIAN_POINT ( 'NONE',  ( 6.376069600431401696, -13.97715805579494130, 0.6469259796868158663 ) ) ;
#15251 = CARTESIAN_POINT ( 'NONE',  ( -12.87096146653068196, 58.93153423982063543, -10.60403923708992835 ) ) ;
#15252 = CARTESIAN_POINT ( 'NONE',  ( 4.968814169093906941, 56.51947256399660802, 4.801687862347802316 ) ) ;
#15253 = ORIENTED_EDGE ( 'NONE', *, *, #37950, .T. ) ;
#15254 = CARTESIAN_POINT ( 'NONE',  ( 11.93340282868940960, 123.0912118827050108, 1.763528850166467432 ) ) ;
#15255 = DIRECTION ( 'NONE',  ( -0.8745520943968243532, 0.4849315768086547296, -6.829619984160642269E-16 ) ) ;
#15256 = CARTESIAN_POINT ( 'NONE',  ( -1.527851852856435766, 118.1343055320472928, -0.9288516185665885994 ) ) ;
#15257 = CARTESIAN_POINT ( 'NONE',  ( -1.979347617175880147, 122.1523088006674840, 0.1944583918105484699 ) ) ;
#15258 = CARTESIAN_POINT ( 'NONE',  ( -6.116428202004375869, -11.74185255526443505, -5.788024375304219760 ) ) ;
#15259 = CARTESIAN_POINT ( 'NONE',  ( 15.64597882779391114, 147.9168465093495399, 1.159024332450872663 ) ) ;
#15260 = CARTESIAN_POINT ( 'NONE',  ( -4.770965495274668733, 118.5930653697794384, -0.9879445655740133336 ) ) ;
#15261 = CARTESIAN_POINT ( 'NONE',  ( 10.59335592519045299, 157.9214973357695158, -0.4646299181629826580 ) ) ;
#15262 = CARTESIAN_POINT ( 'NONE',  ( 5.322311913656744942, 57.14999999999977831, -5.239113282063458499 ) ) ;
#15263 = CARTESIAN_POINT ( 'NONE',  ( -58.16454994639720155, 0.1482675199355112661, 0.6170558006857020938 ) ) ;
#15264 = DIRECTION ( 'NONE',  ( -0.8745520943968548844, 0.4849315768085996070, -4.268512490100397104E-16 ) ) ;
#15265 = DIRECTION ( 'NONE',  ( 4.017660918040594346E-17, -1.000000000000000000, -2.376309959284834438E-19 ) ) ;
#15266 = CARTESIAN_POINT ( 'NONE',  ( -4.293957123808202603, 118.2142473212576164, 0.3502411785888445150 ) ) ;
#15267 = CARTESIAN_POINT ( 'NONE',  ( -20.51686376604223128, 129.1072961674477710, -0.4099757654675939000 ) ) ;
#15268 = VERTEX_POINT ( 'NONE', #40184 ) ;
#15269 = CARTESIAN_POINT ( 'NONE',  ( -54.12303657725384198, 9.464413707472848714, 3.807237671326749506 ) ) ;
#15270 = EDGE_CURVE ( 'NONE', #14618, #35734, #21807, .T. ) ;
#15271 = CARTESIAN_POINT ( 'NONE',  ( -6.278307647342964870, 119.9169151369681430, -1.219481925155367907 ) ) ;
#15272 = CARTESIAN_POINT ( 'NONE',  ( -10.19284229789036900, 16.51000000000000156, 4.908176479697702099 ) ) ;
#15273 = CARTESIAN_POINT ( 'NONE',  ( -5.218277051435869396, 121.1607713875043117, -0.4468594773273020793 ) ) ;
#15274 = CARTESIAN_POINT ( 'NONE',  ( 4.999199951152328403, 117.4030387777868469, -0.8341129481215795449 ) ) ;
#15275 = CYLINDRICAL_SURFACE ( 'NONE', #7600, 0.2539999999999956737 ) ;
#15276 = EDGE_CURVE ( 'NONE', #37721, #24344, #20763, .T. ) ;
#15277 = ORIENTED_EDGE ( 'NONE', *, *, #4825, .F. ) ;
#15278 = CARTESIAN_POINT ( 'NONE',  ( -3.854280124997887746, 21.23357344512866973, -2.551540157904111261 ) ) ;
#15279 = CARTESIAN_POINT ( 'NONE',  ( -29.61277755921473442, 68.29894143241583038, 1.270000000001148877 ) ) ;
#15280 = DIRECTION ( 'NONE',  ( 0.9575201071113178530, -0.2883665106726683858, 8.537024980200786319E-16 ) ) ;
#15281 = DIRECTION ( 'NONE',  ( -5.188838149069472160E-16, 1.699382548006136559E-16, 1.000000000000000000 ) ) ;
#15282 = CARTESIAN_POINT ( 'NONE',  ( -41.08172402297545744, 23.06268970575965938, 1.270028526666263646 ) ) ;
#15283 = CARTESIAN_POINT ( 'NONE',  ( 7.790228995712999094, 122.5851452327640772, 0.3185712494481027224 ) ) ;
#15284 = CARTESIAN_POINT ( 'NONE',  ( 2.264360804680111805, 21.29314879275315064, 4.027482774281332389 ) ) ;
#15285 = CARTESIAN_POINT ( 'NONE',  ( 15.38653228232027992, 121.5363848317736739, 1.155577132538254670 ) ) ;
#15286 = CARTESIAN_POINT ( 'NONE',  ( 2.051927835239828024, 104.6144662015457243, -4.377228190977056954 ) ) ;
#15288 = CARTESIAN_POINT ( 'NONE',  ( 2.147481372520596121, 117.7847241295267651, -0.6070331404035437250 ) ) ;
#15287 = CARTESIAN_POINT ( 'NONE',  ( 3.092642723064080279, -14.67800799544728285, 3.675123631970977911 ) ) ;
#15289 = CARTESIAN_POINT ( 'NONE',  ( -12.44264023681993869, 124.1810962131942517, 1.301390444852660755 ) ) ;
#15290 = CARTESIAN_POINT ( 'NONE',  ( 4.610398055573782905, 23.01736123548795021, -0.3254830233858732602 ) ) ;
#15291 = CARTESIAN_POINT ( 'NONE',  ( -15.18175346423898198, 121.1469641333237917, -1.070035192906481081 ) ) ;
#15292 = CARTESIAN_POINT ( 'NONE',  ( -0.9660709935815289251, 7.903159174923253261, 0.1333004412508401459 ) ) ;
#15293 = EDGE_LOOP ( 'NONE', ( #24765, #3616, #13927, #17951 ) ) ;
#15294 = CARTESIAN_POINT ( 'NONE',  ( -57.24575050778504703, 1.871741192705528301, 0.5496743666258914196 ) ) ;
#15295 = CARTESIAN_POINT ( 'NONE',  ( -15.92043486079658088, 145.9828583539951126, 0.2780828054990249765 ) ) ;
#15296 = CARTESIAN_POINT ( 'NONE',  ( 4.383797612528895549, -14.46967269938057044, 4.720428574551663203 ) ) ;
#15297 = CARTESIAN_POINT ( 'NONE',  ( 3.430652046320601389, 156.3978305292817481, -1.152991164011112346 ) ) ;
#15298 = ORIENTED_EDGE ( 'NONE', *, *, #14908, .T. ) ;
#15299 = CARTESIAN_POINT ( 'NONE',  ( 1.786958751275772306, 115.7029469026952029, 1.723307358492499830 ) ) ;
#15300 = ORIENTED_EDGE ( 'NONE', *, *, #25522, .F. ) ;
#15301 = CARTESIAN_POINT ( 'NONE',  ( -4.815518961581000568, 117.8246686530165448, -0.8829384762845114976 ) ) ;
#15302 = CARTESIAN_POINT ( 'NONE',  ( 5.945776936743700780, 121.5465042053001667, 0.1188107733588234516 ) ) ;
#15304 = EDGE_LOOP ( 'NONE', ( #9423, #15089, #6568, #18157 ) ) ;
#15303 = CIRCLE ( 'NONE', #1076, 0.2539999999999956737 ) ;
#15305 = CARTESIAN_POINT ( 'NONE',  ( 19.26131898708108992, 149.3473233412102275, 2.496341295301664598 ) ) ;
#15306 = CARTESIAN_POINT ( 'NONE',  ( -3.174366308152012817, 84.67546620154573134, -0.06343139340882732180 ) ) ;
#15307 = DIRECTION ( 'NONE',  ( 5.188838149069472160E-16, -1.699382548006136559E-16, -1.000000000000000000 ) ) ;
#15308 = ADVANCED_BREP_SHAPE_REPRESENTATION ( '', ( #24724, #3275 ), #9399 ) ;
#15309 = CARTESIAN_POINT ( 'NONE',  ( 4.949796331672161820, 117.4773373787071193, -0.8984534372031296456 ) ) ;
#15310 = CARTESIAN_POINT ( 'NONE',  ( 22.63314285866076858, 150.6357905964555925, 0.1239933314926730257 ) ) ;
#15311 = CARTESIAN_POINT ( 'NONE',  ( 12.69999999999999929, 14.60500000000000043, 1.555301434917138235E-15 ) ) ;
#15312 = CARTESIAN_POINT ( 'NONE',  ( -10.96186877710140273, 56.39406130473899736, 5.016500000001508752 ) ) ;
#15313 = CARTESIAN_POINT ( 'NONE',  ( 1.957116903647192263, -15.34957576579747140, 5.354569344195124536 ) ) ;
#15314 = CARTESIAN_POINT ( 'NONE',  ( -45.39816439898302036, 21.06106408185672763, 4.080402960186377825 ) ) ;
#15315 = CARTESIAN_POINT ( 'NONE',  ( -28.92060043785469503, 77.33101988233063651, 1.269999999999991136 ) ) ;
#15316 = CARTESIAN_POINT ( 'NONE',  ( -4.678029067978729749, 117.8847919582286465, 0.8180832583663835145 ) ) ;
#15317 = VERTEX_POINT ( 'NONE', #40390 ) ;
#15318 = ORIENTED_EDGE ( 'NONE', *, *, #10042, .T. ) ;
#15319 = CARTESIAN_POINT ( 'NONE',  ( 4.850929972935443146, 117.7610086971114356, 0.9074237114610381738 ) ) ;
#15320 = CARTESIAN_POINT ( 'NONE',  ( 5.722844102788878118, 118.5195176813615063, -0.9755545356960315662 ) ) ;
#15321 = CARTESIAN_POINT ( 'NONE',  ( -1.025137579952785094, 106.6134986179334589, -5.027802332087124348 ) ) ;
#15322 = CARTESIAN_POINT ( 'NONE',  ( 4.899053217361366563, 117.6324216922197365, 0.9917945611932356131 ) ) ;
#15323 = CARTESIAN_POINT ( 'NONE',  ( -13.85159022459153988, 12.96416000000000146, 5.016499999999999737 ) ) ;
#15324 = CARTESIAN_POINT ( 'NONE',  ( -0.7690845662406576855, 119.7070660435176279, 0.6575911349602957534 ) ) ;
#15325 = CARTESIAN_POINT ( 'NONE',  ( -1.504723661876595786, -8.552649586842417051, -4.374500482163298898 ) ) ;
#15326 = CARTESIAN_POINT ( 'NONE',  ( -58.70413935429054675, 0.2332485698458008905, 0.6626129746612758886 ) ) ;
#15327 = DIRECTION ( 'NONE',  ( 1.000000000000000000, 0.000000000000000000, 1.224646799147354933E-16 ) ) ;
#15328 = CARTESIAN_POINT ( 'NONE',  ( 3.604966970014626959, -13.82400766246429136, 3.906450875976586801 ) ) ;
#15329 = CARTESIAN_POINT ( 'NONE',  ( 7.618479139564604985, 124.9344662015457317, 0.1522353441811855612 ) ) ;
#15330 = CARTESIAN_POINT ( 'NONE',  ( -8.888678185457033365, 122.0520977060996586, -1.259005013942402718 ) ) ;
#15331 = EDGE_CURVE ( 'NONE', #41136, #1859, #32911, .T. ) ;
#15332 = CARTESIAN_POINT ( 'NONE',  ( 5.152689472752729039, 116.8412042436348912, 0.1029629964107459106 ) ) ;
#15333 = CARTESIAN_POINT ( 'NONE',  ( -0.02244247360070318262, 39.09286639261657115, 1.286999615499952787 ) ) ;
#15334 = CIRCLE ( 'NONE', #9246, 8.794749999999993406 ) ;
#15335 = CARTESIAN_POINT ( 'NONE',  ( -1.627051029834679419, 115.7027888630229171, 1.667098993452897693 ) ) ;
#15336 = CARTESIAN_POINT ( 'NONE',  ( 1.068493265602401987, 5.690783753869971484, 4.496582723949734017 ) ) ;
#15338 = ORIENTED_EDGE ( 'NONE', *, *, #42104, .F. ) ;
#15337 = CARTESIAN_POINT ( 'NONE',  ( 15.81407516854438100, 121.2341309109925334, 0.7422539548746110993 ) ) ;
#15339 = CARTESIAN_POINT ( 'NONE',  ( 0.2402493194813784261, 105.1224165606177365, -5.340051935206860279 ) ) ;
#15340 = CARTESIAN_POINT ( 'NONE',  ( 4.100156219318407125, -15.52122063102406813, 2.251114749721512709 ) ) ;
#15341 = CARTESIAN_POINT ( 'NONE',  ( -12.31762543427507417, 122.6846661264431191, 1.317417697584883030 ) ) ;
#15342 = CARTESIAN_POINT ( 'NONE',  ( 0.7093541224826089842, 23.24201423063343697, -0.6674325600367136957 ) ) ;
#15343 = CARTESIAN_POINT ( 'NONE',  ( -0.7472855871240335901, 21.88424109716052612, -0.6269268744489370215 ) ) ;
#15344 = ORIENTED_EDGE ( 'NONE', *, *, #25847, .T. ) ;
#15345 = ORIENTED_EDGE ( 'NONE', *, *, #32407, .T. ) ;
#15346 = CARTESIAN_POINT ( 'NONE',  ( -41.05189575270519242, 23.09451173561983950, 0.4656666666666613996 ) ) ;
#15347 = CARTESIAN_POINT ( 'NONE',  ( 1.486515533885975016, 107.1743931308027129, 4.786382923486936392 ) ) ;
#15348 = SHAPE_REPRESENTATION_RELATIONSHIP ( 'NONE' , 'NONE' ,  #23419, #15308 ) ;
#15349 = CARTESIAN_POINT ( 'NONE',  ( -1.514956540612282021, 120.4980338609919386, 0.3173598453907558459 ) ) ;
#15350 = CARTESIAN_POINT ( 'NONE',  ( 5.586884702347365561, 68.92746620154572668, 0.1116392523995368286 ) ) ;
#15351 = CARTESIAN_POINT ( 'NONE',  ( 3.497624268394256219, -13.57517324819364291, 2.900746184505403669 ) ) ;
#15352 = CARTESIAN_POINT ( 'NONE',  ( 18.00357552251023563, 146.8415343102147972, -1.578964580512862925 ) ) ;
#15353 = CARTESIAN_POINT ( 'NONE',  ( -1.082660538731543776, 158.4310823543925721, -1.603207764552046832 ) ) ;
#15354 = CARTESIAN_POINT ( 'NONE',  ( -5.586884702347496123, 79.34146620154574236, -0.1116392523995361624 ) ) ;
#15355 = CARTESIAN_POINT ( 'NONE',  ( 3.047145566129288330, -14.72663143740328806, 3.823360744794035870 ) ) ;
#15356 = CARTESIAN_POINT ( 'NONE',  ( -0.01632536679074420016, 38.84944212800221663, 1.323018725044088573 ) ) ;
#15357 = CARTESIAN_POINT ( 'NONE',  ( 7.620757776630359359, 122.3831840716419066, -0.1218999176909028453 ) ) ;
#15358 = ORIENTED_EDGE ( 'NONE', *, *, #15764, .T. ) ;
#15359 = CARTESIAN_POINT ( 'NONE',  ( -0.4436142255061583661, 106.0194232803738998, -5.281734587570124262 ) ) ;
#15360 = DIRECTION ( 'NONE',  ( -0.9816537812491126225, -0.1906721105964872265, -8.537024980200846470E-16 ) ) ;
#15361 = PLANE ( 'NONE',  #2819 ) ;
#15362 = CARTESIAN_POINT ( 'NONE',  ( -58.47668496617072975, -0.4796687618228244743, 0.2989310191336559952 ) ) ;
#15363 = TOROIDAL_SURFACE ( 'NONE', #30357, 2.286000000000000032, 0.2540000000000000036 ) ;
#15364 = CARTESIAN_POINT ( 'NONE',  ( -3.436282163690115077, 26.04026231355703658, -7.687665148811276161 ) ) ;
#15365 = CARTESIAN_POINT ( 'NONE',  ( -0.02156534543299366835, 156.6359106937186709, 1.079218069903262744 ) ) ;
#15366 = CARTESIAN_POINT ( 'NONE',  ( -17.65389921742010060, 84.42347906515803402, 1.269999999999995799 ) ) ;
#15367 = CARTESIAN_POINT ( 'NONE',  ( 15.52360445758504426, 120.7153972339879715, 0.2596658046059213687 ) ) ;
#15368 = EDGE_CURVE ( 'NONE', #15239, #9633, #17237, .T. ) ;
#15369 = CARTESIAN_POINT ( 'NONE',  ( -1.571019246621560450, 106.2535611835979239, 5.108158685570669988 ) ) ;
#15370 = CARTESIAN_POINT ( 'NONE',  ( -3.609430071560130848, 3.966570591990036032, 2.889066364458971137 ) ) ;
#15371 = CARTESIAN_POINT ( 'NONE',  ( 15.77133435453283461, 146.5691041611200660, 0.3151487940933137555 ) ) ;
#15372 = EDGE_CURVE ( 'NONE', #2842, #4427, #8836, .T. ) ;
#15373 = CARTESIAN_POINT ( 'NONE',  ( 3.135079784281773918, -3.970030566872769562, -7.817010796087090263 ) ) ;
#15374 = CARTESIAN_POINT ( 'NONE',  ( -56.88731995051696089, 2.378615435641953546, -0.1283520312635632321 ) ) ;
#15375 = CARTESIAN_POINT ( 'NONE',  ( -2.148722934776839288, 116.3868840314291475, -0.3193016367261526933 ) ) ;
#15376 = CARTESIAN_POINT ( 'NONE',  ( -0.8285762425324525449, 121.5536190086353372, -0.3701497059917958632 ) ) ;
#15377 = DIRECTION ( 'NONE',  ( 0.01731298258487451447, -0.9998501190848635423, 1.788962107505245826E-16 ) ) ;
#15378 = CARTESIAN_POINT ( 'NONE',  ( -19.86616884172038766, 72.62886460123898758, -1.270000000000002460 ) ) ;
#15379 = CARTESIAN_POINT ( 'NONE',  ( -0.3239230800893593276, 29.42979164457532804, -4.628216972995994993 ) ) ;
#15380 = CARTESIAN_POINT ( 'NONE',  ( 0.6796407112084186242, 118.1588882304778423, 0.9027520341413136640 ) ) ;
#15381 = CARTESIAN_POINT ( 'NONE',  ( -6.135835944515187101, 77.40800365160224317, 1.270000000000003793 ) ) ;
#15382 = DIRECTION ( 'NONE',  ( -5.188838149069472160E-16, 1.699382548006136559E-16, 1.000000000000000000 ) ) ;
#15383 = EDGE_CURVE ( 'NONE', #17144, #17052, #9097, .T. ) ;
#15384 = CARTESIAN_POINT ( 'NONE',  ( 0.3799753109754416269, 121.9236798544226730, -0.3295597595137199631 ) ) ;
#15385 = CARTESIAN_POINT ( 'NONE',  ( -13.24393851483428719, 156.9672759736256467, 0.3459722171078645769 ) ) ;
#15386 = ORIENTED_EDGE ( 'NONE', *, *, #37572, .F. ) ;
#15387 = CARTESIAN_POINT ( 'NONE',  ( -5.809227842914839179, 77.60418761620948658, 1.270000000000003126 ) ) ;
#15388 = VERTEX_POINT ( 'NONE', #31408 ) ;
#15389 = DIRECTION ( 'NONE',  ( -5.188838149069472160E-16, 1.699382548006136559E-16, 1.000000000000000000 ) ) ;
#15390 = CARTESIAN_POINT ( 'NONE',  ( -14.13522066970473112, 138.8284419781823829, -0.1497975941480006734 ) ) ;
#15391 = CARTESIAN_POINT ( 'NONE',  ( 4.849545180983690251, -15.35966036743073637, 3.882997576023691444 ) ) ;
#15392 = CARTESIAN_POINT ( 'NONE',  ( -20.72967856921748009, 148.2641884961211076, 1.615940018417327817 ) ) ;
#15393 = CARTESIAN_POINT ( 'NONE',  ( 21.94752568715507834, 149.4141677464492091, -1.146579238551070468 ) ) ;
#15394 = CARTESIAN_POINT ( 'NONE',  ( -3.130497002865707312, 23.39511390029671745, 3.426874451367011520 ) ) ;
#15395 = AXIS2_PLACEMENT_3D ( 'NONE', #40871, #7869, #8067 ) ;
#15396 = CARTESIAN_POINT ( 'NONE',  ( -15.30459713313471681, 120.6995131204970875, -0.6235550965980859450 ) ) ;
#15397 = CARTESIAN_POINT ( 'NONE',  ( -54.11170070365439955, 9.036272999044422605, -3.680880771591853229 ) ) ;
#15398 = EDGE_CURVE ( 'NONE', #32706, #11324, #14997, .T. ) ;
#15399 = ORIENTED_EDGE ( 'NONE', *, *, #39258, .F. ) ;
#15400 = CIRCLE ( 'NONE', #9303, 0.7620000000000000107 ) ;
#15401 = CARTESIAN_POINT ( 'NONE',  ( 0.3665064675491350177, 121.9236798544226730, 0.3444762419765421968 ) ) ;
#15402 = CARTESIAN_POINT ( 'NONE',  ( -5.134369219808014861, 120.3680889145531552, 0.6721547394862481539 ) ) ;
#15403 = CARTESIAN_POINT ( 'NONE',  ( -51.39111418837354961, 13.76717004397113087, -4.421739674169018031 ) ) ;
#15404 = CARTESIAN_POINT ( 'NONE',  ( 11.73216920131852881, 154.7938929448963279, -1.733846838993656325 ) ) ;
#15405 = CARTESIAN_POINT ( 'NONE',  ( -17.48279436891391114, 128.5781302034472162, -2.030760391889158800 ) ) ;
#15406 = CARTESIAN_POINT ( 'NONE',  ( -49.13940628111213016, 17.59503125033257120, -5.062072503518689537 ) ) ;
#15407 = CARTESIAN_POINT ( 'NONE',  ( 12.35517153206324181, 152.0262389575480881, -0.8038591168380518903 ) ) ;
#15408 = EDGE_LOOP ( 'NONE', ( #28304, #34498, #33384, #20140 ) ) ;
#15409 = CARTESIAN_POINT ( 'NONE',  ( -0.8698789912703093208, 157.1975648536147787, -1.511617766987151334 ) ) ;
#15410 = CARTESIAN_POINT ( 'NONE',  ( 4.433333709997448580, -15.52846643035468688, 1.874498299855786421 ) ) ;
#15411 = CARTESIAN_POINT ( 'NONE',  ( -4.105428725848253357, 118.2429491485453070, -0.3529517962327167191 ) ) ;
#15412 = EDGE_CURVE ( 'NONE', #29525, #18747, #12471, .T. ) ;
#15413 = CARTESIAN_POINT ( 'NONE',  ( -57.64973313486724038, 1.352533784701764885, -1.499908592384923134 ) ) ;
#15414 = CARTESIAN_POINT ( 'NONE',  ( -4.996941175475388519, 117.4672098027941303, 0.7805663078437622415 ) ) ;
#15415 = CARTESIAN_POINT ( 'NONE',  ( -0.02874415600673332558, 157.0795416643300939, 1.438475106415294302 ) ) ;
#15416 = DIRECTION ( 'NONE',  ( 1.000000000000000000, 0.000000000000000000, -6.146657985744592735E-16 ) ) ;
#15417 = AXIS2_PLACEMENT_3D ( 'NONE', #8463, #1868, #34657 ) ;
#15418 = ADVANCED_FACE ( 'NONE', ( #14578 ), #41197, .F. ) ;
#15419 = CARTESIAN_POINT ( 'NONE',  ( -8.268995186617910775, -7.056286353048313309, -1.660136952399225319 ) ) ;
#15420 = CARTESIAN_POINT ( 'NONE',  ( 10.39558336183860021, 126.0814211662656419, 0.4651924986760612724 ) ) ;
#15421 = CARTESIAN_POINT ( 'NONE',  ( 1.563499521607991438, 118.1343052102891988, -0.8670908977950454455 ) ) ;
#15422 = AXIS2_PLACEMENT_3D ( 'NONE', #1318, #10464, #30264 ) ;
#15424 = ORIENTED_EDGE ( 'NONE', *, *, #991, .T. ) ;
#15423 = CARTESIAN_POINT ( 'NONE',  ( -41.05189575270519242, 23.09451173561982174, -0.2116666666666723873 ) ) ;
#15425 = CARTESIAN_POINT ( 'NONE',  ( -0.02812206017517816792, 117.9394518360233519, 1.407342955188501943 ) ) ;
#15426 = CARTESIAN_POINT ( 'NONE',  ( -56.71132732703541990, 3.319205314284062958, 2.191228219141345246 ) ) ;
#15427 = CARTESIAN_POINT ( 'NONE',  ( -53.06925326111847596, 10.99994025872287118, 4.072059781937412914 ) ) ;
#15428 = LINE ( 'NONE', #8418, #1161 ) ;
#15429 = CARTESIAN_POINT ( 'NONE',  ( -5.965356522962928842, 65.30181249999998272, -5.016499999999999737 ) ) ;
#15430 = CARTESIAN_POINT ( 'NONE',  ( -50.42190507837991476, 20.37545339363690999, 1.629190407695419784 ) ) ;
#15431 = CARTESIAN_POINT ( 'NONE',  ( -5.733252156539744071, 159.1225378944267845, 0.03759195597257692506 ) ) ;
#15432 = ORIENTED_EDGE ( 'NONE', *, *, #15331, .T. ) ;
#15433 = CARTESIAN_POINT ( 'NONE',  ( -49.18824384045164777, 22.20099125052343680, -1.469723468883198825 ) ) ;
#15434 = CARTESIAN_POINT ( 'NONE',  ( -6.919813487662133333, 121.8949882256362827, -0.3984175079523645246 ) ) ;
#15435 = CARTESIAN_POINT ( 'NONE',  ( -7.966529119767051803, 121.8269078720122565, 0.7202784793016417941 ) ) ;
#15436 = ORIENTED_EDGE ( 'NONE', *, *, #37538, .T. ) ;
#15437 = CARTESIAN_POINT ( 'NONE',  ( 1.232143138580572783, 115.7029489553663808, -1.695162972283317249 ) ) ;
#15438 = CARTESIAN_POINT ( 'NONE',  ( -10.25892126925259085, 126.0184183664171655, -0.2980827979995013255 ) ) ;
#15439 = CARTESIAN_POINT ( 'NONE',  ( 2.450443274655972559, -15.26395620497007855, 5.889056594049635329 ) ) ;
#15440 = CARTESIAN_POINT ( 'NONE',  ( -5.066682439019665196, 158.5910778905036977, 1.349075717862105783 ) ) ;
#15441 = DIRECTION ( 'NONE',  ( -0.1548639604663282210, -0.9876883405951374373, 0.02211098372092801939 ) ) ;
#15442 = CARTESIAN_POINT ( 'NONE',  ( 0.9122582399080617632, 116.5216256635990391, 0.1489946802529018843 ) ) ;
#15443 = AXIS2_PLACEMENT_3D ( 'NONE', #21759, #18575, #4987 ) ;
#15444 = CARTESIAN_POINT ( 'NONE',  ( 7.042656930656880476, 122.0730845385896544, 0.2183737125472967333 ) ) ;
#15445 = CARTESIAN_POINT ( 'NONE',  ( -17.32429653712378936, 61.56493206124108042, 1.269999999999999796 ) ) ;
#15446 = CARTESIAN_POINT ( 'NONE',  ( -0.9542339719106045504, 13.68595756868040603, 0.2091889690632084686 ) ) ;
#15447 = CARTESIAN_POINT ( 'NONE',  ( -3.725034515352510844, 116.6403000632267464, -0.1520601685204151510 ) ) ;
#15448 = DIRECTION ( 'NONE',  ( 5.188838149069472160E-16, -1.699382548006136559E-16, -1.000000000000000000 ) ) ;
#15449 = EDGE_CURVE ( 'NONE', #20737, #37727, #6378, .T. ) ;
#15450 = DIRECTION ( 'NONE',  ( -1.000000000000000000, 1.365923996832131856E-16, 0.000000000000000000 ) ) ;
#15451 = ORIENTED_EDGE ( 'NONE', *, *, #37372, .T. ) ;
#15452 = CARTESIAN_POINT ( 'NONE',  ( -3.743659292024924756, 118.0176333062828320, 0.7744886050550696677 ) ) ;
#15453 = LINE ( 'NONE', #37409, #14322 ) ;
#15454 = CARTESIAN_POINT ( 'NONE',  ( 17.05973152613361066, 125.2153959547233910, 1.608365543201426773 ) ) ;
#15455 = AXIS2_PLACEMENT_3D ( 'NONE', #7583, #26540, #26958 ) ;
#15456 = CARTESIAN_POINT ( 'NONE',  ( 11.48785675552145591, 156.2473422840488979, -1.634126210350451469 ) ) ;
#15457 = CARTESIAN_POINT ( 'NONE',  ( 3.518211725887771202, 24.73955407011506935, -7.658871095584262711 ) ) ;
#15458 = CARTESIAN_POINT ( 'NONE',  ( -3.017629403179087788, 159.2229145144301867, -1.079859862993577391 ) ) ;
#15459 = CARTESIAN_POINT ( 'NONE',  ( 4.781198548879745047, 117.7628531851493534, -0.8766415564179582676 ) ) ;
#15460 = CARTESIAN_POINT ( 'NONE',  ( 5.928176885185626688, 118.9717589635377664, 0.5867527899620113008 ) ) ;
#15461 = AXIS2_PLACEMENT_3D ( 'NONE', #12357, #25344, #19560 ) ;
#15462 = CARTESIAN_POINT ( 'NONE',  ( -8.074187567049014191, 122.8559727437779827, -0.08249527776860599015 ) ) ;
#15463 = CARTESIAN_POINT ( 'NONE',  ( -11.78639615006497365, 122.5845257805695923, -1.760937685738447334 ) ) ;
#15464 = CARTESIAN_POINT ( 'NONE',  ( 6.422280156622033331, -13.89829431882434818, 0.3667318345078443564 ) ) ;
#15465 = CARTESIAN_POINT ( 'NONE',  ( -15.27962295839633811, 80.49293118800726177, 1.523999999999998023 ) ) ;
#15466 = CARTESIAN_POINT ( 'NONE',  ( -42.09814309847200064, 23.46876350539121248, -1.524000000000005794 ) ) ;
#15467 = ORIENTED_EDGE ( 'NONE', *, *, #2134, .F. ) ;
#15468 = CARTESIAN_POINT ( 'NONE',  ( 16.55752258724309911, 151.1890201267100906, 2.396410905537823766 ) ) ;
#15469 = DIRECTION ( 'NONE',  ( 0.9998004120163608288, 0.000000000000000000, 0.01997839162482749342 ) ) ;
#15470 = EDGE_CURVE ( 'NONE', #39412, #34293, #26762, .T. ) ;
#15471 = CARTESIAN_POINT ( 'NONE',  ( -16.60960244842765832, 1.599067919197793490E-15, 0.000000000000000000 ) ) ;
#15472 = VECTOR ( 'NONE', #34802, 1000.000000000000227 ) ;
#15473 = CARTESIAN_POINT ( 'NONE',  ( -2.656358736808195342, 121.0686911241271702, 0.2846299364715212388 ) ) ;
#15474 = EDGE_CURVE ( 'NONE', #4252, #2129, #21999, .T. ) ;
#15475 = CARTESIAN_POINT ( 'NONE',  ( 8.404578209848946102, -5.696077331678487177, -0.5057995593162113446 ) ) ;
#15476 = CARTESIAN_POINT ( 'NONE',  ( 7.089475284343898842, 121.8675249661327626, 0.6210822171188468133 ) ) ;
#15477 = CARTESIAN_POINT ( 'NONE',  ( -45.76673701974917208, 25.51931200435043934, -1.524000000000008237 ) ) ;
#15478 = CARTESIAN_POINT ( 'NONE',  ( 22.97084167624219475, 148.6798292920915117, -0.5140709287734970268 ) ) ;
#15479 = CARTESIAN_POINT ( 'NONE',  ( 5.332935397695205637, 105.1224662015457199, 0.1065647409268305201 ) ) ;
#15480 = CARTESIAN_POINT ( 'NONE',  ( -58.27229612817279047, -0.08447917103104905789, 0.4063237998337170254 ) ) ;
#15481 = CARTESIAN_POINT ( 'NONE',  ( -9.960492004070044203, 64.81807050032566053, 1.270000000000003126 ) ) ;
#15482 = UNCERTAINTY_MEASURE_WITH_UNIT (LENGTH_MEASURE( 1.000000000000000082E-05 ), #14434, 'distance_accuracy_value', 'NONE');
#15483 = LINE ( 'NONE', #16477, #14370 ) ;
#15484 = DIRECTION ( 'NONE',  ( -5.206863593109713661E-17, 1.000000000000000000, -1.077750396879097183E-30 ) ) ;
#15485 = ORIENTED_EDGE ( 'NONE', *, *, #40949, .T. ) ;
#15486 = CARTESIAN_POINT ( 'NONE',  ( -55.11216289415786207, 6.786895728730008237, 3.177266426849158609 ) ) ;
#15487 = CARTESIAN_POINT ( 'NONE',  ( -6.576985208878872946, 120.6005770300147049, -1.107357257247939764 ) ) ;
#15488 = CARTESIAN_POINT ( 'NONE',  ( -6.442348895218290093E-14, 63.84746620154572838, 4.408874939877717575E-29 ) ) ;
#15489 = CARTESIAN_POINT ( 'NONE',  ( -5.204851039068017826, 121.0999079655412203, -0.5006067476712319220 ) ) ;
#15490 = DIRECTION ( 'NONE',  ( 0.7548010569845451379, 0.6559537821943047797, 0.000000000000000000 ) ) ;
#15491 = CARTESIAN_POINT ( 'NONE',  ( 23.34271727006406394, 149.0672090665632936, 0.4921983935722531456 ) ) ;
#15492 = EDGE_LOOP ( 'NONE', ( #8335, #17738 ) ) ;
#15493 = CARTESIAN_POINT ( 'NONE',  ( 2.739727753987758252, 28.35525327666260864, -3.728201022356329553 ) ) ;
#15494 = CARTESIAN_POINT ( 'NONE',  ( -28.94717034999018068, 63.96727089256646082, 1.523999999999993582 ) ) ;
#15495 = DIRECTION ( 'NONE',  ( -0.8745520943968250194, 0.4849315768086535083, -5.424246918827963022E-16 ) ) ;
#15496 = CARTESIAN_POINT ( 'NONE',  ( -42.60041433329244853, 22.17261999083466506, 1.881317670890278126 ) ) ;
#15497 = DIRECTION ( 'NONE',  ( 1.000000000000000000, -1.365923996832131856E-16, 0.000000000000000000 ) ) ;
#15498 = CARTESIAN_POINT ( 'NONE',  ( -7.795039456000409039, 122.5917715370820815, -0.009836026403675746793 ) ) ;
#15499 = CARTESIAN_POINT ( 'NONE',  ( -4.095482865093060809, 71.62450171983788039, -1.269999999999994023 ) ) ;
#15500 = CARTESIAN_POINT ( 'NONE',  ( 8.098994982418634692, 117.9016134627522945, 0.8176261169560979924 ) ) ;
#15501 = FACE_OUTER_BOUND ( 'NONE', #27340, .T. ) ;
#15503 = CARTESIAN_POINT ( 'NONE',  ( 21.28061085028114618, 148.8133262010608462, -1.460188425234497878 ) ) ;
#15502 = CARTESIAN_POINT ( 'NONE',  ( 4.002739386954954348, 110.9560952025013023, 3.257662289751307672 ) ) ;
#15504 = CARTESIAN_POINT ( 'NONE',  ( -5.091199858996015237, 119.8577235299091228, 0.8121313320900891419 ) ) ;
#15505 = CARTESIAN_POINT ( 'NONE',  ( -0.001188813386588473625, -13.89074316258246000, -0.9734844304884215926 ) ) ;
#15506 = CARTESIAN_POINT ( 'NONE',  ( -13.07250590169516613, 156.9444350391594014, -1.084824903291609521 ) ) ;
#15507 = CARTESIAN_POINT ( 'NONE',  ( -0.3451692354163579113, -3.745485276186693469, -0.9107729336563508138 ) ) ;
#15508 = ORIENTED_EDGE ( 'NONE', *, *, #29812, .T. ) ;
#15509 = CARTESIAN_POINT ( 'NONE',  ( -57.25386126824266597, 1.903786294961781866, 0.7664973485411351595 ) ) ;
#15510 = CARTESIAN_POINT ( 'NONE',  ( -1.566048506583701316, 120.7946061759640486, 0.1772761409975700808 ) ) ;
#15511 = CARTESIAN_POINT ( 'NONE',  ( 3.942998349758990440, -14.41637075870405482, 4.944918514907367779 ) ) ;
#15512 = CARTESIAN_POINT ( 'NONE',  ( 11.50974670170843162, 153.2879862121713757, -1.252373795633383580 ) ) ;
#15513 = ORIENTED_EDGE ( 'NONE', *, *, #21522, .F. ) ;
#15514 = CARTESIAN_POINT ( 'NONE',  ( 0.8281752705314345819, 115.7028553439171930, 1.753372524936649413 ) ) ;
#15515 = AXIS2_PLACEMENT_3D ( 'NONE', #7630, #13798, #17406 ) ;
#15516 = CARTESIAN_POINT ( 'NONE',  ( -4.734773379377719138, 117.6653775457820501, -1.128990523777680277 ) ) ;
#15517 = CARTESIAN_POINT ( 'NONE',  ( 15.76486438913719468, 145.9085485750152316, 0.2635089261703657537 ) ) ;
#15518 = EDGE_LOOP ( 'NONE', ( #24301, #19186, #20768, #24676, #21892, #39585, #3906, #21283, #22534, #5466, #29652, #25812 ) ) ;
#15519 = CARTESIAN_POINT ( 'NONE',  ( 2.522816026436708992, 158.1729697732556588, 1.709197703933636348 ) ) ;
#15520 = DIRECTION ( 'NONE',  ( -4.017660918040594346E-17, 1.000000000000000000, 2.376309959284834438E-19 ) ) ;
#15521 = FACE_BOUND ( 'NONE', #2475, .T. ) ;
#15522 = EDGE_CURVE ( 'NONE', #16450, #10948, #28794, .T. ) ;
#15523 = CARTESIAN_POINT ( 'NONE',  ( 4.900892916173488878, 117.4105777512120596, -0.9669312268769758578 ) ) ;
#15524 = CARTESIAN_POINT ( 'NONE',  ( 23.14523085694525051, 149.5941399179437781, 0.009123583346248015716 ) ) ;
#15525 = FACE_OUTER_BOUND ( 'NONE', #21738, .T. ) ;
#15526 = CARTESIAN_POINT ( 'NONE',  ( -11.25890006629609097, 56.90956307411621395, 5.016499999999999737 ) ) ;
#15527 = DIRECTION ( 'NONE',  ( 1.000000000000000000, -9.627370216492862708E-17, 0.000000000000000000 ) ) ;
#15528 = CARTESIAN_POINT ( 'NONE',  ( 1.797270874020278297, -15.24711907797275678, 5.420427335509073963 ) ) ;
#15529 = CARTESIAN_POINT ( 'NONE',  ( -46.07906060731711761, 24.80782705053048076, 1.769089518195985367 ) ) ;
#15530 = CARTESIAN_POINT ( 'NONE',  ( -7.213960532363670630, 78.77618639008812806, 1.904999999999999583 ) ) ;
#15531 = CARTESIAN_POINT ( 'NONE',  ( -4.558937555069585201, 118.0891754523873942, 0.5799898687118973939 ) ) ;
#15532 = EDGE_LOOP ( 'NONE', ( #7622, #493, #5343, #31007, #9589, #33068 ) ) ;
#15533 = ORIENTED_EDGE ( 'NONE', *, *, #36996, .T. ) ;
#15534 = CARTESIAN_POINT ( 'NONE',  ( 5.250303803498147737, 115.7029491485453150, -0.9234757868886493970 ) ) ;
#15535 = AXIS2_PLACEMENT_3D ( 'NONE', #25849, #18828, #12657 ) ;
#15536 = CARTESIAN_POINT ( 'NONE',  ( 8.440428959602655823, 119.5498230060619278, -1.071212130833359977 ) ) ;
#15537 = CARTESIAN_POINT ( 'NONE',  ( -1.237704251691503332, 106.3840144300045409, -5.116357776886615305 ) ) ;
#15538 = CARTESIAN_POINT ( 'NONE',  ( 4.733981652075166302, 117.7614939300864023, 1.072079134280608192 ) ) ;
#15539 = AXIS2_PLACEMENT_3D ( 'NONE', #8856, #15649, #40610 ) ;
#15540 = CYLINDRICAL_SURFACE ( 'NONE', #15461, 5.334000000000001407 ) ;
#15541 = CARTESIAN_POINT ( 'NONE',  ( -0.3780739950605601085, 121.2597428844643161, 0.4280417039577733007 ) ) ;
#15542 = CARTESIAN_POINT ( 'NONE',  ( 4.114294302962228755, -10.72644468530807416, -2.136776772127288559 ) ) ;
#15543 = CARTESIAN_POINT ( 'NONE',  ( -55.34794038087419210, 7.786537553440359360, 3.264576684945853291 ) ) ;
#15544 = CARTESIAN_POINT ( 'NONE',  ( 6.932344361571690428, 124.3275308867733600, 0.1272746869527294211 ) ) ;
#15545 = CARTESIAN_POINT ( 'NONE',  ( -17.47633463031934298, 147.2926247242496345, -2.162249527696345375 ) ) ;
#15546 = DIRECTION ( 'NONE',  ( -0.9998004120163608288, 0.000000000000000000, -0.01997839162482750383 ) ) ;
#15547 = CARTESIAN_POINT ( 'NONE',  ( -5.892701309309134494, 29.15168417748227014, 1.983235083422884015 ) ) ;
#15548 = FACE_OUTER_BOUND ( 'NONE', #33909, .T. ) ;
#15549 = CARTESIAN_POINT ( 'NONE',  ( -3.998286381996895233, 3.741657206818807424, 2.332027183294827832 ) ) ;
#15551 = ORIENTED_EDGE ( 'NONE', *, *, #4596, .F. ) ;
#15550 = CARTESIAN_POINT ( 'NONE',  ( 15.11126220171598256, 120.7387302883610118, 0.8143899245520164198 ) ) ;
#15552 = CARTESIAN_POINT ( 'NONE',  ( 2.873716936905370556, 105.1244232856616350, -4.504777322494160963 ) ) ;
#15553 = CARTESIAN_POINT ( 'NONE',  ( 3.662106647173574370, -15.69883703644059381, 4.006612474821164227 ) ) ;
#15554 = CARTESIAN_POINT ( 'NONE',  ( -9.920314382279082466, 120.7895603300898699, 1.200622369358214980 ) ) ;
#15555 = CARTESIAN_POINT ( 'NONE',  ( 0.1924800537393606958, 19.99376482044840486, 0.9543378882872525226 ) ) ;
#15556 = CARTESIAN_POINT ( 'NONE',  ( 0.9479787518424646064, 8.937585264489511516, -0.2400550011337005962 ) ) ;
#15557 = EDGE_LOOP ( 'NONE', ( #39856, #8552, #3426, #3652, #11469, #1892 ) ) ;
#15558 = ORIENTED_EDGE ( 'NONE', *, *, #41743, .T. ) ;
#15559 = CARTESIAN_POINT ( 'NONE',  ( -14.73199999999999577, 61.59499999999999886, 1.904999999999990479 ) ) ;
#15560 = CARTESIAN_POINT ( 'NONE',  ( -0.1065646865916381331, 105.8844662015456777, 5.332932678536312032 ) ) ;
#15561 = CARTESIAN_POINT ( 'NONE',  ( -7.796255004792742582, 122.1031240515655298, 0.5053261734565678287 ) ) ;
#15562 = CARTESIAN_POINT ( 'NONE',  ( -14.16569067496504353, 138.8670163227227476, -0.2830642121559618363 ) ) ;
#15563 = CARTESIAN_POINT ( 'NONE',  ( 2.715028358135622266, -14.64271907847003362, 5.065740987199049528 ) ) ;
#15564 = CARTESIAN_POINT ( 'NONE',  ( 4.309327875668891750, 119.9149831030956932, -0.7077533764146594075 ) ) ;
#15565 = CARTESIAN_POINT ( 'NONE',  ( -18.46656456646938693, 135.7714211226372640, -2.417028963773544259 ) ) ;
#15566 = CARTESIAN_POINT ( 'NONE',  ( -5.369399562154598904, 64.90898011766716991, -1.523999999999993582 ) ) ;
#15567 = CARTESIAN_POINT ( 'NONE',  ( 7.974932797479802993, 121.6047494564416951, 1.136202016109667978 ) ) ;
#15568 = CARTESIAN_POINT ( 'NONE',  ( -0.2616981356411257065, 38.12352966651759090, 1.602708108658221109 ) ) ;
#15569 = CARTESIAN_POINT ( 'NONE',  ( 15.83367336760669097, 146.2622375132148989, -0.01472612784998089501 ) ) ;
#15570 = ORIENTED_EDGE ( 'NONE', *, *, #16742, .F. ) ;
#15571 = CARTESIAN_POINT ( 'NONE',  ( 5.010184479710102501, 117.3993854065330851, 0.7504461923096029663 ) ) ;
#15572 = DIRECTION ( 'NONE',  ( -0.3256999990547897461, -0.9454731675810318370, 0.000000000000000000 ) ) ;
#15573 = AXIS2_PLACEMENT_3D ( 'NONE', #24713, #24929, #18524 ) ;
#15574 = DIRECTION ( 'NONE',  ( -5.188838149069471174E-16, 1.699382548006136313E-16, 1.000000000000000000 ) ) ;
#15575 = CARTESIAN_POINT ( 'NONE',  ( -58.67120857663415734, -0.3138064510425503384, 0.3172299661764326761 ) ) ;
#15576 = CARTESIAN_POINT ( 'NONE',  ( -7.510622214715407807, 18.91685342841953954, 3.806420843228597306 ) ) ;
#15577 = CARTESIAN_POINT ( 'NONE',  ( 10.10772093100550961, 154.1059161911440469, 1.650231108813019265 ) ) ;
#15578 = FACE_OUTER_BOUND ( 'NONE', #1121, .T. ) ;
#15579 = CARTESIAN_POINT ( 'NONE',  ( 23.44551923343641064, 146.8400249081559537, 0.3912800906488115293 ) ) ;
#15580 = CARTESIAN_POINT ( 'NONE',  ( -3.568456891169586420, 108.6786390861269922, 3.983803253449686110 ) ) ;
#15581 = LINE ( 'NONE', #3036, #24379 ) ;
#15582 = CARTESIAN_POINT ( 'NONE',  ( 2.884051542275651414, 156.0957788938021054, 0.05763021347587640730 ) ) ;
#15583 = CARTESIAN_POINT ( 'NONE',  ( 5.670988759832523485, -4.508684804710943794, -6.293633234193930726 ) ) ;
#15584 = CARTESIAN_POINT ( 'NONE',  ( -5.512364842945291166, 116.9397240910284239, -0.6180008233057252554 ) ) ;
#15585 = CARTESIAN_POINT ( 'NONE',  ( 0.07157677170298341884, 110.3683645023726569, -3.581994345755902032 ) ) ;
#15586 = DIRECTION ( 'NONE',  ( -0.9816537812491090698, -0.1906721105965065721, -4.769617732184476148E-16 ) ) ;
#15587 = DIRECTION ( 'NONE',  ( 0.01731298258488512057, -0.9998501190848634312, 6.551018405069406341E-15 ) ) ;
#15588 = CARTESIAN_POINT ( 'NONE',  ( -1.796629210684171918, -4.683219827815034542, 8.244768259809569955 ) ) ;
#15589 = CARTESIAN_POINT ( 'NONE',  ( 1.067977723796545320, 118.1588881525931640, 0.8905038927680214433 ) ) ;
#15590 = FACE_OUTER_BOUND ( 'NONE', #18223, .T. ) ;
#15591 = CARTESIAN_POINT ( 'NONE',  ( 1.831848720338793202, -15.17974794010013007, 5.463771816453670382 ) ) ;
#15592 = CARTESIAN_POINT ( 'NONE',  ( 0.1289837059587395918, 106.1822392402443143, -5.211597877332949658 ) ) ;
#15593 = CARTESIAN_POINT ( 'NONE',  ( -2.863213894092427658, 116.8186761214209213, 0.2817159656421849290 ) ) ;
#15594 = ORIENTED_EDGE ( 'NONE', *, *, #14403, .T. ) ;
#15595 = CARTESIAN_POINT ( 'NONE',  ( 6.059261036834406866, 65.30181249999998272, 5.016499999999999737 ) ) ;
#15596 = AXIS2_PLACEMENT_3D ( 'NONE', #18896, #31905, #1896 ) ;
#15597 = VERTEX_POINT ( 'NONE', #9773 ) ;
#15598 = FACE_OUTER_BOUND ( 'NONE', #26156, .T. ) ;
#15599 = CARTESIAN_POINT ( 'NONE',  ( -5.953081049894649368, 155.3987518795295273, -0.06674817819388183249 ) ) ;
#15600 = CARTESIAN_POINT ( 'NONE',  ( 3.006733222167471631, -15.59844357659602387, 5.538909454127313836 ) ) ;
#15601 = CARTESIAN_POINT ( 'NONE',  ( -13.70042256496009614, 122.3361261571837986, 1.218568937077757264 ) ) ;
#15602 = CARTESIAN_POINT ( 'NONE',  ( 15.72870526381831269, 122.9504679175852573, -0.8738493638518137763 ) ) ;
#15603 = CARTESIAN_POINT ( 'NONE',  ( -3.158589313471108273, 4.191505055319898254, 3.400481138232230194 ) ) ;
#15604 = CARTESIAN_POINT ( 'NONE',  ( -56.22360126104668154, 4.817347650610097176, -2.667469593848362130 ) ) ;
#15605 = ORIENTED_EDGE ( 'NONE', *, *, #12059, .F. ) ;
#15606 = CARTESIAN_POINT ( 'NONE',  ( -0.008700780993364600618, 121.2597428844645293, 0.4354226598341946475 ) ) ;
#15607 = DIRECTION ( 'NONE',  ( 5.188838149069472160E-16, -1.699382548006136559E-16, -1.000000000000000000 ) ) ;
#15608 = CARTESIAN_POINT ( 'NONE',  ( -10.26617122093362333, 123.0849000269954701, 0.9769925898671679709 ) ) ;
#15609 = DIRECTION ( 'NONE',  ( -1.000000000000000000, 1.011795553208986377E-16, 0.000000000000000000 ) ) ;
#15610 = CARTESIAN_POINT ( 'NONE',  ( 11.84733475906190314, 122.5845257805695923, -1.288679497020476905 ) ) ;
#15611 = CARTESIAN_POINT ( 'NONE',  ( 0.02768730785345232051, 158.9256195073445213, -1.385586103196075447 ) ) ;
#15612 = CARTESIAN_POINT ( 'NONE',  ( -50.36516092884956208, 15.79195539882771726, -4.916963016749614113 ) ) ;
#15613 = CARTESIAN_POINT ( 'NONE',  ( 9.485477581651457157, 123.8597080710187015, -0.4105858232041851852 ) ) ;
#15614 = ORIENTED_EDGE ( 'NONE', *, *, #31641, .F. ) ;
#15615 = CARTESIAN_POINT ( 'NONE',  ( -9.561780282765809602, 155.2307989660268959, -2.006535919638082088 ) ) ;
#15616 = CARTESIAN_POINT ( 'NONE',  ( 3.866904830252686054, -15.34763638737450542, 1.784481441967298743 ) ) ;
#15617 = CARTESIAN_POINT ( 'NONE',  ( -4.107451408814531746, 118.2429491485452928, -0.3509027312660569220 ) ) ;
#15618 = EDGE_CURVE ( 'NONE', #24697, #30779, #34246, .T. ) ;
#15619 = CARTESIAN_POINT ( 'NONE',  ( -11.58677707360137532, 55.24499999999999034, -4.474811398758259173 ) ) ;
#15620 = CARTESIAN_POINT ( 'NONE',  ( -4.842027084325775554, 117.6755028110320183, 0.8981427047208370151 ) ) ;
#15621 = CARTESIAN_POINT ( 'NONE',  ( -0.009931517865308202644, 119.6374844068871397, 0.4970137656763585210 ) ) ;
#15622 = PLANE ( 'NONE',  #38953 ) ;
#15623 = AXIS2_PLACEMENT_3D ( 'NONE', #15238, #18642, #41031 ) ;
#15624 = CARTESIAN_POINT ( 'NONE',  ( -2.614655561276646889, 23.60746518810343986, 3.812863311767609620 ) ) ;
#15625 = CARTESIAN_POINT ( 'NONE',  ( 11.87576104716899117, 151.9737369308441544, 0.5463127210923327537 ) ) ;
#15626 = LINE ( 'NONE', #38650, #32401 ) ;
#15627 = B_SPLINE_CURVE_WITH_KNOTS ( 'NONE', 3,
 ( #30459, #40489, #37274, #20438, #13854, #23852, #27681 ),
 .UNSPECIFIED., .F., .F.,
 ( 4, 1, 1, 1, 4 ),
 ( 0.6462721360804385418, 0.7047636632187940231, 0.8031757754791960524, 0.9015878877395980817, 1.000000000000000000 ),
 .UNSPECIFIED. ) ;
#15629 = ORIENTED_EDGE ( 'NONE', *, *, #40979, .T. ) ;
#15628 = CARTESIAN_POINT ( 'NONE',  ( -46.43071087740785430, 19.11736041196146374, -2.831212230509051686 ) ) ;
#15630 = CARTESIAN_POINT ( 'NONE',  ( -0.5995136777521792304, 117.9394517551924082, 1.384272192882745278 ) ) ;
#15631 = CARTESIAN_POINT ( 'NONE',  ( -58.43690671596436914, -0.4125963578781866037, -1.035377653829272970E-14 ) ) ;
#15632 = CARTESIAN_POINT ( 'NONE',  ( -54.02024612309215001, 9.209302577745638985, 3.715716622219290777 ) ) ;
#15633 = CARTESIAN_POINT ( 'NONE',  ( -8.464895589923902008, 119.1960555687802525, -1.333724091418657220 ) ) ;
#15634 = CARTESIAN_POINT ( 'NONE',  ( -5.871452009091383317, 53.58606249999999704, -5.016499999999999737 ) ) ;
#15635 = CARTESIAN_POINT ( 'NONE',  ( -53.18864123405685262, 14.74122628988702743, 1.932938280191007996 ) ) ;
#15636 = CARTESIAN_POINT ( 'NONE',  ( -10.81400209053381545, 157.9177219752764358, -0.09677702710655955443 ) ) ;
#15637 = VERTEX_POINT ( 'NONE', #32561 ) ;
#15638 = CARTESIAN_POINT ( 'NONE',  ( -47.16890147375944764, 22.20336809214633433, -4.187060126831887885 ) ) ;
#15639 = CARTESIAN_POINT ( 'NONE',  ( -6.939462325801320830, 121.9280307701022679, -0.3189346169104567141 ) ) ;
#15640 = FACE_OUTER_BOUND ( 'NONE', #27071, .T. ) ;
#15641 = ORIENTED_EDGE ( 'NONE', *, *, #38437, .T. ) ;
#15642 = CARTESIAN_POINT ( 'NONE',  ( 2.027518441928002790, 115.7029486573731702, -1.637689744274474002 ) ) ;
#15643 = CARTESIAN_POINT ( 'NONE',  ( -8.827910802435056326, 123.6950213215744583, -0.2595790122280455803 ) ) ;
#15644 = CARTESIAN_POINT ( 'NONE',  ( 5.611934155553572445, -13.19144435144412064, 2.399925970747030846 ) ) ;
#15645 = CARTESIAN_POINT ( 'NONE',  ( -5.880040083609346269, 118.0670013439590491, 0.7714800252663618352 ) ) ;
#15646 = CARTESIAN_POINT ( 'NONE',  ( -5.071732749312718447, 117.1432901748061113, -0.6012547207297572749 ) ) ;
#15647 = CARTESIAN_POINT ( 'NONE',  ( 23.18927481933079449, 149.6199392087789306, 0.6935230913228408456 ) ) ;
#15648 = CARTESIAN_POINT ( 'NONE',  ( 0.6507712759201194075, 120.9971526617350577, 0.1121992020169609583 ) ) ;
#15649 = DIRECTION ( 'NONE',  ( 4.017660918040594346E-17, -1.000000000000000000, -2.376309959284834438E-19 ) ) ;
#15650 = CARTESIAN_POINT ( 'NONE',  ( -0.4721710868402241301, 14.98625149489145159, 0.8573358612705738180 ) ) ;
#15651 = EDGE_CURVE ( 'NONE', #14687, #4530, #4055, .T. ) ;
#15652 = CARTESIAN_POINT ( 'NONE',  ( 0.0008202526017135117458, 159.6052337359418800, -0.04104879434819952433 ) ) ;
#15653 = CARTESIAN_POINT ( 'NONE',  ( -17.64290547347870941, 83.78857423953914463, 1.269999999999996909 ) ) ;
#15654 = DIRECTION ( 'NONE',  ( 0.000000000000000000, 0.000000000000000000, 1.000000000000000000 ) ) ;
#15655 = ORIENTED_EDGE ( 'NONE', *, *, #17045, .T. ) ;
#15656 = CARTESIAN_POINT ( 'NONE',  ( 8.658023306739559999, 118.2891936209626778, 0.9762238836702761269 ) ) ;
#15657 = CARTESIAN_POINT ( 'NONE',  ( -15.24000000000000554, 71.11999999999999034, -5.714999999999999858 ) ) ;
#15658 = CARTESIAN_POINT ( 'NONE',  ( 0.3865025759030094044, 117.6538564835029206, 0.5089310662413600861 ) ) ;
#15659 = CARTESIAN_POINT ( 'NONE',  ( 20.17730036299072793, 147.7236477000422497, -1.702857440531004185 ) ) ;
#15660 = CARTESIAN_POINT ( 'NONE',  ( -5.002256584969458686, 16.77047026005132224, -6.819937116506380903 ) ) ;
#15661 = CARTESIAN_POINT ( 'NONE',  ( -3.924194517545539274, 117.4679918459733585, -0.7389123598820264149 ) ) ;
#15662 = CARTESIAN_POINT ( 'NONE',  ( 4.726004515057145028, 117.8966366527547933, -0.7851610368387000882 ) ) ;
#15663 = DIRECTION ( 'NONE',  ( -0.7770581983690701966, 0.6294287539884197979, -8.537024980200731099E-16 ) ) ;
#15664 = CARTESIAN_POINT ( 'NONE',  ( -9.119960873764156872, 153.9201329141909866, -0.06997149051007733878 ) ) ;
#15665 = CARTESIAN_POINT ( 'NONE',  ( -18.87709319873820135, 147.8663216482595146, -2.479723349601893112 ) ) ;
#15666 = CARTESIAN_POINT ( 'NONE',  ( 5.927515451590630313, -14.79481669900410701, -0.3156388015035426764 ) ) ;
#15667 = CARTESIAN_POINT ( 'NONE',  ( 4.726250468511487668, 118.5931160184169073, 1.020578222860014872 ) ) ;
#15668 = ADVANCED_FACE ( 'NONE', ( #32355, #3183 ), #207, .T. ) ;
#15669 = B_SPLINE_CURVE_WITH_KNOTS ( 'NONE', 3,
 ( #12128, #31293, #28316, #28529, #37906, #38332, #2137, #5759, #14890, #18293, #41534, #15099 ),
 .UNSPECIFIED., .F., .F.,
 ( 4, 1, 1, 1, 1, 1, 1, 1, 1, 4 ),
 ( 0.5426758968252777260, 0.5876249999999998419, 0.6700999999999999179, 0.7525749999999999940, 0.7938125000000000320, 0.8350499999999998479, 0.8762874999999994419, 0.9175249999999994799, 0.9587624999999999620, 0.9957666935384934526 ),
 .UNSPECIFIED. ) ;
#15670 = PLANE ( 'NONE',  #21290 ) ;
#15671 = VERTEX_POINT ( 'NONE', #40030 ) ;
#15672 = B_SPLINE_SURFACE_WITH_KNOTS ( 'NONE', 3, 3, ( 
 ( #41212, #31401, #31183, #2453, #17765, #5227, #11803, #12013, #21790, #1614, #38008, #37375, #8192, #27576, #2025, #5653 ),
 ( #18608, #8830, #34818, #5018, #14990, #17979, #31614, #11382, #11591, #37789, #21161, #8616, #34394, #27991, #15414, #37580 ),
 ( #5434, #8407, #28418, #21367, #18390, #41424, #34194, #12231, #40584, #37171, #30976, #7995, #20963, #33984, #307, #35239 ),
 ( #9865, #13061, #25437, #18816, #6269, #26051, #22835, #39062, #12445, #25637, #35444, #38438, #3501, #12650, #29040, #42059 ),
 ( #19026, #3285, #22007, #31824, #22418, #32454, #15620, #16460, #2661, #19240, #28624, #41638, #16246, #35661, #9253, #28838 ),
 ( #25221, #29467, #9659, #38227, #9041, #35038, #29250, #32249, #12853, #22626, #25840, #35873, #6065, #32032, #22209, #15832 ),
 ( #16038, #6684, #41851, #2870, #38645, #3079, #6472, #19651, #94, #19447, #38848, #32667, #5858, #9451, #2358, #8524 ),
 ( #14894, #34311, #37283, #1936, #37485, #18298, #28322, #31095, #21694, #14479, #21075, #34720, #24480, #30887, #11708, #2143 ),
 ( #15316, #27897, #37910, #5550, #5139, #34101, #24911, #27490, #30675, #18507, #8102, #27692, #41331, #31512, #40904, #24696 ),
 ( #4928, #11495, #21483, #11921, #5765, #40700, #8944, #12133, #25125, #1728, #24278, #37702, #38127, #21910, #34941, #17885 ),
 ( #34516, #14685, #1523, #18092, #5342, #31297, #8733, #8310, #40498, #11293, #21281, #15103, #28105, #41115, #9977, #12348 ),
 ( #19551, #32147, #18931, #22532, #22736, #38544, #31941, #41752, #28535, #15943, #16145, #35767, #26168, #2980, #28939, #2777 ),
 ( #41541, #15733, #25338, #19347, #16361, #13181, #19143, #38752, #31728, #9561, #41956, #3395, #35978, #5969, #29147, #25954 ),
 ( #12757, #12960, #32560, #35561, #32354, #25743, #22320, #38341, #6377, #25542, #3182, #29367, #14851, #9772, #2572, #9158 ),
 ( #12553, #28738, #38961, #6584, #206, #39170, #22951, #18718, #15531, #35347, #22114, #35143, #9358, #6174, #36825, #26380 ),
 ( #4461, #7644, #7228, #20187, #13603, #14013, #14218, #17418, #7016, #6794, #27020, #3829, #16793, #33213, #1263, #23159 ),
 ( #39387, #32783, #10405, #19761, #16576, #634, #17213, #24017, #27227, #39819, #4038, #4250, #1050, #23594, #40240, #39602 ),
 ( #19984, #33001, #26811, #26594, #29794, #30210, #20602, #17000, #23377, #10612, #10822, #36410, #29999, #839, #29587, #13813 ),
 ( #23805, #11035, #36616, #7435, #20393, #33420, #421, #40029, #13391, #33634, #30415, #3613, #10190, #36195, #7853, #27847 ),
 ( #21645, #40854, #28271, #2090, #41063, #30832, #15266, #11657, #34259, #24641, #21433, #14635, #4879, #8257, #34669, #2306 ),
 ( #5499, #31042, #33839, #40648, #37234, #37653, #11874, #27636, #8053, #17834, #4667, #5088, #34461, #24863, #41277, #21229 ),
 ( #18040, #17624, #8477, #1679, #12083, #11442, #24225, #30626, #1469, #5294, #18458, #37035, #18243, #15054, #14426, #28054 ),
 ( #24430, #20813, #31248, #1880, #37859, #8681, #37435, #14843, #31462, #27433, #40449, #21026, #11240, #34049, #21859, #28690 ),
 ( #12296, #36097, #32896, #35888, #9878, #19881, #39499, #3516, #39285, #22848, #41698, #31678, #39076, #31891, #13290, #23273 ) ),
 .UNSPECIFIED., .F., .F., .F.,
 ( 4, 2, 2, 2, 2, 2, 2, 2, 2, 2, 2, 4 ),
 ( 4, 2, 2, 2, 2, 1, 1, 2, 4 ),
 ( 0.000000000000000000, 0.1320156187279754312, 0.1980234280919631606, 0.2640312374559508624, 0.3918846486443451349, 0.4558113542385422989, 0.5197380598327394630, 0.5807839412718216465, 0.6418298227109038301, 0.7639215855890681972, 0.8819607927945340986, 1.000000000000000000 ),
 ( 0.000000000000000000, 0.1250000000000000000, 0.2500000000000000000, 0.3750000000000000000, 0.5000000000000000000, 0.7500000000000000000, 0.8750000000000000000, 0.9375000000000000000, 1.000000000000000000 ),
 .UNSPECIFIED. ) ;
#15673 = CARTESIAN_POINT ( 'NONE',  ( 18.29546242682543422, 149.1773161885088825, 2.457454238777247557 ) ) ;
#15674 = CARTESIAN_POINT ( 'NONE',  ( -4.792324638262678960, 56.51998046905272588, 4.972049999962470324 ) ) ;
#15675 = VECTOR ( 'NONE', #7897, 1000.000000000000114 ) ;
#15676 = DIRECTION ( 'NONE',  ( -0.8745520943968245753, 0.4849315768086539524, -5.691349986800526185E-16 ) ) ;
#15677 = CARTESIAN_POINT ( 'NONE',  ( -0.9965922269827753865, 107.7619142660649203, 4.530701086038176228 ) ) ;
#15678 = CARTESIAN_POINT ( 'NONE',  ( 6.819937116507564845, -4.819529739946951885, -5.002256584970107056 ) ) ;
#15679 = CARTESIAN_POINT ( 'NONE',  ( 16.02106284285049753, 145.8417561620165372, 1.176135107295965154 ) ) ;
#15680 = EDGE_CURVE ( 'NONE', #25646, #6455, #257, .T. ) ;
#15681 = CARTESIAN_POINT ( 'NONE',  ( 3.845766519666786287, 116.9593488885201538, -0.3368132424836104977 ) ) ;
#15682 = DIRECTION ( 'NONE',  ( -9.627370216492862708E-17, -1.000000000000000000, 0.000000000000000000 ) ) ;
#15683 = CARTESIAN_POINT ( 'NONE',  ( -57.95663924081166130, 0.5986300452915040982, 0.9156402804120569172 ) ) ;
#15684 = CARTESIAN_POINT ( 'NONE',  ( -5.936145915410568463, 56.51499999999997925, 4.381499802576774627 ) ) ;
#15685 = CARTESIAN_POINT ( 'NONE',  ( -6.894732321505390615, 117.1676844715483270, -0.1377731603346601386 ) ) ;
#15686 = ORIENTED_EDGE ( 'NONE', *, *, #11633, .F. ) ;
#15687 = CARTESIAN_POINT ( 'NONE',  ( 6.362922045609294308, 119.9956554345082935, -0.9575366525960410380 ) ) ;
#15688 = CARTESIAN_POINT ( 'NONE',  ( -5.332935397695336199, 116.0444662015457311, -0.1065647409268299234 ) ) ;
#15689 = CARTESIAN_POINT ( 'NONE',  ( -14.53200193279647223, 139.1552669279217298, -1.026914593849030943 ) ) ;
#15690 = CARTESIAN_POINT ( 'NONE',  ( -5.064403469544192404, 117.2685460503076627, 0.4793543776217523145 ) ) ;
#15691 = CIRCLE ( 'NONE', #6870, 0.3810000000000015041 ) ;
#15692 = CARTESIAN_POINT ( 'NONE',  ( 23.36005780523110431, 148.8745345081378559, 0.4925575130201677032 ) ) ;
#15693 = VERTEX_POINT ( 'NONE', #37036 ) ;
#15694 = CARTESIAN_POINT ( 'NONE',  ( 0.1710433496020407063, 14.98650505531991506, 4.637963194678765610 ) ) ;
#15695 = ADVANCED_FACE ( 'NONE', ( #1264 ), #7063, .T. ) ;
#15696 = DIRECTION ( 'NONE',  ( -0.8745520943968250194, 0.4849315768086532863, -5.361993529360574930E-16 ) ) ;
#15697 = CARTESIAN_POINT ( 'NONE',  ( 7.213960532363571154, 78.77618639008812806, -1.904999999999999583 ) ) ;
#15698 = CARTESIAN_POINT ( 'NONE',  ( -42.32312746590549324, 22.34068395104253213, 1.752427511502289370 ) ) ;
#15699 = DIRECTION ( 'NONE',  ( -9.627370216492862708E-17, -1.000000000000000000, 0.000000000000000000 ) ) ;
#15700 = CARTESIAN_POINT ( 'NONE',  ( 6.103784187571975828, 121.1829703657862751, 0.6769658165800259697 ) ) ;
#15701 = EDGE_CURVE ( 'NONE', #11376, #28135, #17625, .T. ) ;
#15702 = CARTESIAN_POINT ( 'NONE',  ( 1.305078825605721526, 159.4185946040361728, 0.8784184817623138519 ) ) ;
#15703 = CARTESIAN_POINT ( 'NONE',  ( 3.350153020191438014, 104.6144662015457385, -3.487106363639548512 ) ) ;
#15705 = CARTESIAN_POINT ( 'NONE',  ( 11.79681931163863595, 156.4111399680655552, -1.533406117021610227 ) ) ;
#15704 = CARTESIAN_POINT ( 'NONE',  ( 5.224085778414913506, 56.51499999999996504, 4.542437760755090537 ) ) ;
#15706 = VECTOR ( 'NONE', #19188, 1000.000000000000000 ) ;
#15707 = CARTESIAN_POINT ( 'NONE',  ( -0.03066982525788228969, 157.3074135339440147, 1.534843470138540722 ) ) ;
#15708 = CARTESIAN_POINT ( 'NONE',  ( 3.750385610654966229, 4.675867361267946443, -2.714424430587211834 ) ) ;
#15709 = CARTESIAN_POINT ( 'NONE',  ( -14.81745968805125102, 156.1223461918646933, -1.150419650929870530 ) ) ;
#15710 = ADVANCED_FACE ( 'NONE', ( #30627 ), #31020, .T. ) ;
#15711 = EDGE_LOOP ( 'NONE', ( #4416, #37911, #3185, #12781, #40616, #18643 ) ) ;
#15712 = CARTESIAN_POINT ( 'NONE',  ( -56.89020484191215132, 2.444072280526621288, 0.3054065742134224881 ) ) ;
#15713 = CARTESIAN_POINT ( 'NONE',  ( -13.24427968334914851, 134.0707761029912035, 0.3110103029741254077 ) ) ;
#15714 = CARTESIAN_POINT ( 'NONE',  ( 5.179289707447474633, -13.00434337860746581, 2.646125397160491222 ) ) ;
#15715 = CARTESIAN_POINT ( 'NONE',  ( -0.03519895178523997636, 115.7029491485446613, 1.761499482104069703 ) ) ;
#15716 = CARTESIAN_POINT ( 'NONE',  ( -4.558806136799320008, 118.0156478519566576, -0.8816215797218194261 ) ) ;
#15717 = CARTESIAN_POINT ( 'NONE',  ( 12.85860202769631755, 133.7716054015561156, 0.2569454702854387373 ) ) ;
#15718 = ORIENTED_EDGE ( 'NONE', *, *, #25394, .F. ) ;
#15719 = CARTESIAN_POINT ( 'NONE',  ( 8.740007204533831953, 120.0394951565550343, 1.484413609726634942 ) ) ;
#15720 = CYLINDRICAL_SURFACE ( 'NONE', #11346, 0.2540000000000012248 ) ;
#15721 = DIRECTION ( 'NONE',  ( 1.000000000000000000, 0.000000000000000000, -6.146657985744586818E-16 ) ) ;
#15722 = VECTOR ( 'NONE', #37312, 1000.000000000000000 ) ;
#15723 = CARTESIAN_POINT ( 'NONE',  ( -22.08264656579488161, 150.6352520364973486, 0.6282006774575533692 ) ) ;
#15724 = CARTESIAN_POINT ( 'NONE',  ( 4.851964763131728198, 117.4768176267210009, -0.9923522720269655206 ) ) ;
#15725 = CARTESIAN_POINT ( 'NONE',  ( 0.9295402922911353283, 116.5712332538976455, -0.1496640007645968773 ) ) ;
#15726 = CARTESIAN_POINT ( 'NONE',  ( -19.33375693323417011, 80.42273151551299293, -1.524000000000003574 ) ) ;
#15727 = TOROIDAL_SURFACE ( 'NONE', #39576, 3.683000000000000718, 0.5080000000000000071 ) ;
#15728 = CARTESIAN_POINT ( 'NONE',  ( 5.295064810963916457, 115.6909491485453145, 0.7219800058539025400 ) ) ;
#15729 = CARTESIAN_POINT ( 'NONE',  ( -46.60530155212508419, 26.17382724835469432, 1.171222222222213505 ) ) ;
#15730 = CARTESIAN_POINT ( 'NONE',  ( -4.812635773683934026, 117.4067914754907065, -1.196957445793439989 ) ) ;
#15731 = CARTESIAN_POINT ( 'NONE',  ( -45.76673701974917208, 25.51931200435043934, 1.523999999999991806 ) ) ;
#15732 = DIRECTION ( 'NONE',  ( -0.9849462604886047856, 0.000000000000000000, 0.1728608224830407714 ) ) ;
#15733 = CARTESIAN_POINT ( 'NONE',  ( -4.572877053309778006, 118.0343149336223831, 0.6783132061656282907 ) ) ;
#15734 = ADVANCED_FACE ( 'NONE', ( #24643 ), #38349, .T. ) ;
#15735 = ORIENTED_EDGE ( 'NONE', *, *, #32280, .T. ) ;
#15736 = VERTEX_POINT ( 'NONE', #31043 ) ;
#15737 = CARTESIAN_POINT ( 'NONE',  ( -1.967456252267424155, 118.7629491485468236, -1.232493637335213332 ) ) ;
#15738 = CARTESIAN_POINT ( 'NONE',  ( -6.004173374711351485, 119.3322421624460077, -1.266279038469856122 ) ) ;
#15739 = CARTESIAN_POINT ( 'NONE',  ( -2.208446607403949713, 108.4767889311100362, -4.246804138318780453 ) ) ;
#15740 = CARTESIAN_POINT ( 'NONE',  ( 4.636258067987869325, 118.0184330405641333, 0.8097526809780418722 ) ) ;
#15741 = CIRCLE ( 'NONE', #12356, 0.5080000000000000071 ) ;
#15742 = FACE_OUTER_BOUND ( 'NONE', #28509, .T. ) ;
#15743 = CARTESIAN_POINT ( 'NONE',  ( -12.84263471596180928, 130.8243885708800747, -1.276791159582618018 ) ) ;
#15744 = CARTESIAN_POINT ( 'NONE',  ( 1.360477052538118681, -3.804838552850991817, 4.419457122809256511 ) ) ;
#15745 = CARTESIAN_POINT ( 'NONE',  ( -15.37877921309977047, 79.99470228764801050, 1.269999999999996909 ) ) ;
#15746 = DIRECTION ( 'NONE',  ( -0.8745520943968225769, 0.4849315768086578382, -5.691349986800571545E-16 ) ) ;
#15747 = CARTESIAN_POINT ( 'NONE',  ( 5.317809737553744753, 116.7000894413872629, -0.8094161617621952187 ) ) ;
#15748 = CARTESIAN_POINT ( 'NONE',  ( -10.41670863957363302, 122.9580799906392343, -1.467069541016856826 ) ) ;
#15749 = CARTESIAN_POINT ( 'NONE',  ( 21.68875320759051917, 132.7412702629105468, 0.4333929054516009183 ) ) ;
#15750 = CARTESIAN_POINT ( 'NONE',  ( -5.307248809044878612, 31.23445644987117120, 3.607707940702756133 ) ) ;
#15751 = DIRECTION ( 'NONE',  ( 5.188838149069472160E-16, -1.699382548006136559E-16, -1.000000000000000000 ) ) ;
#15752 = CARTESIAN_POINT ( 'NONE',  ( -4.012847786888796620, 11.73797844546971270, -2.294585225469591983 ) ) ;
#15754 = ORIENTED_EDGE ( 'NONE', *, *, #31878, .T. ) ;
#15753 = CARTESIAN_POINT ( 'NONE',  ( 7.852582050918188727, 158.6543443936584481, 0.7853876145049530910 ) ) ;
#15755 = CARTESIAN_POINT ( 'NONE',  ( -1.944567074771800241, 104.6144662015455111, -4.425999150025703877 ) ) ;
#15756 = CARTESIAN_POINT ( 'NONE',  ( 3.885490704569380060, -15.31119228946847777, 1.341400144935093630 ) ) ;
#15757 = CARTESIAN_POINT ( 'NONE',  ( -5.880668475635614456, 119.2401804501882197, 0.9647153462086465181 ) ) ;
#15758 = VECTOR ( 'NONE', #6376, 999.9999999999998863 ) ;
#15759 = CARTESIAN_POINT ( 'NONE',  ( -0.8274880129334906131, 26.04165684986237039, -0.5117960016238547460 ) ) ;
#15760 = AXIS2_PLACEMENT_3D ( 'NONE', #34159, #30946, #27122 ) ;
#15761 = EDGE_CURVE ( 'NONE', #24980, #17144, #28484, .T. ) ;
#15762 = CARTESIAN_POINT ( 'NONE',  ( 0.8097498057273965211, -0.1318080948593848278, -0.5455758836208917106 ) ) ;
#15763 = ORIENTED_EDGE ( 'NONE', *, *, #24064, .F. ) ;
#15764 = EDGE_CURVE ( 'NONE', #13560, #24559, #31249, .T. ) ;
#15765 = EDGE_LOOP ( 'NONE', ( #41984, #3784, #17398, #16364 ) ) ;
#15766 = FACE_OUTER_BOUND ( 'NONE', #36102, .T. ) ;
#15767 = CARTESIAN_POINT ( 'NONE',  ( 6.475519728870414049, 122.5560431351108974, 0.2403424393823896110 ) ) ;
#15768 = CARTESIAN_POINT ( 'NONE',  ( -15.20409169301252739, 148.9716719698033387, 0.7946991634813627137 ) ) ;
#15769 = FACE_OUTER_BOUND ( 'NONE', #1730, .T. ) ;
#15770 = CARTESIAN_POINT ( 'NONE',  ( 2.584330390446285985, -14.72226154538576459, 5.166463236119047231 ) ) ;
#15771 = CARTESIAN_POINT ( 'NONE',  ( 3.787250209144782165, 156.8112981010400802, -1.501541828261893086 ) ) ;
#15772 = CARTESIAN_POINT ( 'NONE',  ( -4.978738709155277498, 118.8869175073591578, -1.099525347370199135 ) ) ;
#15773 = CARTESIAN_POINT ( 'NONE',  ( -48.28978369826177186, 19.63653578263564015, -5.206999999995405304 ) ) ;
#15774 = CARTESIAN_POINT ( 'NONE',  ( 7.976738704924626333, 121.5955735554254602, 1.139979217470462158 ) ) ;
#15775 = FACE_OUTER_BOUND ( 'NONE', #11037, .T. ) ;
#15776 = CARTESIAN_POINT ( 'NONE',  ( 15.42372963437252587, 147.8340308814284754, -0.02010286832636620433 ) ) ;
#15777 = ORIENTED_EDGE ( 'NONE', *, *, #30869, .T. ) ;
#15778 = CARTESIAN_POINT ( 'NONE',  ( -8.584014518950164430, 73.13423810798757074, -1.523999999999996691 ) ) ;
#15779 = CARTESIAN_POINT ( 'NONE',  ( 0.1066493941974573784, 105.7853621660184444, -5.332931186019219005 ) ) ;
#15780 = CARTESIAN_POINT ( 'NONE',  ( 4.898459268277319367, 117.7581306180235288, -0.6108534173935511458 ) ) ;
#15781 = CARTESIAN_POINT ( 'NONE',  ( -2.798479926918381544, 16.31753791307728818, -7.953355231451358698 ) ) ;
#15782 = CARTESIAN_POINT ( 'NONE',  ( 6.488156926834022897, 121.4051597255373025, 0.7118474008431251443 ) ) ;
#15783 = CARTESIAN_POINT ( 'NONE',  ( 3.682264917456192777, 84.67546620154573134, 0.07358041635424013294 ) ) ;
#15784 = CARTESIAN_POINT ( 'NONE',  ( 17.27060146982319466, 122.7565812399420651, 0.2921901055230267108 ) ) ;
#15785 = CARTESIAN_POINT ( 'NONE',  ( -7.643893061813611389, 124.7210964017841377, -0.1527835634684687749 ) ) ;
#15786 = CIRCLE ( 'NONE', #2896, 0.5080000000000000071 ) ;
#15787 = CARTESIAN_POINT ( 'NONE',  ( -8.210443557797230341, 69.68696903609418314, -1.523999999999995802 ) ) ;
#15788 = CARTESIAN_POINT ( 'NONE',  ( 8.041889123127029748, 122.8518031662551948, 0.1606960833125207766 ) ) ;
#15789 = CARTESIAN_POINT ( 'NONE',  ( 19.44881300980840777, 136.0480396440595996, 2.307899331309748003 ) ) ;
#15790 = CARTESIAN_POINT ( 'NONE',  ( 0.3193725800214416988, -13.04287899337829515, -8.422265478599168631 ) ) ;
#15791 = CARTESIAN_POINT ( 'NONE',  ( 8.748550937609889999, 117.9820647352999003, -0.4023511751121509050 ) ) ;
#15792 = CARTESIAN_POINT ( 'NONE',  ( -0.2949767777650753042, 114.7739974199301116, -2.049407731665748411 ) ) ;
#15793 = CARTESIAN_POINT ( 'NONE',  ( -10.44685452804831804, 82.62549350906336088, -1.269999999999999130 ) ) ;
#15794 = CARTESIAN_POINT ( 'NONE',  ( -17.99070523305416813, 61.93444992276926797, -1.523999999999999799 ) ) ;
#15795 = CARTESIAN_POINT ( 'NONE',  ( 1.765626013768924807, -4.031643488171090972, 8.243228240708695864 ) ) ;
#15796 = CARTESIAN_POINT ( 'NONE',  ( -47.16890147375937659, 22.20336809214646578, -4.187060126831891438 ) ) ;
#15797 = FACE_OUTER_BOUND ( 'NONE', #24156, .T. ) ;
#15798 = CARTESIAN_POINT ( 'NONE',  ( 3.092642723064080279, -14.67800799544728285, 3.675123631970977911 ) ) ;
#15799 = CARTESIAN_POINT ( 'NONE',  ( 1.034729067459722485, 124.2655319029901335, -0.03890078971358913035 ) ) ;
#15800 = CARTESIAN_POINT ( 'NONE',  ( -0.009748065369249884343, 159.5507987164374981, 0.4878330526048098581 ) ) ;
#15801 = CIRCLE ( 'NONE', #7684, 0.3810000000000000053 ) ;
#15802 = ORIENTED_EDGE ( 'NONE', *, *, #22254, .F. ) ;
#15803 = CARTESIAN_POINT ( 'NONE',  ( 5.871452009091314039, 65.30181249999998272, 5.016499999999999737 ) ) ;
#15804 = ADVANCED_FACE ( 'NONE', ( #37860 ), #10614, .T. ) ;
#15805 = VERTEX_POINT ( 'NONE', #18548 ) ;
#15806 = CARTESIAN_POINT ( 'NONE',  ( -42.18385791109623995, 22.43440044418303714, -1.696665287888123208 ) ) ;
#15807 = CARTESIAN_POINT ( 'NONE',  ( 3.361984464572039144, -15.63109852379819564, 5.271848418269179604 ) ) ;
#15808 = CARTESIAN_POINT ( 'NONE',  ( -20.67621894907605196, 148.5655811199389689, 1.615315227278341537 ) ) ;
#15809 = CARTESIAN_POINT ( 'NONE',  ( 12.49407882476840115, 156.7420262770442037, -1.161473977901223531 ) ) ;
#15810 = EDGE_CURVE ( 'NONE', #16922, #329, #24045, .T. ) ;
#15811 = CARTESIAN_POINT ( 'NONE',  ( -1.214995109038484067, 0.9429784454696930052, -4.460028654918597901 ) ) ;
#15812 = CARTESIAN_POINT ( 'NONE',  ( -58.09669861156134374, 0.8533854034191163951, -1.257397024040518563 ) ) ;
#15813 = ORIENTED_EDGE ( 'NONE', *, *, #6532, .F. ) ;
#15814 = CARTESIAN_POINT ( 'NONE',  ( -57.55255837555640852, 1.471581310123148967, -1.351947345341661721 ) ) ;
#15815 = CARTESIAN_POINT ( 'NONE',  ( 0.3588522330932212845, 120.9711055683163323, 0.4900691623393884644 ) ) ;
#15816 = LINE ( 'NONE', #9028, #1907 ) ;
#15817 = CARTESIAN_POINT ( 'NONE',  ( -17.27955699683406721, 146.3482411845097886, 1.367784599882192476 ) ) ;
#15818 = CARTESIAN_POINT ( 'NONE',  ( -17.97610982144389524, 83.97333317030323485, 1.523999999999995802 ) ) ;
#15819 = CARTESIAN_POINT ( 'NONE',  ( 6.683041398157518742, 119.8184877057495754, -1.002300253150233411 ) ) ;
#15820 = CARTESIAN_POINT ( 'NONE',  ( -7.819746389599830927, 118.9574329095587757, -1.279815391681077275 ) ) ;
#15821 = CARTESIAN_POINT ( 'NONE',  ( -6.262914499211170494, 78.85772796343783853, 4.069400916056300943 ) ) ;
#15822 = AXIS2_PLACEMENT_3D ( 'NONE', #7340, #20095, #29700 ) ;
#15823 = ORIENTED_EDGE ( 'NONE', *, *, #29542, .T. ) ;
#15824 = CARTESIAN_POINT ( 'NONE',  ( 7.108627447324208148, 121.8675249661327626, -0.3373703349335457902 ) ) ;
#15825 = ORIENTED_EDGE ( 'NONE', *, *, #23245, .F. ) ;
#15826 = CARTESIAN_POINT ( 'NONE',  ( -10.86423259349712467, 154.4230204216147513, -2.019759596344636865 ) ) ;
#15827 = CARTESIAN_POINT ( 'NONE',  ( 3.037377538037926428, -15.29769487807139328, 4.066060606540134792 ) ) ;
#15828 = CARTESIAN_POINT ( 'NONE',  ( -4.112438057953108128, 118.2429491485453070, -0.3456707284627133503 ) ) ;
#15829 = AXIS2_PLACEMENT_3D ( 'NONE', #36819, #21020, #34043 ) ;
#15830 = CARTESIAN_POINT ( 'NONE',  ( 9.094996104468805243, 78.64197151092925253, -1.904999999999999583 ) ) ;
#15831 = TOROIDAL_SURFACE ( 'NONE', #26336, 8.794749999999996959, 0.2540000000000000036 ) ;
#15832 = CARTESIAN_POINT ( 'NONE',  ( -4.909535097854543118, 117.7132662139654684, 0.7284956952065094749 ) ) ;
#15833 = CARTESIAN_POINT ( 'NONE',  ( 17.32761985034175822, 148.7932787949812905, 2.272318092294528746 ) ) ;
#15834 = DIRECTION ( 'NONE',  ( 0.6675346791886971332, -0.7445787077807445309, -3.514707485634470267E-14 ) ) ;
#15835 = CARTESIAN_POINT ( 'NONE',  ( 0.2838385327444274964, 29.22985346960623332, -4.617364983570896086 ) ) ;
#15836 = CARTESIAN_POINT ( 'NONE',  ( 15.27538331669044780, 143.4753230507764670, 0.6393389556987906230 ) ) ;
#15837 = CARTESIAN_POINT ( 'NONE',  ( -10.39456080247344083, 81.94606122948148652, 1.270000000000000240 ) ) ;
#15839 = EDGE_LOOP ( 'NONE', ( #32024, #18230, #11513, #15686 ) ) ;
#15838 = CARTESIAN_POINT ( 'NONE',  ( -47.20049172920048619, 19.11349993950443249, -3.907078929042799853 ) ) ;
#15840 = CARTESIAN_POINT ( 'NONE',  ( -17.14500000000466784, 71.11999999999886768, -1.524000000000000909 ) ) ;
#15841 = DIRECTION ( 'NONE',  ( -0.8745520943968235761, 0.4849315768086558398, -4.268512490100410909E-16 ) ) ;
#15842 = CARTESIAN_POINT ( 'NONE',  ( -49.61317302244366090, 16.90600142608853318, 5.005032797918173237 ) ) ;
#15843 = CARTESIAN_POINT ( 'NONE',  ( -33.42971872652992005, 49.93539301574497102, -1.524000000000005572 ) ) ;
#15844 = CIRCLE ( 'NONE', #27416, 0.2539999999999997260 ) ;
#15845 = DIRECTION ( 'NONE',  ( 0.9998004120163608288, 0.000000000000000000, 0.01997839162482749342 ) ) ;
#15846 = CARTESIAN_POINT ( 'NONE',  ( -54.34407705511657127, 12.44913727002957415, 1.242021477015509578 ) ) ;
#15847 = CARTESIAN_POINT ( 'NONE',  ( -16.81673201796769845, 155.2524275687165982, -0.03818847721824999292 ) ) ;
#15848 = ORIENTED_EDGE ( 'NONE', *, *, #29037, .T. ) ;
#15849 = CARTESIAN_POINT ( 'NONE',  ( -52.41299847468118855, 17.00754718993399095, -1.481513115354252452 ) ) ;
#15850 = CARTESIAN_POINT ( 'NONE',  ( -7.796374419565617941, 122.5468937217193997, -0.4035712047578281503 ) ) ;
#15851 = CARTESIAN_POINT ( 'NONE',  ( 5.152689472752729039, 116.8412042436348912, 0.1029629964107459106 ) ) ;
#15852 = ORIENTED_EDGE ( 'NONE', *, *, #16581, .F. ) ;
#15853 = CARTESIAN_POINT ( 'NONE',  ( 1.626908944290321735, 115.7027889457816769, -1.667109174786431280 ) ) ;
#15854 = CARTESIAN_POINT ( 'NONE',  ( -9.242391706085612668, 124.1957968681474824, -0.3461533994140003068 ) ) ;
#15855 = CARTESIAN_POINT ( 'NONE',  ( 6.023256536641487635, -13.63339314725699225, 2.031454315062427796 ) ) ;
#15856 = CARTESIAN_POINT ( 'NONE',  ( -13.26523119301606002, 121.0513591912305316, 0.9938426049807239648 ) ) ;
#15857 = CARTESIAN_POINT ( 'NONE',  ( -5.124566020981691672, 116.9360569234986116, -0.3865489709985214795 ) ) ;
#15858 = TOROIDAL_SURFACE ( 'NONE', #40392, 0.7620000000000000107, 0.2540000000000000036 ) ;
#15859 = CARTESIAN_POINT ( 'NONE',  ( 22.81319227410996220, 150.4043717142618277, 0.6849243123989299242 ) ) ;
#15860 = CARTESIAN_POINT ( 'NONE',  ( 8.877428936179040164, 123.9526547814713950, 0.3101401378828683164 ) ) ;
#15861 = CARTESIAN_POINT ( 'NONE',  ( -5.177913976931285411, 57.14999999999998437, 5.372100000000002318 ) ) ;
#15862 = CARTESIAN_POINT ( 'NONE',  ( 0.9699771559235883522, 8.716109271805494885, -0.1015519487743763993 ) ) ;
#15863 = CARTESIAN_POINT ( 'NONE',  ( -6.903663268456499580, 117.1865127098105575, -0.2656477445430289186 ) ) ;
#15864 = FACE_OUTER_BOUND ( 'NONE', #21937, .T. ) ;
#15865 = EDGE_CURVE ( 'NONE', #1003, #3266, #25429, .T. ) ;
#15866 = VERTEX_POINT ( 'NONE', #26743 ) ;
#15867 = CARTESIAN_POINT ( 'NONE',  ( -8.690633472767538947, 118.2864615337380485, 0.6276850432433955795 ) ) ;
#15868 = ORIENTED_EDGE ( 'NONE', *, *, #29567, .T. ) ;
#15869 = CARTESIAN_POINT ( 'NONE',  ( -47.84356795211458291, 19.38525671449504983, 5.197506975155153697 ) ) ;
#15870 = CARTESIAN_POINT ( 'NONE',  ( 5.110479671343659547, 158.7070047875298826, 1.445852496635407824 ) ) ;
#15871 = CARTESIAN_POINT ( 'NONE',  ( 4.124323422701878350, 118.5849532427036905, -0.8258982430451993206 ) ) ;
#15872 = CARTESIAN_POINT ( 'NONE',  ( -7.300781474974964880, 17.39199087320084658, -4.267473507878162486 ) ) ;
#15873 = CARTESIAN_POINT ( 'NONE',  ( -21.70861548485266113, 150.3096123636779566, -1.869307503447338314 ) ) ;
#15874 = CARTESIAN_POINT ( 'NONE',  ( 4.749224635152644147, 117.9454780248063059, -0.6340590349429241490 ) ) ;
#15875 = DIRECTION ( 'NONE',  ( -0.8745520943968250194, 0.4849315768086535083, -5.424246918827963022E-16 ) ) ;
#15876 = CARTESIAN_POINT ( 'NONE',  ( -15.81024248929847964, 146.2514283349100594, -0.08545504004084561456 ) ) ;
#15877 = CARTESIAN_POINT ( 'NONE',  ( -3.283742410131533784, 119.1333808041459577, -0.8926212079385045239 ) ) ;
#15878 = CARTESIAN_POINT ( 'NONE',  ( 5.620948709224020234, -15.12563517700941951, 1.754161952847088868 ) ) ;
#15879 = CIRCLE ( 'NONE', #19978, 0.2540000000000052771 ) ;
#15880 = CARTESIAN_POINT ( 'NONE',  ( 4.744456427932504994, 118.5931160184169073, 1.015333858321567861 ) ) ;
#15881 = CARTESIAN_POINT ( 'NONE',  ( -43.87210973174860129, 22.05421410453335795, -2.454571855453439255 ) ) ;
#15882 = TOROIDAL_SURFACE ( 'NONE', #10450, 16.60960244842765832, 1.396999999999998909 ) ;
#15883 = ORIENTED_EDGE ( 'NONE', *, *, #35752, .F. ) ;
#15884 = CARTESIAN_POINT ( 'NONE',  ( 12.63334184343642796, 124.0847267554996591, 1.843480660383216563 ) ) ;
#15885 = CARTESIAN_POINT ( 'NONE',  ( -17.14500000000466784, 71.11999999999886768, -1.270000000000000684 ) ) ;
#15886 = VECTOR ( 'NONE', #32437, 1000.000000000000000 ) ;
#15887 = CARTESIAN_POINT ( 'NONE',  ( -3.075034626192941101, 115.9530684888725460, 1.465612804093755495 ) ) ;
#15888 = CARTESIAN_POINT ( 'NONE',  ( -3.468545696377880461, 29.88095345675903403, -7.690089085670218871 ) ) ;
#15889 = CARTESIAN_POINT ( 'NONE',  ( 13.85976170726103796, 150.2454140652271803, 1.103110692033626217 ) ) ;
#15890 = CARTESIAN_POINT ( 'NONE',  ( 22.38075128446548234, 150.2360280492587776, -0.6257272249761318683 ) ) ;
#15891 = CARTESIAN_POINT ( 'NONE',  ( -19.97113776634630611, 79.44829951959813741, 1.523999999999995802 ) ) ;
#15892 = TOROIDAL_SURFACE ( 'NONE', #28159, 3.683000000000000718, 0.5080000000000000071 ) ;
#15893 = CARTESIAN_POINT ( 'NONE',  ( -58.37116772670351850, -0.2940390518722524327, -2.603646672650065119E-13 ) ) ;
#15894 = EDGE_CURVE ( 'NONE', #10310, #1073, #40113, .T. ) ;
#15895 = CARTESIAN_POINT ( 'NONE',  ( -8.075779052176619288, 158.6620026115301698, -0.1430648235678988744 ) ) ;
#15896 = ORIENTED_EDGE ( 'NONE', *, *, #30451, .T. ) ;
#15897 = CARTESIAN_POINT ( 'NONE',  ( -8.196833826245901733, 120.4943603722682326, -1.426315956448065636 ) ) ;
#15898 = CARTESIAN_POINT ( 'NONE',  ( 22.98488057257191741, 150.1591296352320910, 0.4592926148156237232 ) ) ;
#15899 = AXIS2_PLACEMENT_3D ( 'NONE', #14812, #34852, #15654 ) ;
#15900 = CARTESIAN_POINT ( 'NONE',  ( -9.400309931224136051, 124.0858766813489780, -0.6109843400649569434 ) ) ;
#15901 = CARTESIAN_POINT ( 'NONE',  ( -5.146090777129525229, 116.8856917068506220, 0.08017679380233867781 ) ) ;
#15902 = CARTESIAN_POINT ( 'NONE',  ( 10.83330528665002923, 157.8980211815716928, 0.2164752214609689529 ) ) ;
#15903 = EDGE_CURVE ( 'NONE', #25560, #26298, #41730, .T. ) ;
#15904 = ORIENTED_EDGE ( 'NONE', *, *, #18547, .F. ) ;
#15905 = CARTESIAN_POINT ( 'NONE',  ( -2.359559261509405204, 14.11188314818778267, 3.974389579228013503 ) ) ;
#15906 = CARTESIAN_POINT ( 'NONE',  ( -29.20589784623331653, 64.40785669711193862, 1.269999999999897211 ) ) ;
#15907 = CARTESIAN_POINT ( 'NONE',  ( -5.008553077021508315, 117.3993868461436421, 0.7755932514345632578 ) ) ;
#15908 = CARTESIAN_POINT ( 'NONE',  ( -23.75997692595333177, 82.67351089148900201, -1.270000000000006235 ) ) ;
#15909 = CARTESIAN_POINT ( 'NONE',  ( -6.431420355030265265E-14, 156.3034662015457172, 9.897580308537652682E-17 ) ) ;
#15910 = CARTESIAN_POINT ( 'NONE',  ( -7.840345251802245841, 122.4018557723364040, 0.3085103408382670054 ) ) ;
#15911 = CARTESIAN_POINT ( 'NONE',  ( 1.100877510726109954, 5.750359496286542971, -4.487862572965156005 ) ) ;
#15912 = CARTESIAN_POINT ( 'NONE',  ( 10.25083424799698228, 157.8242135995235458, 1.281710951059998882 ) ) ;
#15913 = DIRECTION ( 'NONE',  ( -0.9998004120163608288, 0.000000000000000000, -0.01997839162482749342 ) ) ;
#15915 = CARTESIAN_POINT ( 'NONE',  ( 13.46025642088307883, 121.5866728338796463, -1.110021706884414261 ) ) ;
#15914 = CARTESIAN_POINT ( 'NONE',  ( 3.026662605148213725, -13.87242449132548217, 1.205013440933411228 ) ) ;
#15916 = CARTESIAN_POINT ( 'NONE',  ( 4.627658001546194555, 13.29687521248714610, 0.05192310334374634212 ) ) ;
#15917 = CARTESIAN_POINT ( 'NONE',  ( -1.349732659538083190, 159.5224216140176168, -0.6194554754934779028 ) ) ;
#15918 = AXIS2_PLACEMENT_3D ( 'NONE', #24690, #31091, #34714 ) ;
#15919 = VERTEX_POINT ( 'NONE', #7985 ) ;
#15920 = EDGE_CURVE ( 'NONE', #32786, #34625, #11642, .T. ) ;
#15921 = CARTESIAN_POINT ( 'NONE',  ( -12.05713894362187766, 151.9703418938154584, 0.4396675171196801069 ) ) ;
#15922 = CARTESIAN_POINT ( 'NONE',  ( 6.231544205925810154, -13.28212530995504004, 1.212557631246017564 ) ) ;
#15923 = CARTESIAN_POINT ( 'NONE',  ( -17.14500000000466784, 71.11999999999886768, -1.524000000000000909 ) ) ;
#15924 = CARTESIAN_POINT ( 'NONE',  ( -4.696919984883029642, 117.9693496385861380, -0.8143052264822483455 ) ) ;
#15925 = CARTESIAN_POINT ( 'NONE',  ( 9.049782359939477772, 124.0675141969884692, 0.1808361888366266657 ) ) ;
#15926 = ORIENTED_EDGE ( 'NONE', *, *, #30573, .T. ) ;
#15927 = EDGE_CURVE ( 'NONE', #9488, #41007, #31976, .T. ) ;
#15928 = CARTESIAN_POINT ( 'NONE',  ( 19.94553544501711428, 148.6304843473828043, 2.499072228797275308 ) ) ;
#15929 = CARTESIAN_POINT ( 'NONE',  ( 5.106395947886047004, 78.95054594174945350, 5.392902600000138769 ) ) ;
#15930 = AXIS2_PLACEMENT_3D ( 'NONE', #41960, #35147, #16148 ) ;
#15931 = DIRECTION ( 'NONE',  ( -0.8745520943968235761, 0.4849315768086558398, -4.268512490100410909E-16 ) ) ;
#15932 = CARTESIAN_POINT ( 'NONE',  ( -19.39512251848563906, 128.7092500879292345, 0.6293422422100684033 ) ) ;
#15933 = ADVANCED_FACE ( 'NONE', ( #19591 ), #10970, .T. ) ;
#15934 = CARTESIAN_POINT ( 'NONE',  ( -6.431420355030265265E-14, 156.3034662015457172, 9.897580308537652682E-17 ) ) ;
#15935 = CARTESIAN_POINT ( 'NONE',  ( 23.27509581586231491, 146.7258352529021863, -0.1368228026537801900 ) ) ;
#15936 = CARTESIAN_POINT ( 'NONE',  ( -4.910976174659007043, 115.7029491485453576, -1.454476526932306113 ) ) ;
#15937 = CARTESIAN_POINT ( 'NONE',  ( -46.75595590928379863, 25.85823223380729985, 1.409582097145047674 ) ) ;
#15938 = CARTESIAN_POINT ( 'NONE',  ( 5.614623559985534307, 78.91041036408813625, 5.070733448224204132 ) ) ;
#15939 = CARTESIAN_POINT ( 'NONE',  ( -4.757313731898603848, 117.4006812934349284, -1.206872148879561513 ) ) ;
#15940 = EDGE_CURVE ( 'NONE', #32067, #33842, #13160, .T. ) ;
#15941 = CARTESIAN_POINT ( 'NONE',  ( -47.11704014324646295, 20.18577099567727373, 5.127035723291425207 ) ) ;
#15942 = CARTESIAN_POINT ( 'NONE',  ( -58.66106266037335359, -0.3146683754999778926, 0.3235272937950393612 ) ) ;
#15943 = CARTESIAN_POINT ( 'NONE',  ( -4.652583246796857530, 118.0213927529021731, 0.6398161096456489449 ) ) ;
#15944 = EDGE_LOOP ( 'NONE', ( #12826, #19172, #35602, #6721 ) ) ;
#15945 = VERTEX_POINT ( 'NONE', #8986 ) ;
#15946 = CARTESIAN_POINT ( 'NONE',  ( -0.6720308294796238924, 115.6909491485452435, -1.760267559040072483 ) ) ;
#15947 = CARTESIAN_POINT ( 'NONE',  ( 3.456802958751930888, 118.5942819653431002, -0.7917318383961905459 ) ) ;
#15948 = CARTESIAN_POINT ( 'NONE',  ( -6.868335724905657358, 121.8312213470058225, -0.2935230024867366838 ) ) ;
#15949 = CARTESIAN_POINT ( 'NONE',  ( 4.798460879778644106, 117.8359694357527161, 0.9162085815312616122 ) ) ;
#15950 = CARTESIAN_POINT ( 'NONE',  ( 3.075357915497110017, -13.94103813162880989, 1.416127232796946966 ) ) ;
#15951 = CARTESIAN_POINT ( 'NONE',  ( -16.44150122627331001, 146.0252812507985141, -1.609049209688530935 ) ) ;
#15952 = CARTESIAN_POINT ( 'NONE',  ( -1.787119016036921693, 115.7029469008264186, -1.723302017833900912 ) ) ;
#15953 = CARTESIAN_POINT ( 'NONE',  ( -2.745631362450760893, 107.6373487222285235, 4.456378253842885329 ) ) ;
#15954 = CARTESIAN_POINT ( 'NONE',  ( -18.01920641645601151, 83.84822824455466161, -1.524000000000003352 ) ) ;
#15955 = CARTESIAN_POINT ( 'NONE',  ( 3.556334529072911366, 108.6891572770382624, -3.980722479600265817 ) ) ;
#15956 = CARTESIAN_POINT ( 'NONE',  ( -9.877803879600318027, 122.5082557396031291, -1.415055850893564227 ) ) ;
#15957 = DIRECTION ( 'NONE',  ( -1.000000000000000000, 1.011795553208986254E-16, 0.000000000000000000 ) ) ;
#15958 = CARTESIAN_POINT ( 'NONE',  ( -0.3252752853362120833, 37.07821745674546321, 2.201007984806573337 ) ) ;
#15959 = CARTESIAN_POINT ( 'NONE',  ( 6.059261036834405090, 56.51500000000000057, -4.381499999999999950 ) ) ;
#15960 = CARTESIAN_POINT ( 'NONE',  ( 4.440015753948663324, -2.305524871907271400, 1.325333094644747245 ) ) ;
#15962 = EDGE_LOOP ( 'NONE', ( #18435, #40701, #13473, #3074, #41227, #9396, #36780, #4840 ) ) ;
#15961 = CARTESIAN_POINT ( 'NONE',  ( 2.849674052733008889, 116.8186761214209213, 0.3958730627374474342 ) ) ;
#15963 = DIRECTION ( 'NONE',  ( 0.9575201071113187412, -0.2883665106726659433, -1.122696976216275637E-15 ) ) ;
#15964 = CARTESIAN_POINT ( 'NONE',  ( 3.489657270499090025, -15.47349394630789732, 3.491754635552897668 ) ) ;
#15965 = CARTESIAN_POINT ( 'NONE',  ( -12.68516923343336700, 122.7135068550949200, 1.328447112472142644 ) ) ;
#15966 = CARTESIAN_POINT ( 'NONE',  ( -0.7381358996182917354, 6.602865006980263018, -0.6401951644792284180 ) ) ;
#15967 = CARTESIAN_POINT ( 'NONE',  ( 0.8978640518332915432, -1.652899491467043180, 0.3817720442996600516 ) ) ;
#15968 = ORIENTED_EDGE ( 'NONE', *, *, #24603, .F. ) ;
#15969 = ORIENTED_EDGE ( 'NONE', *, *, #5827, .F. ) ;
#15970 = CARTESIAN_POINT ( 'NONE',  ( -41.31984638471809745, 22.80761424078405497, 1.396846000931794007 ) ) ;
#15971 = CARTESIAN_POINT ( 'NONE',  ( 3.148404055479938624, 118.0279923103727242, 0.8990514348027990321 ) ) ;
#15972 = CARTESIAN_POINT ( 'NONE',  ( -13.14213916796054349, 130.8944540161131442, 0.9043360416341286179 ) ) ;
#15973 = CARTESIAN_POINT ( 'NONE',  ( 3.009276887026297587, 39.20946620154573736, -1.210121013456480599 ) ) ;
#15974 = CARTESIAN_POINT ( 'NONE',  ( 2.810721824165392846, -14.60963343767143741, 5.218503737131710452 ) ) ;
#15975 = CARTESIAN_POINT ( 'NONE',  ( 12.06094766868686463, 124.3217332413628640, -1.226997676231848855 ) ) ;
#15976 = CARTESIAN_POINT ( 'NONE',  ( -19.13795181554008096, 149.5120288530235655, -2.492102325696694987 ) ) ;
#15977 = FACE_OUTER_BOUND ( 'NONE', #37938, .T. ) ;
#15978 = CARTESIAN_POINT ( 'NONE',  ( 1.824654213811243819, -15.25386490109567639, 5.420715704377902178 ) ) ;
#15979 = CARTESIAN_POINT ( 'NONE',  ( -0.02287401428062574640, 38.91018238071126945, -0.8096150143283803446 ) ) ;
#15980 = CARTESIAN_POINT ( 'NONE',  ( 0.6320890182442912009, 120.8998192842950488, -0.1133706938477902909 ) ) ;
#15981 = ADVANCED_FACE ( 'NONE', ( #34984 ), #15858, .T. ) ;
#15982 = ORIENTED_EDGE ( 'NONE', *, *, #29205, .T. ) ;
#15983 = CARTESIAN_POINT ( 'NONE',  ( -10.84307050033138786, 78.30450799593342026, 1.270000000000000240 ) ) ;
#15984 = ADVANCED_FACE ( 'NONE', ( #2400 ), #17950, .T. ) ;
#15985 = DIRECTION ( 'NONE',  ( -0.9454731675810336133, 0.3256999990547843615, -5.459396135145337199E-16 ) ) ;
#15986 = CARTESIAN_POINT ( 'NONE',  ( -0.006810764310409325381, 120.3493709785083183, 0.3408384964863779287 ) ) ;
#15987 = CARTESIAN_POINT ( 'NONE',  ( -24.57769139521899149, 76.70147894597536720, -1.524000000000005572 ) ) ;
#15988 = CARTESIAN_POINT ( 'NONE',  ( 22.53566265713729422, 150.7862151120626777, 0.3736683405004933012 ) ) ;
#15989 = EDGE_CURVE ( 'NONE', #2340, #40423, #23330, .T. ) ;
#15990 = CARTESIAN_POINT ( 'NONE',  ( -4.047044637104160181, 109.8183322527596602, 3.518666775989008677 ) ) ;
#15991 = EDGE_CURVE ( 'NONE', #33761, #38422, #7734, .T. ) ;
#15992 = DIRECTION ( 'NONE',  ( -5.206863593109713661E-17, 1.000000000000000000, -1.077750396879097183E-30 ) ) ;
#15993 = DIRECTION ( 'NONE',  ( -0.01997839162482737546, -1.040247600000940825E-18, 0.9998004120163610509 ) ) ;
#15994 = CARTESIAN_POINT ( 'NONE',  ( -4.460903749329073520, 31.58350409445925777, -0.5211678667172463530 ) ) ;
#15995 = CARTESIAN_POINT ( 'NONE',  ( 9.341440546823472246, 157.3305555497073271, 1.901068499721875193 ) ) ;
#15996 = VECTOR ( 'NONE', #20810, 1000.000000000000227 ) ;
#15997 = CARTESIAN_POINT ( 'NONE',  ( -1.220754042303205500, 16.12054255322086860, -4.471266627502475721 ) ) ;
#15998 = CARTESIAN_POINT ( 'NONE',  ( 4.725500162001525339, -13.89046571553399900, -6.993667195001821213 ) ) ;
#15999 = CARTESIAN_POINT ( 'NONE',  ( 5.512123453640334070, 117.2133480785072521, -0.5884807297197708342 ) ) ;
#16000 = CARTESIAN_POINT ( 'NONE',  ( 0.01254005783532663974, 120.1716774721351157, -0.6275557724548020966 ) ) ;
#16001 = CARTESIAN_POINT ( 'NONE',  ( -10.75478607932181241, 82.07015292912137738, 1.270000000000000684 ) ) ;
#16002 = CARTESIAN_POINT ( 'NONE',  ( 2.745797790083741141, 107.6376760790657698, -4.456235498929850714 ) ) ;
#16003 = CARTESIAN_POINT ( 'NONE',  ( -1.939848034429841217, 105.1240075698378575, 4.970163540756382226 ) ) ;
#16004 = CARTESIAN_POINT ( 'NONE',  ( 2.889066315880882030, 25.55657059589919911, 3.609430016826872478 ) ) ;
#16005 = DIRECTION ( 'NONE',  ( -0.8745520943968240202, 0.4849315768086551737, -5.361993529360572958E-16 ) ) ;
#16006 = CARTESIAN_POINT ( 'NONE',  ( -23.36555825341177339, 148.7788340588663800, -0.4668994608413308267 ) ) ;
#16007 = CARTESIAN_POINT ( 'NONE',  ( 2.969447359227861405, -13.80100253337253946, 0.9847735008004718793 ) ) ;
#16008 = CARTESIAN_POINT ( 'NONE',  ( 2.274554406286624975, 117.6064948828932444, -1.027890184761801384 ) ) ;
#16009 = CARTESIAN_POINT ( 'NONE',  ( -15.52007106302766282, 121.3130774642648220, 0.3850180365863631327 ) ) ;
#16010 = ORIENTED_EDGE ( 'NONE', *, *, #9209, .F. ) ;
#16011 = LINE ( 'NONE', #32636, #18863 ) ;
#16012 = ORIENTED_EDGE ( 'NONE', *, *, #35198, .T. ) ;
#16013 = DIRECTION ( 'NONE',  ( 0.9816537812491126225, 0.1906721105964872265, 8.537024980200846470E-16 ) ) ;
#16014 = CARTESIAN_POINT ( 'NONE',  ( 2.394017677299879576, -15.71294128685811486, 5.613897423981592638 ) ) ;
#16015 = CARTESIAN_POINT ( 'NONE',  ( -0.01111639779269613798, 118.2594330468507593, 0.5563100024230164253 ) ) ;
#16016 = CARTESIAN_POINT ( 'NONE',  ( 10.00431039430831248, 157.6892375622926181, -1.152258088200127650 ) ) ;
#16017 = CARTESIAN_POINT ( 'NONE',  ( 2.829288187452689396, 6.340478445469713620, 3.655570690059357197 ) ) ;
#16018 = CARTESIAN_POINT ( 'NONE',  ( -56.12001930601648070, 5.030854614368569955, -2.726109727168831931 ) ) ;
#16019 = ORIENTED_EDGE ( 'NONE', *, *, #37299, .T. ) ;
#16020 = CARTESIAN_POINT ( 'NONE',  ( -58.14608079600321133, 0.1881903270869317302, -0.6509722733302600872 ) ) ;
#16021 = CARTESIAN_POINT ( 'NONE',  ( 0.3855071059147253676, 123.1683257372383054, 0.1933446952578523892 ) ) ;
#16022 = CARTESIAN_POINT ( 'NONE',  ( -17.09258512000246100, 84.17916046765628835, -1.270000000000002904 ) ) ;
#16023 = B_SPLINE_SURFACE_WITH_KNOTS ( 'NONE', 3, 3, ( 
 ( #32348, #38539, #15729, #5761, #12548, #31937, #28934, #22110, #28734 ),
 ( #32143, #41327, #42160, #5966, #41747, #9354, #12753, #6169, #9153 ),
 ( #22316, #41952, #29143, #35342, #8939, #12130, #19546, #19342, #28531 ),
 ( #38957, #12955, #19139, #9555, #22527, #41536, #35556, #25949, #6372 ),
 ( #21905, #22732, #9768, #35763, #31723, #38335, #35139, #6790, #13177 ),
 ( #13387, #36406, #16789, #9973, #33209, #7640, #33414, #20184, #30206 ),
 ( #39166, #201, #4034, #16995, #26807, #39815, #36821, #29790, #23589 ),
 ( #7223, #629, #7011, #35973, #32996, #20389, #4458, #29994, #10819 ),
 ( #19756, #7431, #23802, #26588, #3825, #10401, #22946, #834, #36191 ),
 ( #39382, #13599, #13809, #39598, #29583, #14010, #23373, #40025, #32779 ),
 ( #20599, #26374, #19980, #10608, #4246, #3609, #36612, #17208, #1046 ),
 ( #27017, #33630, #16571, #29363, #26164, #417, #10185, #23154, #38021 ),
 ( #18406, #41225, #31413, #21805, #8842, #24588, #37801, #2255, #1828 ),
 ( #14792, #5239, #8421, #18194, #34619, #15430, #41439, #37595, #34205 ),
 ( #12459, #25236, #12027, #11819, #25019, #12244, #28002, #21379, #27795 ),
 ( #11604, #34832, #5666, #18623, #8627, #15217, #34405, #31628, #17990 ),
 ( #2677, #30987, #31195, #21590, #2468, #41011, #28432, #5446, #2038 ),
 ( #15003, #5032, #24808, #38240, #18834, #9057, #40803, #28219, #31838 ),
 ( #22022, #35050, #5871, #41651, #15635, #28640, #25453, #8205, #21177 ),
 ( #114, #6078, #9468, #38864, #25652, #15846, #29267, #36099, #19669 ),
 ( #32683, #38660, #22431, #19040, #16263, #35460, #10093, #9675, #6485 ),
 ( #39287, #3093, #22640, #19460, #9880, #3300, #6283, #28852, #16052 ),
 ( #13292, #12868, #32046, #9266, #16687, #16479, #19254, #32263, #6913 ),
 ( #35676, #29055, #42073, #25856, #32470, #23066, #13077, #26277, #29483 ),
 ( #22225, #41865, #534, #19883, #26068, #39078, #22850, #325, #35890 ),
 ( #2883, #29692, #12662, #6700, #3518, #32898, #3729, #13508, #38450 ),
 ( #35254, #39716, #20928, #7131, #23487, #26914, #36935, #4148, #40138 ),
 ( #741, #10720, #10516, #10307, #36512, #23919, #37139, #27337, #36311 ),
 ( #7960, #30734, #1367, #17111, #10930, #17732, #33319, #7755, #30112 ),
 ( #952, #11143, #23701, #13920, #40349, #23275, #33951, #4783, #24130 ),
 ( #20087, #17527, #36721, #39928, #33110, #7543, #20504, #14123, #7333 ),
 ( #33532, #20291, #4364, #1582, #13716, #26497, #17324, #39501, #30313 ),
 ( #1158, #27123, #14325, #20720, #3941, #16901, #29903, #4568, #26710 ),
 ( #33744, #30528, #14957, #21338, #18151, #14749, #37760, #28388, #24761 ) ),
 .UNSPECIFIED., .F., .F., .F.,
 ( 4, 1, 1, 1, 1, 1, 1, 1, 1, 1, 1, 2, 1, 1, 1, 1, 1, 1, 1, 1, 1, 1, 1, 1, 1, 1, 1, 1, 1, 1, 4 ),
 ( 4, 1, 1, 1, 1, 1, 4 ),
 ( 0.000000000000000000, 0.01653533301974152714, 0.03307066603948305428, 0.04960599905922458142, 0.06614133207896610855, 0.09921199811844916283, 0.1322826641579322171, 0.1653533301974152714, 0.1984239962368983257, 0.2314946622763813799, 0.2500000000000000000, 0.2645653283158644342, 0.3105299952961229071, 0.3335123287862520325, 0.3564946622763812689, 0.4024593292566397418, 0.4943886632171566875, 0.5863179971776735222, 0.6666666666666666297, 0.6782473311381906900, 0.7701766650987074136, 0.8161413320789658865, 0.8850883325493537068, 0.8965794992944182695, 0.9080706660394826102, 0.9195618327845473949, 0.9310529995296121797, 0.9425441662746769644, 0.9540353330197415271, 0.9770176665098706525, 1.000000000000000000 ),
 ( 0.000000000000000000, 0.2500000000000000000, 0.4444444444444445308, 0.5000000000000000000, 0.7500000000000000000, 0.8333333333333333703, 1.000000000000000000 ),
 .UNSPECIFIED. ) ;
#16024 = CARTESIAN_POINT ( 'NONE',  ( -2.563812760316581674, 119.9929590031203901, 0.5332384965226231177 ) ) ;
#16025 = CARTESIAN_POINT ( 'NONE',  ( -28.60507221318228943, 76.72702915747851193, 1.269999999999991358 ) ) ;
#16026 = CARTESIAN_POINT ( 'NONE',  ( 4.236690124160776172, 119.4047208153655646, -0.8054972593864422326 ) ) ;
#16027 = CARTESIAN_POINT ( 'NONE',  ( -14.93032553133231310, 154.7288491705591866, -2.132398917750006451 ) ) ;
#16028 = CARTESIAN_POINT ( 'NONE',  ( -58.07447437077728125, 1.735896131820596766, -1.499107834811110429 ) ) ;
#16029 = ORIENTED_EDGE ( 'NONE', *, *, #1445, .F. ) ;
#16030 = CARTESIAN_POINT ( 'NONE',  ( 4.493176929058669167, 118.1153340809138257, -0.5662424233016255526 ) ) ;
#16031 = CARTESIAN_POINT ( 'NONE',  ( 4.488166000884652007, 120.9326014760084007, -0.2785428184686806752 ) ) ;
#16032 = AXIS2_PLACEMENT_3D ( 'NONE', #26138, #22917, #23559 ) ;
#16033 = ORIENTED_EDGE ( 'NONE', *, *, #20043, .T. ) ;
#16034 = CARTESIAN_POINT ( 'NONE',  ( -0.5297590882382788857, 119.7690751942239729, -0.5117926329762007009 ) ) ;
#16035 = CARTESIAN_POINT ( 'NONE',  ( 3.302563718500166612, -15.23312206205887342, 3.441858572223985391 ) ) ;
#16036 = LINE ( 'NONE', #42056, #40843 ) ;
#16037 = CARTESIAN_POINT ( 'NONE',  ( -14.60888863026623952, 79.54114996201613508, 1.523999999999998467 ) ) ;
#16038 = CARTESIAN_POINT ( 'NONE',  ( -4.737627528408766331, 117.7521883752312419, 0.9000133201668191196 ) ) ;
#16039 = CARTESIAN_POINT ( 'NONE',  ( 15.36238541928142887, 134.8939017613128328, 2.058614936883395696 ) ) ;
#16040 = CARTESIAN_POINT ( 'NONE',  ( -1.606566256928684933, 32.19982401495065716, 1.077694121983206799 ) ) ;
#16041 = ADVANCED_FACE ( 'NONE', ( #11222 ), #9757, .T. ) ;
#16042 = CARTESIAN_POINT ( 'NONE',  ( 5.678980076864418969, -10.27674996446047828, -6.244917620322217644 ) ) ;
#16043 = CARTESIAN_POINT ( 'NONE',  ( 7.835359239711011448, 154.6110463214094182, 0.4315757689284727139 ) ) ;
#16044 = CARTESIAN_POINT ( 'NONE',  ( -51.58367816905025194, 14.91232437457545146, -4.609044670965841917 ) ) ;
#16045 = CARTESIAN_POINT ( 'NONE',  ( -44.40685758373556524, 19.43703734468909516, -6.894256627225939810E-15 ) ) ;
#16046 = CARTESIAN_POINT ( 'NONE',  ( -0.01811615190475213133, 118.1588900175948709, 0.9066062283863981497 ) ) ;
#16047 = CARTESIAN_POINT ( 'NONE',  ( -46.74696603144393237, 25.88044175092360888, -1.397587819153285338 ) ) ;
#16048 = CARTESIAN_POINT ( 'NONE',  ( -56.42620073798607194, 4.397991135091313453, 2.549475455950332758 ) ) ;
#16049 = CARTESIAN_POINT ( 'NONE',  ( -8.198442868473685863, 120.4868523889126095, -1.425315046605219127 ) ) ;
#16050 = DIRECTION ( 'NONE',  ( -0.1565721916417968096, -0.9876665170007964401, 0.000000000000000000 ) ) ;
#16051 = CARTESIAN_POINT ( 'NONE',  ( 6.059261036833980540, 78.87450423423040036, -5.016499999999999737 ) ) ;
#16052 = CARTESIAN_POINT ( 'NONE',  ( -55.80532936045926107, 9.325833942460080905, -1.040959450429527543E-14 ) ) ;
#16053 = CIRCLE ( 'NONE', #3160, 0.2539999999999998925 ) ;
#16054 = CARTESIAN_POINT ( 'NONE',  ( -3.772649051595033498, 116.7207137014398626, 0.1335598970234345428 ) ) ;
#16055 = TOROIDAL_SURFACE ( 'NONE', #28986, 0.7620000000000000107, 0.2540000000000000036 ) ;
#16056 = ORIENTED_EDGE ( 'NONE', *, *, #2384, .F. ) ;
#16057 = CARTESIAN_POINT ( 'NONE',  ( -55.15137202863810728, 10.98262019425784430, -0.5441000652716039276 ) ) ;
#16058 = CARTESIAN_POINT ( 'NONE',  ( -5.991689710969556160, 121.4334662389527466, -0.2049652515977599954 ) ) ;
#16059 = VERTEX_POINT ( 'NONE', #40224 ) ;
#16060 = CARTESIAN_POINT ( 'NONE',  ( 2.946371836444962256, 115.7030910448373788, -1.559712811386695819 ) ) ;
#16061 = CARTESIAN_POINT ( 'NONE',  ( -10.32597032162043682, 126.0505730134521230, -0.3842079712423248639 ) ) ;
#16062 = CARTESIAN_POINT ( 'NONE',  ( 3.036109343602874322, -15.28514977651167150, 5.695352409590039855 ) ) ;
#16063 = CARTESIAN_POINT ( 'NONE',  ( -14.28818831795934230, 121.8555783441548073, 1.022170725131337665 ) ) ;
#16064 = DIRECTION ( 'NONE',  ( 5.188838149069472160E-16, -1.699382548006136559E-16, -1.000000000000000000 ) ) ;
#16065 = CARTESIAN_POINT ( 'NONE',  ( 18.58235751530886404, 154.1615476314759974, 0.6802042707109063890 ) ) ;
#16066 = CARTESIAN_POINT ( 'NONE',  ( 14.67276854806925002, 148.8626603488974354, 0.4253145049176021986 ) ) ;
#16067 = DIRECTION ( 'NONE',  ( -0.8745520943968245753, 0.4849315768086539524, -5.691349986800526185E-16 ) ) ;
#16068 = CARTESIAN_POINT ( 'NONE',  ( 0.3244192847266222923, 10.43846528477952340, -0.9201954171864650256 ) ) ;
#16069 = CARTESIAN_POINT ( 'NONE',  ( -21.59686147024597247, 132.6646020023713959, -0.5653344646799387530 ) ) ;
#16070 = CARTESIAN_POINT ( 'NONE',  ( -14.42383115828894624, 69.61113539875873357, -1.269999999999998908 ) ) ;
#16071 = CARTESIAN_POINT ( 'NONE',  ( -10.15441061790785859, 81.86333342972157823, 1.270000000000000018 ) ) ;
#16072 = CARTESIAN_POINT ( 'NONE',  ( 5.530566976517129696, 117.1577684187682564, 0.7355826452304826679 ) ) ;
#16073 = ORIENTED_EDGE ( 'NONE', *, *, #27913, .F. ) ;
#16074 = CARTESIAN_POINT ( 'NONE',  ( -58.35078352787948575, -0.2517290638376923906, -0.1717528990698407032 ) ) ;
#16075 = CARTESIAN_POINT ( 'NONE',  ( 21.52700195390584526, 148.3057046726078170, 2.246165485461373290 ) ) ;
#16076 = CARTESIAN_POINT ( 'NONE',  ( 2.589082543892768484, 158.1729697732556588, -1.607049804855985586 ) ) ;
#16077 = CARTESIAN_POINT ( 'NONE',  ( -1.740095136297252543, 16.12223834230618635, -8.265420891812045312 ) ) ;
#16078 = CARTESIAN_POINT ( 'NONE',  ( -3.006067730438063634, 117.5448765310053005, -0.7098943453401749260 ) ) ;
#16079 = CARTESIAN_POINT ( 'NONE',  ( 4.827068429489758117, 117.7658018909618818, -0.8358721460697561279 ) ) ;
#16080 = CARTESIAN_POINT ( 'NONE',  ( -30.19451713491628553, 70.61549828015994024, -1.524000000000007571 ) ) ;
#16081 = CARTESIAN_POINT ( 'NONE',  ( -12.88210196283061038, 133.7932622986943159, -0.2101989309002755546 ) ) ;
#16082 = CARTESIAN_POINT ( 'NONE',  ( -18.01629081398026244, 149.0664087073519681, -2.421686302305671390 ) ) ;
#16083 = CARTESIAN_POINT ( 'NONE',  ( 5.478045763647380717, -15.20773871853380044, 2.260320276039294640 ) ) ;
#16084 =( BOUNDED_CURVE ( )  B_SPLINE_CURVE ( 3, ( #6881, #36278, #39684, #23671 ),
 .UNSPECIFIED., .F., .T. ) 
 B_SPLINE_CURVE_WITH_KNOTS ( ( 4, 4 ),
 ( 0.6486116422890977340, 0.6881516260757224446 ),
 .UNSPECIFIED. ) 
 CURVE ( )  GEOMETRIC_REPRESENTATION_ITEM ( )  RATIONAL_B_SPLINE_CURVE ( ( 0.5822367926346045941, 0.5608560245277020018, 0.5436443506017243354, 0.5306017708566714841 ) ) 
 REPRESENTATION_ITEM ( '' )  );
#16085 = DIRECTION ( 'NONE',  ( 9.627370216492862708E-17, 1.000000000000000000, -0.000000000000000000 ) ) ;
#16086 = CARTESIAN_POINT ( 'NONE',  ( -46.40591231939538375, 23.70796668624020853, -2.618124260499401945 ) ) ;
#16088 = ORIENTED_EDGE ( 'NONE', *, *, #21410, .F. ) ;
#16087 = VECTOR ( 'NONE', #4138, 999.9999999999998863 ) ;
#16089 = CARTESIAN_POINT ( 'NONE',  ( 0.5061634396315372042, 119.4440140289964774, 0.5640781084940280632 ) ) ;
#16090 = CARTESIAN_POINT ( 'NONE',  ( -15.52687642492895037, 147.5330934759543879, -0.3102639428822864254 ) ) ;
#16091 = DIRECTION ( 'NONE',  ( 2.458663194297837693E-13, 4.507549189546035939E-13, 1.000000000000000000 ) ) ;
#16092 = CARTESIAN_POINT ( 'NONE',  ( -0.4402454045157814244, 106.4201689084969047, 5.104646014783341457 ) ) ;
#16093 = CARTESIAN_POINT ( 'NONE',  ( -2.821688713678647709, 20.15627898171042176, -7.936949992814660071 ) ) ;
#16094 = CARTESIAN_POINT ( 'NONE',  ( 1.656170893581987658, 156.3096136994911092, 0.5768031348127033997 ) ) ;
#16095 = CARTESIAN_POINT ( 'NONE',  ( 22.08264656579475016, 150.6352520364973486, -0.6282006774575531471 ) ) ;
#16096 = CARTESIAN_POINT ( 'NONE',  ( 3.682264917456192332, 91.02546620154572565, 0.07358041635424013294 ) ) ;
#16098 = AXIS2_PLACEMENT_3D ( 'NONE', #11532, #37521, #18755 ) ;
#16097 = CARTESIAN_POINT ( 'NONE',  ( 6.485865538701863997, -14.69951297778787414, -0.2726410864842441772 ) ) ;
#16099 = AXIS2_PLACEMENT_3D ( 'NONE', #9010, #5619, #34160 ) ;
#16100 = CARTESIAN_POINT ( 'NONE',  ( -6.896656464550618537, 117.1676486657671177, -0.1232935741316916883 ) ) ;
#16101 = ORIENTED_EDGE ( 'NONE', *, *, #30576, .F. ) ;
#16102 = CARTESIAN_POINT ( 'NONE',  ( -6.449468943369818241, 120.2918880417729781, -1.168816612019687229 ) ) ;
#16103 = LINE ( 'NONE', #22279, #31908 ) ;
#16104 = VECTOR ( 'NONE', #7374, 1000.000000000000114 ) ;
#16105 = CARTESIAN_POINT ( 'NONE',  ( -14.86280047924408798, 148.8756053271976327, -1.012714816113364558 ) ) ;
#16106 = CARTESIAN_POINT ( 'NONE',  ( 4.273959209556542405, -12.80518358089995168, 2.504334382443756724 ) ) ;
#16107 = CARTESIAN_POINT ( 'NONE',  ( 6.059261036834405090, 56.51500000000000057, -4.381499999999999950 ) ) ;
#16108 = CARTESIAN_POINT ( 'NONE',  ( 18.63504953328963154, 154.1157618415863624, 0.3723726386282266709 ) ) ;
#16109 = EDGE_LOOP ( 'NONE', ( #11786, #13767, #24465, #14049 ) ) ;
#16110 = CARTESIAN_POINT ( 'NONE',  ( -0.2084201458593382406, 5.265951782950084592, 4.622859108429906883 ) ) ;
#16111 = CARTESIAN_POINT ( 'NONE',  ( -18.86374853661781970, 125.3403196291361610, -0.3769425889880998470 ) ) ;
#16112 = CARTESIAN_POINT ( 'NONE',  ( -5.008987216415587973, 117.3966124399498199, 0.7756614673512686187 ) ) ;
#16113 = DIRECTION ( 'NONE',  ( 5.188838149069472160E-16, -1.699382548006136559E-16, -1.000000000000000000 ) ) ;
#16114 = AXIS2_PLACEMENT_3D ( 'NONE', #19613, #9413, #35405 ) ;
#16115 = DIRECTION ( 'NONE',  ( -0.4849315768086426282, -0.8745520943968310146, -1.030032898892908135E-16 ) ) ;
#16116 = CARTESIAN_POINT ( 'NONE',  ( 7.813248254659782788, 122.4491652087703670, 0.5620385025197442985 ) ) ;
#16117 = CARTESIAN_POINT ( 'NONE',  ( 2.029292378383023898, 15.02103924000656043, -4.168288449772576065 ) ) ;
#16118 = CARTESIAN_POINT ( 'NONE',  ( 1.978713825503164436, 117.0827246868714013, 0.4887249842031142766 ) ) ;
#16119 = CARTESIAN_POINT ( 'NONE',  ( -0.06282972276541670675, 111.5577547982949227, 3.144256248693278355 ) ) ;
#16121 = CARTESIAN_POINT ( 'NONE',  ( 13.94573646207659223, 122.0315337860429423, -1.127490061167130575 ) ) ;
#16120 = CARTESIAN_POINT ( 'NONE',  ( 5.354045385558688253, 56.51499999999995794, 5.213862164400304700 ) ) ;
#16122 = CARTESIAN_POINT ( 'NONE',  ( 2.029292378383023898, 15.02103924000656043, -4.168288449772576065 ) ) ;
#16123 = CARTESIAN_POINT ( 'NONE',  ( -14.85510260296675966, 121.0052616771249347, -1.128405194827190705 ) ) ;
#16124 = ORIENTED_EDGE ( 'NONE', *, *, #32873, .F. ) ;
#16125 = CARTESIAN_POINT ( 'NONE',  ( -9.317815699932426199, 124.0984330410602183, 0.1356161447201457426 ) ) ;
#16126 = CARTESIAN_POINT ( 'NONE',  ( 4.669346286639404653, -14.72966438191931893, 4.552848284282712044 ) ) ;
#16127 = DIRECTION ( 'NONE',  ( 2.731847993664264244E-14, 2.731847993664264244E-14, -1.000000000000000000 ) ) ;
#16128 = CIRCLE ( 'NONE', #10702, 4.826000000000001400 ) ;
#16129 = ORIENTED_EDGE ( 'NONE', *, *, #25832, .F. ) ;
#16130 = CARTESIAN_POINT ( 'NONE',  ( 19.42875987905491897, 141.0981142166620259, 2.503406319619450482 ) ) ;
#16131 = CARTESIAN_POINT ( 'NONE',  ( -6.451606698686837575E-14, 65.62546620154573418, 4.217636114931141265E-29 ) ) ;
#16132 = CARTESIAN_POINT ( 'NONE',  ( -1.925929944387235853E-31, 0.000000000000000000, 0.000000000000000000 ) ) ;
#16133 = CARTESIAN_POINT ( 'NONE',  ( -14.88832262945836504, 121.0052616771249347, 0.5340607732653417372 ) ) ;
#16134 = ADVANCED_FACE ( 'NONE', ( #30397 ), #24206, .F. ) ;
#16135 = EDGE_CURVE ( 'NONE', #11942, #27588, #39698, .T. ) ;
#16136 = CARTESIAN_POINT ( 'NONE',  ( 11.66725022231030984, 17.14499999999999957, 5.016499999999999737 ) ) ;
#16137 = CIRCLE ( 'NONE', #39998, 0.7620000000000000107 ) ;
#16138 = CARTESIAN_POINT ( 'NONE',  ( 20.57623859521455856, 152.5775223076369400, -0.1637982859500252686 ) ) ;
#16139 = CARTESIAN_POINT ( 'NONE',  ( -5.449227423778994606, 57.14999999999997726, -5.145694933688813144 ) ) ;
#16140 = CARTESIAN_POINT ( 'NONE',  ( -46.75105655819150030, 25.87039714800365431, 1.402995854639100815 ) ) ;
#16141 = CARTESIAN_POINT ( 'NONE',  ( 5.675123159882344837, 78.90545016724973948, 5.052246757648558351 ) ) ;
#16142 = CARTESIAN_POINT ( 'NONE',  ( 1.734723475976807094E-15, 17.14499999999999957, 0.000000000000000000 ) ) ;
#16143 = CARTESIAN_POINT ( 'NONE',  ( -44.40534991575952972, 23.82367036525651116, 1.730788704199185624 ) ) ;
#16144 = CARTESIAN_POINT ( 'NONE',  ( -3.009276887026422820, 39.20946620154573736, 1.210121013456480377 ) ) ;
#16145 = CARTESIAN_POINT ( 'NONE',  ( -4.665163707145283389, 118.0184243076322019, 0.6237975492375645858 ) ) ;
#16146 = CARTESIAN_POINT ( 'NONE',  ( -5.981046608238790974, 78.88093534801386397, -5.016500000000000625 ) ) ;
#16147 = ORIENTED_EDGE ( 'NONE', *, *, #41455, .F. ) ;
#16148 = DIRECTION ( 'NONE',  ( -0.8745520943968236871, 0.4849315768086558953, -5.361993529360571971E-16 ) ) ;
#16149 = CARTESIAN_POINT ( 'NONE',  ( 8.429306250690459024, 119.6048990681906332, -1.079784194094564720 ) ) ;
#16150 = CARTESIAN_POINT ( 'NONE',  ( -7.563243396832136867, 124.2956292408697863, -0.1602470646927416087 ) ) ;
#16151 = CARTESIAN_POINT ( 'NONE',  ( 4.691553523908495116, 117.8976366721427098, 0.9736576180826594928 ) ) ;
#16152 = CARTESIAN_POINT ( 'NONE',  ( 2.666490510518176649, -13.49855353256042712, 0.05227394649444803282 ) ) ;
#16153 = CARTESIAN_POINT ( 'NONE',  ( -16.31317273256073719, 147.4903123243063590, -1.598834895054539018 ) ) ;
#16154 = TOROIDAL_SURFACE ( 'NONE', #12765, 0.7620000000000000107, 0.2540000000000000036 ) ;
#16155 = CYLINDRICAL_SURFACE ( 'NONE', #922, 1.270000000000000240 ) ;
#16156 = CARTESIAN_POINT ( 'NONE',  ( 12.69999999999999929, 16.51000000000000156, 1.555301434917138235E-15 ) ) ;
#16157 = CARTESIAN_POINT ( 'NONE',  ( -41.23752580366543441, 23.26788267949596900, -1.270000000000005125 ) ) ;
#16158 = CARTESIAN_POINT ( 'NONE',  ( 6.920469006311881444, 121.8192184429722005, -0.01800753507563494088 ) ) ;
#16159 = CARTESIAN_POINT ( 'NONE',  ( -16.52407570443684648, 148.2569838091642964, -1.909119861936069418 ) ) ;
#16160 = CARTESIAN_POINT ( 'NONE',  ( 0.000000000000000000, 0.000000000000000000, 0.000000000000000000 ) ) ;
#16161 = CARTESIAN_POINT ( 'NONE',  ( -6.426369768295692736E-14, 159.6054662015457382, 1.032716915552223178E-16 ) ) ;
#16162 = DIRECTION ( 'NONE',  ( -0.7071067811865504593, 8.659560562354968603E-17, 0.7071067811865445751 ) ) ;
#16163 = CARTESIAN_POINT ( 'NONE',  ( -4.637963820743935983, -6.603494994175692412, 0.1710436084038768345 ) ) ;
#16165 = EDGE_LOOP ( 'NONE', ( #15432, #25459, #30583, #40217 ) ) ;
#16164 = CARTESIAN_POINT ( 'NONE',  ( -0.008148259816616862383, 159.5682499516715040, 0.4077722408685187649 ) ) ;
#16166 = CARTESIAN_POINT ( 'NONE',  ( 5.314256358595446983, 104.6144662015457527, -0.4585142901829573625 ) ) ;
#16167 = CARTESIAN_POINT ( 'NONE',  ( 2.686089547800571964, -15.51909802064466248, 4.724564614977055044 ) ) ;
#16168 = CARTESIAN_POINT ( 'NONE',  ( -19.29133405012203895, 147.6776069388173767, 1.737063910747457474 ) ) ;
#16169 = CARTESIAN_POINT ( 'NONE',  ( 0.8777592251401162837, 3.590160258842859164, -0.4283581310676968790 ) ) ;
#16170 = CARTESIAN_POINT ( 'NONE',  ( -3.254034125433686864, 159.4600617640778353, -0.3425454502237990639 ) ) ;
#16171 = CARTESIAN_POINT ( 'NONE',  ( -0.02445332296907207215, 6.119348097484421878, 0.9755048060674135213 ) ) ;
#16172 = B_SPLINE_CURVE_WITH_KNOTS ( 'NONE', 3,
 ( #609, #19146, #12759, #22323 ),
 .UNSPECIFIED., .F., .F.,
 ( 4, 4 ),
 ( 0.000000000000000000, 0.9716897010375996624 ),
 .UNSPECIFIED. ) ;
#16173 = ADVANCED_FACE ( 'NONE', ( #13795 ), #1929, .T. ) ;
#16174 = VERTEX_POINT ( 'NONE', #2073 ) ;
#16175 = ORIENTED_EDGE ( 'NONE', *, *, #19746, .T. ) ;
#16176 = CARTESIAN_POINT ( 'NONE',  ( -44.22601141000046709, 20.28211486706537414, 1.272444536529917958 ) ) ;
#16177 = CARTESIAN_POINT ( 'NONE',  ( 5.429077642219811928, 122.7706071131974994, 0.2216225483982832978 ) ) ;
#16178 = PRODUCT_CONTEXT ( 'NONE', #35495, 'mechanical' ) ;
#16179 = CARTESIAN_POINT ( 'NONE',  ( -3.236331573563448583, 156.2293907256693331, 0.8668920366435202141 ) ) ;
#16180 = CARTESIAN_POINT ( 'NONE',  ( 3.658150719587269784, -13.97641594243527408, 4.344832359604154703 ) ) ;
#16181 = CARTESIAN_POINT ( 'NONE',  ( 13.85609184427558027, 152.5163154464351294, -1.589750347114883944 ) ) ;
#16182 = CARTESIAN_POINT ( 'NONE',  ( -5.838901281334665683, 119.0696708348911699, -1.193623469369258894 ) ) ;
#16183 = DIRECTION ( 'NONE',  ( -5.188838149069472160E-16, 1.699382548006136559E-16, 1.000000000000000000 ) ) ;
#16184 = CARTESIAN_POINT ( 'NONE',  ( 2.350639260211558668, -15.10312717587823705, 4.966175652281853203 ) ) ;
#16185 = CARTESIAN_POINT ( 'NONE',  ( -4.653079194867565604, 32.84790767926139665, 1.632299058096434496 ) ) ;
#16186 = CARTESIAN_POINT ( 'NONE',  ( 4.553626923285095884, 121.1438296405421937, -0.06679122792761491012 ) ) ;
#16187 = EDGE_LOOP ( 'NONE', ( #29961, #29669, #4722, #9999 ) ) ;
#16188 = DIRECTION ( 'NONE',  ( -0.9998004120163609398, 0.000000000000000000, -0.01997839162482749689 ) ) ;
#16189 = DIRECTION ( 'NONE',  ( 0.4849315768086480127, 0.8745520943968279060, 1.030032898892941415E-16 ) ) ;
#16190 =( GEOMETRIC_REPRESENTATION_CONTEXT ( 3 ) GLOBAL_UNCERTAINTY_ASSIGNED_CONTEXT ( ( #12081 ) ) GLOBAL_UNIT_ASSIGNED_CONTEXT ( ( #18962, #3014, #9593 ) ) REPRESENTATION_CONTEXT ( 'NONE', 'WORKASPACE' ) );
#16191 = CARTESIAN_POINT ( 'NONE',  ( 5.036073817479851833, 117.3993844285031116, -0.5500234170841655779 ) ) ;
#16192 = B_SPLINE_CURVE_WITH_KNOTS ( 'NONE', 3,
 ( #21147, #20945, #14556, #33970, #27563, #24356 ),
 .UNSPECIFIED., .F., .F.,
 ( 4, 2, 4 ),
 ( 0.000000000000000000, 0.5000000000000000000, 1.000000000000000000 ),
 .UNSPECIFIED. ) ;
#16193 = DIRECTION ( 'NONE',  ( 0.000000000000000000, 1.000000000000000000, 0.000000000000000000 ) ) ;
#16194 = CARTESIAN_POINT ( 'NONE',  ( 1.817820247522382138, 116.4909138135563040, -0.03564457049243154735 ) ) ;
#16195 = CARTESIAN_POINT ( 'NONE',  ( -0.1065646865916160396, 105.8844662015456777, 5.332932678536313809 ) ) ;
#16196 = DIRECTION ( 'NONE',  ( -4.017660918040594346E-17, 1.000000000000000000, 2.376309959284834438E-19 ) ) ;
#16197 = DIRECTION ( 'NONE',  ( -0.9336303900108815501, -0.3582377630124009560, -4.235673982319039874E-16 ) ) ;
#16198 = CARTESIAN_POINT ( 'NONE',  ( -4.843427198813659018, 31.50844634454021786, -0.7061668956633826433 ) ) ;
#16199 = ADVANCED_FACE ( 'NONE', ( #22059 ), #15670, .F. ) ;
#16200 = CARTESIAN_POINT ( 'NONE',  ( 18.56731909478072851, 131.8045874826418071, 2.147352672676718033 ) ) ;
#16201 = CARTESIAN_POINT ( 'NONE',  ( 2.233585966345281282, 24.54162662436292308, -4.064490141941544898 ) ) ;
#16202 = CARTESIAN_POINT ( 'NONE',  ( 8.391146056172745560, -15.30543149186461527, -0.4349570568239987667 ) ) ;
#16203 = CARTESIAN_POINT ( 'NONE',  ( 5.510923006218381381, 117.2511638274202994, -0.6088136109206577773 ) ) ;
#16204 = CARTESIAN_POINT ( 'NONE',  ( -0.5374927741466587472, 112.6282971158091470, -2.756357034314327326 ) ) ;
#16205 = CARTESIAN_POINT ( 'NONE',  ( -22.53527615164659892, 150.7831677823004952, -0.4503084484864786075 ) ) ;
#16206 = VECTOR ( 'NONE', #19202, 1000.000000000000000 ) ;
#16207 = CARTESIAN_POINT ( 'NONE',  ( -41.28107547821700507, 23.22158991241123616, 1.269999999999992912 ) ) ;
#16208 = CARTESIAN_POINT ( 'NONE',  ( -0.9365507687766482237, 105.1228617213538570, 5.262462312604806236 ) ) ;
#16209 = CARTESIAN_POINT ( 'NONE',  ( -2.029258473809828711, 23.83235028914373288, 4.157303687431403993 ) ) ;
#16210 = CARTESIAN_POINT ( 'NONE',  ( 1.650612623617701257E-15, 17.14499999999999957, 0.000000000000000000 ) ) ;
#16211 = CARTESIAN_POINT ( 'NONE',  ( -20.51686376604223128, 129.1072961674477710, -0.4099757654675940111 ) ) ;
#16212 = CARTESIAN_POINT ( 'NONE',  ( 2.995043271588619493, -14.66878921821561299, 4.005342282345994320 ) ) ;
#16213 = CARTESIAN_POINT ( 'NONE',  ( 2.226623034866197948, 116.5145642697238344, -1.365476420808193536 ) ) ;
#16214 = CARTESIAN_POINT ( 'NONE',  ( -22.83860824214441720, 149.7823008822066697, 0.3949144739309159990 ) ) ;
#16215 = ORIENTED_EDGE ( 'NONE', *, *, #14158, .T. ) ;
#16216 = EDGE_CURVE ( 'NONE', #36071, #13136, #10140, .T. ) ;
#16217 = DIRECTION ( 'NONE',  ( -0.8745520943968244643, 0.4849315768086544520, -4.268512490100399076E-16 ) ) ;
#16218 = EDGE_LOOP ( 'NONE', ( #10174, #38571, #39986, #38456 ) ) ;
#16219 = CARTESIAN_POINT ( 'NONE',  ( -26.37263903973852663, 72.23735686029533554, -1.524000000000005794 ) ) ;
#16220 = CARTESIAN_POINT ( 'NONE',  ( 3.900291174488768053, -15.73247852219369847, 4.461464635514134969 ) ) ;
#16221 = CARTESIAN_POINT ( 'NONE',  ( -0.4495176323323362699, 118.2558431149878402, 0.5768950177939178303 ) ) ;
#16222 = CARTESIAN_POINT ( 'NONE',  ( 14.19262213114343929, 155.9232964860746620, -1.164639009528572799 ) ) ;
#16223 = CARTESIAN_POINT ( 'NONE',  ( -0.5496829067194369811, 0.7180641350488168317, -4.598301960397928489 ) ) ;
#16224 = CARTESIAN_POINT ( 'NONE',  ( -58.56286374058253585, -0.1552305836484945689, -0.5530141226461045001 ) ) ;
#16225 = ORIENTED_EDGE ( 'NONE', *, *, #18291, .F. ) ;
#16226 = CARTESIAN_POINT ( 'NONE',  ( 3.174366308151880922, 88.99346620154574339, 0.06343139340882768262 ) ) ;
#16227 = CARTESIAN_POINT ( 'NONE',  ( -0.02135216056683805069, 118.1497763966934258, 1.068549427312529776 ) ) ;
#16228 = CARTESIAN_POINT ( 'NONE',  ( -6.350000000000036060, 57.14999999999998437, 7.776507174585692163E-16 ) ) ;
#16229 = CARTESIAN_POINT ( 'NONE',  ( -10.96277846527069322, 123.4376579628654014, 1.079141073574104492 ) ) ;
#16230 = DIRECTION ( 'NONE',  ( -0.9998004120163609398, 0.000000000000000000, -0.01997839162482749689 ) ) ;
#16231 = EDGE_CURVE ( 'NONE', #23452, #27418, #37842, .T. ) ;
#16232 = AXIS2_PLACEMENT_3D ( 'NONE', #13914, #26907, #7125 ) ;
#16233 = CARTESIAN_POINT ( 'NONE',  ( 17.15907173562165156, 135.3907879583883869, -1.705144375702607240 ) ) ;
#16234 = CARTESIAN_POINT ( 'NONE',  ( -11.58753624721098774, 156.3395478113760362, -2.047021040405474945 ) ) ;
#16235 = CARTESIAN_POINT ( 'NONE',  ( -57.07867440696631434, 2.606095844753547830, -1.988717289889820661 ) ) ;
#16236 = ADVANCED_FACE ( 'NONE', ( #5481 ), #4189, .T. ) ;
#16237 = EDGE_LOOP ( 'NONE', ( #10495, #30596, #28298, #7605 ) ) ;
#16238 = CARTESIAN_POINT ( 'NONE',  ( 4.496748124183634232, 118.1159772194654352, -0.5629342433147717095 ) ) ;
#16239 = CARTESIAN_POINT ( 'NONE',  ( 5.220694793870399586, 121.0999079655412203, -0.2922795305089893048 ) ) ;
#16240 = ORIENTED_EDGE ( 'NONE', *, *, #914, .T. ) ;
#16241 = CARTESIAN_POINT ( 'NONE',  ( -16.68865417205013912, 140.0893442862094673, -2.224985475129671375 ) ) ;
#16242 = CARTESIAN_POINT ( 'NONE',  ( 3.885490704569380060, -15.31119228946847777, 1.341400144935093630 ) ) ;
#16243 = CARTESIAN_POINT ( 'NONE',  ( -1.502787496059203809, 105.1237720616447007, -5.127625393460141900 ) ) ;
#16244 = CARTESIAN_POINT ( 'NONE',  ( -45.58494389689084869, 18.10922195552001313, -7.361215080689235889E-15 ) ) ;
#16245 = EDGE_CURVE ( 'NONE', #33280, #20566, #22291, .T. ) ;
#16246 = CARTESIAN_POINT ( 'NONE',  ( -4.930297673862535923, 117.6593853309075115, 0.7657671191340518213 ) ) ;
#16247 = CARTESIAN_POINT ( 'NONE',  ( 17.14723838084580976, 144.2986879860016529, 2.167616513504174947 ) ) ;
#16248 = CARTESIAN_POINT ( 'NONE',  ( -13.85159022459153988, 12.96416000000000146, -5.016499999999999737 ) ) ;
#16249 = CARTESIAN_POINT ( 'NONE',  ( -4.247245584637960647, 22.75789413176893206, 1.861891798430825862 ) ) ;
#16250 = CARTESIAN_POINT ( 'NONE',  ( -0.002459394113082844901, 156.3065584682211124, 0.1230781383047674232 ) ) ;
#16251 = CARTESIAN_POINT ( 'NONE',  ( 4.801216665947148243, 117.4032681888235459, -1.015537427445656782 ) ) ;
#16252 = AXIS2_PLACEMENT_3D ( 'NONE', #40307, #27706, #11725 ) ;
#16254 = VERTEX_POINT ( 'NONE', #24368 ) ;
#16253 = CARTESIAN_POINT ( 'NONE',  ( -47.93564525088164885, 15.36257551998183857, -8.154853246613427015E-15 ) ) ;
#16255 = AXIS2_PLACEMENT_3D ( 'NONE', #38973, #9990, #19774 ) ;
#16256 = CARTESIAN_POINT ( 'NONE',  ( 5.564921306486510844, 116.7072773883409837, -0.001268244569501262957 ) ) ;
#16257 = CARTESIAN_POINT ( 'NONE',  ( 20.69909148798437926, 152.5508394022677692, 0.4136171090298765285 ) ) ;
#16258 = CARTESIAN_POINT ( 'NONE',  ( -46.95911617132934879, 24.98948415085533270, 1.986615011824473864 ) ) ;
#16259 = DIRECTION ( 'NONE',  ( 0.9998004120163608288, 4.016384292689131511E-17, 0.01997839162482749342 ) ) ;
#16260 = CARTESIAN_POINT ( 'NONE',  ( -8.158575919685375766, 120.6841143662035734, -1.398758167514821515 ) ) ;
#16261 = CARTESIAN_POINT ( 'NONE',  ( -58.82991074935231524, -0.2577531494038359794, -1.058401375502683064E-14 ) ) ;
#16262 = DIRECTION ( 'NONE',  ( -5.206863593109713661E-17, 1.000000000000000000, -1.077750396879097183E-30 ) ) ;
#16263 = CARTESIAN_POINT ( 'NONE',  ( -54.91040913962392978, 10.45702928859090086, 1.592171597931398619 ) ) ;
#16264 = EDGE_CURVE ( 'NONE', #18747, #6508, #19266, .T. ) ;
#16265 = CARTESIAN_POINT ( 'NONE',  ( -57.39043856515510811, 2.569568763584578974, 1.997829887931748427 ) ) ;
#16266 = CARTESIAN_POINT ( 'NONE',  ( -23.25537431167569835, 149.3282167461061931, -0.1335628131362693594 ) ) ;
#16267 = EDGE_CURVE ( 'NONE', #15693, #24363, #39013, .T. ) ;
#16268 = ORIENTED_EDGE ( 'NONE', *, *, #24786, .F. ) ;
#16269 = CARTESIAN_POINT ( 'NONE',  ( -52.43464216530867361, 18.97776253654341616, -0.3470174342361405095 ) ) ;
#16270 = CARTESIAN_POINT ( 'NONE',  ( -7.790237900701975526, 122.5851110379722257, -0.3184765188668609581 ) ) ;
#16271 = ORIENTED_EDGE ( 'NONE', *, *, #6873, .T. ) ;
#16272 = CARTESIAN_POINT ( 'NONE',  ( 16.87828382557106721, 4.021169087505850551E-17, 0.000000000000000000 ) ) ;
#16273 = CARTESIAN_POINT ( 'NONE',  ( -15.39298062464846240, 147.8297367799732456, -0.5361660792469025161 ) ) ;
#16274 = CARTESIAN_POINT ( 'NONE',  ( 3.968318174290614397, -14.81366206205479763, 5.151173006574525814 ) ) ;
#16275 = CARTESIAN_POINT ( 'NONE',  ( -19.13467844095171344, 131.8899703912256314, 1.275959715510669001 ) ) ;
#16276 = DIRECTION ( 'NONE',  ( 5.188838149069472160E-16, -1.699382548006136559E-16, -1.000000000000000000 ) ) ;
#16277 = CARTESIAN_POINT ( 'NONE',  ( 20.67395311655588941, 152.5754960671270055, 0.6363119977773277203 ) ) ;
#16278 = CARTESIAN_POINT ( 'NONE',  ( 15.75762098209218465, 145.9019271191307610, 0.4493305750801200316 ) ) ;
#16279 = CARTESIAN_POINT ( 'NONE',  ( -10.57002714855771686, 82.40335727708655611, -1.523999999999999355 ) ) ;
#16280 = CARTESIAN_POINT ( 'NONE',  ( 0.7678286665867425365, 17.13787758575863762, 0.6011479000593502597 ) ) ;
#16281 = CARTESIAN_POINT ( 'NONE',  ( -11.68195978820582326, 118.7263634577040676, -0.3785536984881909262 ) ) ;
#16282 = B_SPLINE_CURVE_WITH_KNOTS ( 'NONE', 1,
 ( #18232, #31234 ),
 .UNSPECIFIED., .F., .F.,
 ( 2, 2 ),
 ( 0.04444444444444391878, 0.9701209927381800879 ),
 .UNSPECIFIED. ) ;
#16283 = DIRECTION ( 'NONE',  ( 1.000000000000000000, -1.365923996832131856E-16, 0.000000000000000000 ) ) ;
#16284 = FACE_OUTER_BOUND ( 'NONE', #33808, .T. ) ;
#16285 = ORIENTED_EDGE ( 'NONE', *, *, #23204, .F. ) ;
#16286 = CARTESIAN_POINT ( 'NONE',  ( 5.604777855449654567, 117.7098723955010513, 0.9801559107764311607 ) ) ;
#16287 = EDGE_LOOP ( 'NONE', ( #21343, #31078, #26364, #7018 ) ) ;
#16288 = CARTESIAN_POINT ( 'NONE',  ( 5.078986093043053707, 85.69146620154573668, 0.1014902294541244060 ) ) ;
#16289 = CARTESIAN_POINT ( 'NONE',  ( 2.895878334088767492, 159.0164033662945258, 1.329837440140976268 ) ) ;
#16290 = CARTESIAN_POINT ( 'NONE',  ( 12.76794581240257287, 122.4237789811383550, -1.308419224297318051 ) ) ;
#16291 = CARTESIAN_POINT ( 'NONE',  ( -0.7381358996182917354, 6.602865006980263018, -0.6401951644792284180 ) ) ;
#16292 = CARTESIAN_POINT ( 'NONE',  ( -7.817010796087602742, 17.61996943312679775, -3.135079784279759085 ) ) ;
#16293 = CARTESIAN_POINT ( 'NONE',  ( -19.25714749039855889, 152.1947311750261065, -2.059892502987373142 ) ) ;
#16294 = CARTESIAN_POINT ( 'NONE',  ( 4.756981263701162810, 117.8474050189492459, -0.8188388414369660584 ) ) ;
#16295 = EDGE_CURVE ( 'NONE', #23403, #21375, #25905, .T. ) ;
#16296 = CARTESIAN_POINT ( 'NONE',  ( 5.345964095105256497, 116.9256180743815179, 0.9586058045032991304 ) ) ;
#16297 = AXIS2_PLACEMENT_3D ( 'NONE', #28151, #23951, #15360 ) ;
#16298 = ADVANCED_FACE ( 'NONE', ( #35238 ), #41637, .T. ) ;
#16299 = CARTESIAN_POINT ( 'NONE',  ( 17.00728043862065419, 146.2370505443881257, -1.250989154318494334 ) ) ;
#16300 = CARTESIAN_POINT ( 'NONE',  ( -15.38068278028571712, 147.8292851303062321, -0.2562860988859086975 ) ) ;
#16301 = ORIENTED_EDGE ( 'NONE', *, *, #2888, .F. ) ;
#16302 = CARTESIAN_POINT ( 'NONE',  ( -5.834721624102832571, 119.7498067647950961, -1.158144809029191702 ) ) ;
#16304 = CARTESIAN_POINT ( 'NONE',  ( 2.079639979227050350, -15.65372482070806548, 5.795360105834356013 ) ) ;
#16303 = CIRCLE ( 'NONE', #40128, 8.794749999999996959 ) ;
#16305 = CARTESIAN_POINT ( 'NONE',  ( 4.770534990627869121, 118.5931160184169073, 0.9880304185510659920 ) ) ;
#16306 = CARTESIAN_POINT ( 'NONE',  ( -48.08949201794742123, 19.91830422262442468, -5.194343260851647770 ) ) ;
#16307 = EDGE_LOOP ( 'NONE', ( #22116, #13081, #6613, #25675 ) ) ;
#16308 = CARTESIAN_POINT ( 'NONE',  ( -0.03066982525788402442, 157.3074135339440147, 1.534843470138540500 ) ) ;
#16309 = LINE ( 'NONE', #29095, #19515 ) ;
#16310 = FACE_OUTER_BOUND ( 'NONE', #19438, .T. ) ;
#16311 = CARTESIAN_POINT ( 'NONE',  ( -4.257294657327928000, 122.9893884486272526, 0.03029934543357451493 ) ) ;
#16312 = CARTESIAN_POINT ( 'NONE',  ( 5.644239659282993316, 25.55377913558855596, 6.252972086369320337 ) ) ;
#16313 = CARTESIAN_POINT ( 'NONE',  ( -0.003756957834558761079, 120.7746249494737896, 0.1880135328902411695 ) ) ;
#16314 = CARTESIAN_POINT ( 'NONE',  ( 13.14342457437316192, 119.8381915656929380, -0.4562891928474252512 ) ) ;
#16315 = CARTESIAN_POINT ( 'NONE',  ( -47.72134626992409778, 19.52826264939519163, -5.191136457097766943 ) ) ;
#16316 = DIRECTION ( 'NONE',  ( -0.9998004120163608288, 0.000000000000000000, -0.01997839162482749342 ) ) ;
#16317 = UNCERTAINTY_MEASURE_WITH_UNIT (LENGTH_MEASURE( 1.000000000000000082E-05 ), #37942, 'distance_accuracy_value', 'NONE');
#16318 = CARTESIAN_POINT ( 'NONE',  ( -13.69580498508147137, 119.6466660129326272, -0.2573648061928515696 ) ) ;
#16319 = VERTEX_POINT ( 'NONE', #12852 ) ;
#16320 = CARTESIAN_POINT ( 'NONE',  ( -6.315404033698660768, 119.9964383445381344, -1.210168696518489462 ) ) ;
#16321 = DIRECTION ( 'NONE',  ( -0.01997839162482749342, -1.040247600000944484E-18, 0.9998004120163608288 ) ) ;
#16322 = CARTESIAN_POINT ( 'NONE',  ( -1.557716402914305798, 120.7946061759640486, -0.2396963980366530189 ) ) ;
#16323 = CARTESIAN_POINT ( 'NONE',  ( 3.244298476066852732, -14.49340328532226785, 5.143112664727522265 ) ) ;
#16324 = CARTESIAN_POINT ( 'NONE',  ( -5.152838217380527830, 116.8470107115679468, -0.02676777192457512403 ) ) ;
#16325 = CARTESIAN_POINT ( 'NONE',  ( 21.90559427349690935, 151.4293160993575498, 0.4377259060014666026 ) ) ;
#16326 = VERTEX_POINT ( 'NONE', #25436 ) ;
#16327 = CARTESIAN_POINT ( 'NONE',  ( -3.998286381996895233, 3.741657206818807424, 2.332027183294827832 ) ) ;
#16328 = CARTESIAN_POINT ( 'NONE',  ( -0.8838529761741459323, 116.4325158421065680, -0.01766148591713726304 ) ) ;
#16329 = CARTESIAN_POINT ( 'NONE',  ( -4.999701296913731774, 117.4056873544018487, 0.8305309289140377915 ) ) ;
#16330 = CARTESIAN_POINT ( 'NONE',  ( 17.14499999999999957, 71.11999999999999034, 5.016499999999999737 ) ) ;
#16331 = CARTESIAN_POINT ( 'NONE',  ( 6.946787401000980466, 121.0168171694836019, 1.036538389785776282 ) ) ;
#16332 =( BOUNDED_SURFACE ( )  B_SPLINE_SURFACE ( 3, 2, ( 
 ( #21394, #1843, #8644 ),
 ( #24396, #41453, #5680 ),
 ( #11618, #31209, #2692 ),
 ( #31853, #5254, #37610 ) ),
 .UNSPECIFIED., .F., .F., .T. ) 
 B_SPLINE_SURFACE_WITH_KNOTS ( ( 4, 4 ),
 ( 3, 3 ),
 ( 0.001248090998549182236, 0.001439255081647348349 ),
 ( 0.000000000000000000, 0.2830925978542064847 ),
 .UNSPECIFIED. ) 
 GEOMETRIC_REPRESENTATION_ITEM ( )  RATIONAL_B_SPLINE_SURFACE ( (
 ( 1.000000000000000000, 0.9321727843773290889, 0.9027483341063369249),
 ( 1.000000000000000000, 0.9321727478157031399, 0.9027482816837362201),
 ( 1.000000000000000000, 0.9321727022987384981, 0.9027482164208384674),
 ( 1.000000000000000000, 0.9321727023713098914, 0.9027482165248924550) ) ) 
 REPRESENTATION_ITEM ( '' )  SURFACE ( )  );
#16333 = CARTESIAN_POINT ( 'NONE',  ( -4.255528399684056495, 7.899375212487111497, -1.818898740287305138 ) ) ;
#16334 = CARTESIAN_POINT ( 'NONE',  ( 1.323305960456815811, 159.4649289425152858, 0.7771481453362867331 ) ) ;
#16335 = CARTESIAN_POINT ( 'NONE',  ( -14.64596739026573857, 69.73430801926814127, 1.269999999999999796 ) ) ;
#16337 = CARTESIAN_POINT ( 'NONE',  ( 20.59592450876350966, 149.8464234248869786, -1.516103928358539354 ) ) ;
#16336 = CARTESIAN_POINT ( 'NONE',  ( 4.918266948218991352, 56.51499999999997215, 4.748921713023384505 ) ) ;
#16338 = CARTESIAN_POINT ( 'NONE',  ( -4.609865753310859127, 8.349128549105346409, -0.5081561704775721111 ) ) ;
#16339 = CARTESIAN_POINT ( 'NONE',  ( -16.28621419528974101, 155.1963085991477271, -1.407434501154738449 ) ) ;
#16340 = AXIS2_PLACEMENT_3D ( 'NONE', #34071, #30435, #8279 ) ;
#16341 = ORIENTED_EDGE ( 'NONE', *, *, #32859, .T. ) ;
#16342 = CARTESIAN_POINT ( 'NONE',  ( -15.85793921209448243, 146.6055793175013093, 0.1365194753024331908 ) ) ;
#16343 = CARTESIAN_POINT ( 'NONE',  ( 5.816378023188423896, -13.23522671163289388, 2.128111738716565338 ) ) ;
#16344 = VECTOR ( 'NONE', #23421, 1000.000000000000000 ) ;
#16345 = CARTESIAN_POINT ( 'NONE',  ( -26.29578028364076658, 73.87584665086983193, 1.269999999999993134 ) ) ;
#16346 = CARTESIAN_POINT ( 'NONE',  ( -1.770057497934276691, 106.3924174363319821, -5.031961110743496057 ) ) ;
#16347 = ORIENTED_EDGE ( 'NONE', *, *, #6404, .F. ) ;
#16348 = CARTESIAN_POINT ( 'NONE',  ( 2.398927117898916883, 157.8629595415303584, 1.727538386417435401 ) ) ;
#16349 = DIRECTION ( 'NONE',  ( 9.627370216492862708E-17, 1.000000000000000000, -0.000000000000000000 ) ) ;
#16350 = FACE_OUTER_BOUND ( 'NONE', #4384, .T. ) ;
#16351 = CARTESIAN_POINT ( 'NONE',  ( -3.877771370679356622, 117.0975898859979054, 0.4181078409183316413 ) ) ;
#16352 = AXIS2_PLACEMENT_3D ( 'NONE', #13547, #1404, #6955 ) ;
#16353 = CARTESIAN_POINT ( 'NONE',  ( 2.823947636868042288, 116.6946238705719594, -0.1909394059425170709 ) ) ;
#16354 = CARTESIAN_POINT ( 'NONE',  ( -13.85159022459154166, 60.48513866567135722, 5.016500000000000625 ) ) ;
#16355 = CARTESIAN_POINT ( 'NONE',  ( -50.35389404691220960, 15.58445134054611003, 4.726195680281481515 ) ) ;
#16356 = CARTESIAN_POINT ( 'NONE',  ( -3.456281358658260583, 50.63946620154572997, -1.847419665314800508 ) ) ;
#16357 = CIRCLE ( 'NONE', #30667, 0.3810000000000029474 ) ;
#16358 = DIRECTION ( 'NONE',  ( 0.000000000000000000, -0.000000000000000000, 1.000000000000000000 ) ) ;
#16359 = CARTESIAN_POINT ( 'NONE',  ( -51.54051843738712080, 14.84038450301108192, 4.692172599169413871 ) ) ;
#16360 = LINE ( 'NONE', #39169, #15758 ) ;
#16361 = CARTESIAN_POINT ( 'NONE',  ( -4.592204290372686515, 118.0393302332859378, 0.6628552400479452711 ) ) ;
#16362 = CARTESIAN_POINT ( 'NONE',  ( -5.624629865489270131, 78.90958242041959636, -5.067363953418781541 ) ) ;
#16363 = PRODUCT_DEFINITION_SHAPE ( 'NONE', 'NONE',  #37297 ) ;
#16364 = ORIENTED_EDGE ( 'NONE', *, *, #21925, .T. ) ;
#16365 = CARTESIAN_POINT ( 'NONE',  ( -0.07233785497491922178, 118.7629491485454025, -1.278895185737845441 ) ) ;
#16366 = CARTESIAN_POINT ( 'NONE',  ( -3.439708463638626590, 118.6150900816448797, -0.9303604156532724323 ) ) ;
#16367 = CARTESIAN_POINT ( 'NONE',  ( -7.089375086750039578, 122.4291926079955317, -0.2513136963589432393 ) ) ;
#16369 = CARTESIAN_POINT ( 'NONE',  ( 4.694918129094446613, 117.9582486484168982, 0.8614738248342319604 ) ) ;
#16368 = AXIS2_PLACEMENT_3D ( 'NONE', #37902, #18083, #15721 ) ;
#16370 = CARTESIAN_POINT ( 'NONE',  ( -46.95766867967832070, 25.94401225812155332, -9.481001462019121602E-15 ) ) ;
#16371 = CARTESIAN_POINT ( 'NONE',  ( -9.985636026282492139, 124.1433363813624311, -1.001463123883985729 ) ) ;
#16372 = CARTESIAN_POINT ( 'NONE',  ( -3.627500158948379294, 115.7029588711417887, -1.619953353561904619 ) ) ;
#16373 = CARTESIAN_POINT ( 'NONE',  ( 1.650612623617701257E-15, 17.14499999999999957, 0.000000000000000000 ) ) ;
#16374 = FACE_OUTER_BOUND ( 'NONE', #720, .T. ) ;
#16375 = CARTESIAN_POINT ( 'NONE',  ( 0.1065646865914870178, 105.8844662015456919, -5.332932678536313809 ) ) ;
#16376 = CARTESIAN_POINT ( 'NONE',  ( 0.02400040557466870741, 156.7459281804771365, -1.201078436782489378 ) ) ;
#16377 = CARTESIAN_POINT ( 'NONE',  ( -13.76130258807007500, 16.83823567964705958, -5.016499999999998849 ) ) ;
#16378 = CARTESIAN_POINT ( 'NONE',  ( -0.0008202526018428905668, 159.6052337359418800, 0.04104879434819971862 ) ) ;
#16379 = CARTESIAN_POINT ( 'NONE',  ( -2.969549164036747957, 115.7030431952828735, 1.557416231888924196 ) ) ;
#16380 = CARTESIAN_POINT ( 'NONE',  ( -1.560048624214163793, 156.2601855860432067, 0.007372770612580329189 ) ) ;
#16381 = CARTESIAN_POINT ( 'NONE',  ( 1.398650104629075797, 0.06838872207683838189, -4.420329592304430122 ) ) ;
#16383 = ORIENTED_EDGE ( 'NONE', *, *, #3424, .T. ) ;
#16382 = CARTESIAN_POINT ( 'NONE',  ( 22.91074218474003032, 142.4877946823990271, 1.320775467724695007 ) ) ;
#16384 = CARTESIAN_POINT ( 'NONE',  ( -8.428339483816529309, 74.57444062528223583, 1.270000000000002238 ) ) ;
#16385 = CARTESIAN_POINT ( 'NONE',  ( 3.506097670019660217, -15.11506922876175452, 2.387495833752258267 ) ) ;
#16386 = CARTESIAN_POINT ( 'NONE',  ( -13.98553986197822852, 125.7699432187419575, 1.444593012458400105 ) ) ;
#16387 = CARTESIAN_POINT ( 'NONE',  ( 0.1179719058304127544, 10.27755972103446958, 0.9685762618712100425 ) ) ;
#16388 = CARTESIAN_POINT ( 'NONE',  ( -13.35680032055093847, 119.7032035076741465, -0.7543780172957895713 ) ) ;
#16389 = CARTESIAN_POINT ( 'NONE',  ( 0.9616503885695291132, 8.288457568681202758, 0.1719041247055087540 ) ) ;
#16390 = ORIENTED_EDGE ( 'NONE', *, *, #17820, .T. ) ;
#16391 = EDGE_LOOP ( 'NONE', ( #26243, #37086, #11561, #34788, #3178 ) ) ;
#16392 = CARTESIAN_POINT ( 'NONE',  ( -42.80040666669066241, 21.79149265709745009, 2.067570201390446449 ) ) ;
#16393 = CARTESIAN_POINT ( 'NONE',  ( 5.194452014863536249, 116.1170857923940787, 1.235891685093609915 ) ) ;
#16394 = CARTESIAN_POINT ( 'NONE',  ( -10.90887028606303666, 153.1125297277760069, 0.8016274872379889338 ) ) ;
#16395 = CARTESIAN_POINT ( 'NONE',  ( 3.097180478269691672, -14.43375334869456594, 4.992610980676636778 ) ) ;
#16396 = CARTESIAN_POINT ( 'NONE',  ( 17.22187362939829214, 148.7218176724978775, -1.531815132551777037 ) ) ;
#16397 = CARTESIAN_POINT ( 'NONE',  ( -19.60096582671588550, 145.2539617268756729, -2.527680105953240552 ) ) ;
#16398 = CARTESIAN_POINT ( 'NONE',  ( 2.958531772299236362, 39.20946620154573736, 1.329372033065076231 ) ) ;
#16399 = AXIS2_PLACEMENT_3D ( 'NONE', #11953, #37944, #40935 ) ;
#16400 = CARTESIAN_POINT ( 'NONE',  ( 2.768561164044480272, -13.57843041371762460, 0.3119852368007841603 ) ) ;
#16401 = CARTESIAN_POINT ( 'NONE',  ( -0.5321123018419734452, 37.22158963861809156, -0.7300149017649122385 ) ) ;
#16402 = CARTESIAN_POINT ( 'NONE',  ( 5.269990328701441129, 121.3020066425206807, -0.06069006697729611988 ) ) ;
#16403 = ORIENTED_EDGE ( 'NONE', *, *, #7939, .T. ) ;
#16404 = DIRECTION ( 'NONE',  ( -1.000000000000000000, 0.000000000000000000, 0.000000000000000000 ) ) ;
#16405 = CARTESIAN_POINT ( 'NONE',  ( -7.917360960270791281, 70.00264313970245666, 1.524000000000003574 ) ) ;
#16406 = AXIS2_PLACEMENT_3D ( 'NONE', #27836, #5486, #38278 ) ;
#16407 = LINE ( 'NONE', #32827, #782 ) ;
#16408 = CARTESIAN_POINT ( 'NONE',  ( -13.83234216238653680, 16.68269501491596785, 5.016499999999998849 ) ) ;
#16409 = CARTESIAN_POINT ( 'NONE',  ( 13.42085051059965828, 156.9389434127184018, 0.1400394208249338968 ) ) ;
#16410 = CARTESIAN_POINT ( 'NONE',  ( -6.130181428581336966, 119.5149100643186983, 0.2724793030934819504 ) ) ;
#16411 = VECTOR ( 'NONE', #23654, 1000.000000000000114 ) ;
#16412 = CARTESIAN_POINT ( 'NONE',  ( -1.447287616209143035, 115.6909491485452435, 1.681827335203893936 ) ) ;
#16413 = CARTESIAN_POINT ( 'NONE',  ( 4.560362914109654220, -11.68884639558073069, 0.6953251057713033534 ) ) ;
#16414 = CARTESIAN_POINT ( 'NONE',  ( -3.514327769487986419, 32.73121309073282958, 1.058241958670834704 ) ) ;
#16415 = CARTESIAN_POINT ( 'NONE',  ( 13.26090510203103179, 121.6721647909590303, 1.681263517196597945 ) ) ;
#16416 = CARTESIAN_POINT ( 'NONE',  ( 3.912982837994093188, 14.17146771520798332, -2.459658384584827218 ) ) ;
#16417 = CARTESIAN_POINT ( 'NONE',  ( 8.129739676946041271, 26.40327925692461619, 2.337594602388961107 ) ) ;
#16418 = CARTESIAN_POINT ( 'NONE',  ( -8.686247397591175812, 118.1594658427179780, -0.8950587481708219828 ) ) ;
#16419 = CARTESIAN_POINT ( 'NONE',  ( -0.4574053846283027691, 111.1955024190080223, -3.269098021338873838 ) ) ;
#16420 = FACE_OUTER_BOUND ( 'NONE', #12656, .T. ) ;
#16421 = CIRCLE ( 'NONE', #37533, 2.540000000000000480 ) ;
#16422 = CARTESIAN_POINT ( 'NONE',  ( 0.1701459486970862411, 105.9762159740997305, -5.294439841319366735 ) ) ;
#16423 = CARTESIAN_POINT ( 'NONE',  ( -0.2157595709654898941, 104.6144662015456390, 4.831689808425918109 ) ) ;
#16424 = AXIS2_PLACEMENT_3D ( 'NONE', #1678, #40647, #37434 ) ;
#16425 = CARTESIAN_POINT ( 'NONE',  ( 3.465721614298269415, 18.43485028915299750, -3.064284189100199729 ) ) ;
#16426 = CARTESIAN_POINT ( 'NONE',  ( -47.71508057896579658, 20.49549959222711593, -5.111566084959475731 ) ) ;
#16427 = CARTESIAN_POINT ( 'NONE',  ( 11.66725022231030984, 16.51000000000000156, -5.016499999999999737 ) ) ;
#16428 = CARTESIAN_POINT ( 'NONE',  ( 3.026662605148213725, -13.87242449132548217, 1.205013440933411228 ) ) ;
#16429 = CARTESIAN_POINT ( 'NONE',  ( 2.328636301501455286, 124.8000875644994068, 0.03907356579384867884 ) ) ;
#16430 = CARTESIAN_POINT ( 'NONE',  ( -21.01068656986065974, 132.3427885975763161, 0.3612206858233398821 ) ) ;
#16431 = ORIENTED_EDGE ( 'NONE', *, *, #25895, .T. ) ;
#16432 = CARTESIAN_POINT ( 'NONE',  ( 15.47023807670824525, 120.6682698389898576, 0.3091321738930620788 ) ) ;
#16433 = VERTEX_POINT ( 'NONE', #3078 ) ;
#16434 = CARTESIAN_POINT ( 'NONE',  ( -4.965295013367585497, 115.7029491485453576, 1.257100568209378988 ) ) ;
#16435 = CARTESIAN_POINT ( 'NONE',  ( 5.949011718796170634, -14.81501284647598915, 0.9937821824230966827 ) ) ;
#16436 = CARTESIAN_POINT ( 'NONE',  ( -12.82775609536344774, 122.1393999080170971, 1.276540306405074876 ) ) ;
#16437 = CARTESIAN_POINT ( 'NONE',  ( 1.113991634874381020, 117.6437429425539420, -0.5281592773360502813 ) ) ;
#16438 = CARTESIAN_POINT ( 'NONE',  ( -4.550674770548566173, 2.667180226961371137, -0.8080508602523945871 ) ) ;
#16439 = EDGE_CURVE ( 'NONE', #11659, #4497, #28623, .T. ) ;
#16440 = CARTESIAN_POINT ( 'NONE',  ( -58.67004091686991529, -0.3138842535942401590, -0.3180043108007239994 ) ) ;
#16441 = VERTEX_POINT ( 'NONE', #16037 ) ;
#16442 = CARTESIAN_POINT ( 'NONE',  ( -23.21760062652228385, 78.26400813401573942, 1.523999999999993360 ) ) ;
#16443 = CARTESIAN_POINT ( 'NONE',  ( 0.3557992751141359489, 119.2343925067223722, 0.8259638274389489165 ) ) ;
#16444 = DIRECTION ( 'NONE',  ( -0.0004113621476973288913, 0.9999999153568039922, -8.219994698375953989E-06 ) ) ;
#16445 = CARTESIAN_POINT ( 'NONE',  ( -10.67172107669508208, 123.8807653058400575, 0.9292482510779809246 ) ) ;
#16446 = CARTESIAN_POINT ( 'NONE',  ( 13.17422243436029916, 17.14500000000093394, -5.016499999999999737 ) ) ;
#16447 = CARTESIAN_POINT ( 'NONE',  ( 12.44264023681980902, 124.1810962131942517, -1.301390444852660755 ) ) ;
#16448 = CARTESIAN_POINT ( 'NONE',  ( -13.39049918543330975, 121.7711344121973411, -1.690880791723282428 ) ) ;
#16449 = CARTESIAN_POINT ( 'NONE',  ( -58.83227707057486811, -0.08366279997995551554, -0.2458995907045101459 ) ) ;
#16450 = VERTEX_POINT ( 'NONE', #15619 ) ;
#16451 = CARTESIAN_POINT ( 'NONE',  ( 4.552138684229567467, 118.1085559717327129, -0.4997336699443528651 ) ) ;
#16452 = EDGE_CURVE ( 'NONE', #41795, #34762, #30161, .T. ) ;
#16453 = CARTESIAN_POINT ( 'NONE',  ( 15.82779737147842880, 147.6293441119438512, -0.5318544519934516046 ) ) ;
#16454 = ORIENTED_EDGE ( 'NONE', *, *, #9224, .F. ) ;
#16455 = CARTESIAN_POINT ( 'NONE',  ( -14.65736332902334027, 131.2156652454908112, -2.020252246219832237 ) ) ;
#16456 = CARTESIAN_POINT ( 'NONE',  ( 3.794293369880153310, -15.39696243832143452, 2.404174946430260196 ) ) ;
#16457 = DIRECTION ( 'NONE',  ( -0.9998004120163609398, 0.000000000000000000, -0.01997839162482749689 ) ) ;
#16458 = CIRCLE ( 'NONE', #28044, 0.6349999999999998979 ) ;
#16459 = CARTESIAN_POINT ( 'NONE',  ( -42.12253153191133492, 21.94389511927448311, -6.431429377749453771E-15 ) ) ;
#16460 = CARTESIAN_POINT ( 'NONE',  ( -4.858599712106120627, 117.6759678160989040, 0.8825250931707183666 ) ) ;
#16461 = CARTESIAN_POINT ( 'NONE',  ( 5.258743330460715626, 156.4258374981641282, 1.697662213785431140 ) ) ;
#16462 = CARTESIAN_POINT ( 'NONE',  ( -2.937855498725889802, 30.67129419150591829, -0.3884002086831440104 ) ) ;
#16463 = CARTESIAN_POINT ( 'NONE',  ( -3.130497002865707312, 23.39511390029671745, 3.426874451367011520 ) ) ;
#16464 = CARTESIAN_POINT ( 'NONE',  ( 9.132214679254509804, 153.9061766533773152, 0.3822102345680644109 ) ) ;
#16465 = DIRECTION ( 'NONE',  ( -0.000000000000000000, -0.000000000000000000, -1.000000000000000000 ) ) ;
#16466 = ADVANCED_FACE ( 'NONE', ( #22208 ), #22820, .F. ) ;
#16467 = AXIS2_PLACEMENT_3D ( 'NONE', #38010, #40793, #11593 ) ;
#16468 = ADVANCED_FACE ( 'NONE', ( #3499 ), #29466, .T. ) ;
#16470 = ORIENTED_EDGE ( 'NONE', *, *, #20593, .T. ) ;
#16469 = CARTESIAN_POINT ( 'NONE',  ( -47.40532530373579334, 16.48158934372809270, -0.7854836779716005690 ) ) ;
#16471 = DIRECTION ( 'NONE',  ( -4.017660918040594346E-17, 1.000000000000000000, 2.376309959284834438E-19 ) ) ;
#16472 = DIRECTION ( 'NONE',  ( -5.188838149069471174E-16, 1.699382548006136313E-16, 1.000000000000000000 ) ) ;
#16473 = CARTESIAN_POINT ( 'NONE',  ( -23.09297118196009535, 77.93920196072180318, -1.524000000000005128 ) ) ;
#16474 = FACE_BOUND ( 'NONE', #36335, .T. ) ;
#16475 = CARTESIAN_POINT ( 'NONE',  ( -8.267082973024169945, 120.1495290627620847, -1.449466298147102483 ) ) ;
#16476 = EDGE_CURVE ( 'NONE', #17174, #15268, #29497, .T. ) ;
#16477 = CARTESIAN_POINT ( 'NONE',  ( -14.73199999999999754, 61.59499999999999886, -1.904999999999999583 ) ) ;
#16478 = CARTESIAN_POINT ( 'NONE',  ( -3.682264917456324227, 95.34346620154573770, -0.07358041635423923088 ) ) ;
#16479 = CARTESIAN_POINT ( 'NONE',  ( -56.17386367503594613, 7.314326147911789811, 0.9214986423944734328 ) ) ;
#16480 = CARTESIAN_POINT ( 'NONE',  ( -57.69570286664291103, 2.558035660193719529, 1.875687456014364152 ) ) ;
#16481 = CARTESIAN_POINT ( 'NONE',  ( -16.13169674176122115, 121.3783152868344075, -0.08747489889995958834 ) ) ;
#16482 = ORIENTED_EDGE ( 'NONE', *, *, #20903, .F. ) ;
#16483 = CARTESIAN_POINT ( 'NONE',  ( -54.68578128246380743, 13.03233524003756472, -0.2705950194913063767 ) ) ;
#16484 = CARTESIAN_POINT ( 'NONE',  ( -7.789231022850876762, 122.5917277006084447, -0.3009637317056043093 ) ) ;
#16485 = ORIENTED_EDGE ( 'NONE', *, *, #19413, .T. ) ;
#16486 = DIRECTION ( 'NONE',  ( 5.188838149069472160E-16, -1.699382548006136559E-16, -1.000000000000000000 ) ) ;
#16487 = CARTESIAN_POINT ( 'NONE',  ( -9.075584820321632051, 124.0722828908287454, -0.2154388746608566219 ) ) ;
#16488 = CARTESIAN_POINT ( 'NONE',  ( 6.168037961413951997, -13.40247527924742776, 1.492370457280242091 ) ) ;
#16489 = CARTESIAN_POINT ( 'NONE',  ( -0.02768730785358111679, 158.9256195073445213, 1.385586103196075891 ) ) ;
#16490 = CARTESIAN_POINT ( 'NONE',  ( -6.401666570281891566, 64.12941061790216679, -1.269999999999994023 ) ) ;
#16491 = VECTOR ( 'NONE', #24549, 1000.000000000000000 ) ;
#16492 = CARTESIAN_POINT ( 'NONE',  ( 15.30459713313458892, 120.6995131204970875, 0.6235550965980859450 ) ) ;
#16493 = DIRECTION ( 'NONE',  ( 1.000000000000000000, 0.000000000000000000, 0.000000000000000000 ) ) ;
#16494 = CARTESIAN_POINT ( 'NONE',  ( 4.831639344160726601, 118.5266822147775940, -0.7488923974486405566 ) ) ;
#16495 = CARTESIAN_POINT ( 'NONE',  ( -0.7366970693195243891, 2.667464547469879488, -0.6395729927624468347 ) ) ;
#16496 = CARTESIAN_POINT ( 'NONE',  ( -1.414297571701438105, 159.6040221172770259, -0.1149235736256734586 ) ) ;
#16497 = FACE_OUTER_BOUND ( 'NONE', #10824, .T. ) ;
#16498 = CARTESIAN_POINT ( 'NONE',  ( -23.69188486464780752, 78.08202335040543574, -1.270000000000005347 ) ) ;
#16499 = VERTEX_POINT ( 'NONE', #32880 ) ;
#16500 = CARTESIAN_POINT ( 'NONE',  ( 8.699452012065234996, 118.0993342392008714, 0.8513243511965803423 ) ) ;
#16501 = ORIENTED_EDGE ( 'NONE', *, *, #32307, .T. ) ;
#16502 = CARTESIAN_POINT ( 'NONE',  ( -18.41704236485563584, 146.8095856830544790, 1.664602135862215615 ) ) ;
#16503 = DIRECTION ( 'NONE',  ( 6.353134868986659519E-16, -1.000000000000000000, 0.000000000000000000 ) ) ;
#16504 = CARTESIAN_POINT ( 'NONE',  ( 10.62690833282000469, 119.8050749133877275, 1.415659332795228265 ) ) ;
#16505 = CARTESIAN_POINT ( 'NONE',  ( 20.10795522872006913, 148.3334041379468715, -1.700709099906817512 ) ) ;
#16506 = CARTESIAN_POINT ( 'NONE',  ( -0.09096679801628397566, 0.3556511065658448656, 0.9697834404811940257 ) ) ;
#16507 = CARTESIAN_POINT ( 'NONE',  ( -21.06903215802097051, 150.2702755442954583, -2.120733010085479986 ) ) ;
#16508 = CARTESIAN_POINT ( 'NONE',  ( 4.750401733383816882, 117.8973045592046986, -0.7610669662629643284 ) ) ;
#16509 = CARTESIAN_POINT ( 'NONE',  ( 5.608813212978028595, 117.9149360781225937, 0.7492264055198125661 ) ) ;
#16510 = VECTOR ( 'NONE', #5860, 1000.000000000000000 ) ;
#16511 = CARTESIAN_POINT ( 'NONE',  ( 10.28583081752390349, 123.7737839053064022, -0.8195368008302434948 ) ) ;
#16512 = CARTESIAN_POINT ( 'NONE',  ( -15.72486432277162649, 146.8976350983841144, -0.2628874744899974969 ) ) ;
#16513 = ORIENTED_EDGE ( 'NONE', *, *, #15211, .F. ) ;
#16514 = CARTESIAN_POINT ( 'NONE',  ( -0.4972808831008551644, 119.3183582894065893, -0.5800711753708561735 ) ) ;
#16515 = CARTESIAN_POINT ( 'NONE',  ( 3.432040476525267891, -15.74971700692714904, 4.939269227581224442 ) ) ;
#16516 = DIRECTION ( 'NONE',  ( 0.000000000000000000, 0.000000000000000000, -1.000000000000000000 ) ) ;
#16517 = CARTESIAN_POINT ( 'NONE',  ( -43.10982161678889213, 22.52422253607401359, -1.888110242252992066 ) ) ;
#16518 = ORIENTED_EDGE ( 'NONE', *, *, #40126, .F. ) ;
#16519 = CARTESIAN_POINT ( 'NONE',  ( 1.321503922127525765, 119.3298839580929638, 0.6528639922554047015 ) ) ;
#16520 = DIRECTION ( 'NONE',  ( 0.01997839162482749689, 1.040247600000945640E-18, -0.9998004120163610509 ) ) ;
#16521 = ADVANCED_FACE ( 'NONE', ( #723 ), #19319, .T. ) ;
#16522 = DIRECTION ( 'NONE',  ( 0.000000000000000000, 1.000000000000000000, 0.000000000000000000 ) ) ;
#16523 = AXIS2_PLACEMENT_3D ( 'NONE', #6814, #13622, #25976 ) ;
#16524 = CARTESIAN_POINT ( 'NONE',  ( -2.458941639547564506, 111.1666841684333633, 3.140650435616773706 ) ) ;
#16525 = CARTESIAN_POINT ( 'NONE',  ( 8.129739676946041271, 26.40327925692461619, 2.337594602388961107 ) ) ;
#16526 = CARTESIAN_POINT ( 'NONE',  ( 2.749413646642089759, 120.8469057251343060, 0.2833394764088550399 ) ) ;
#16527 = CARTESIAN_POINT ( 'NONE',  ( 16.42246607841793704, 155.2191194103077407, -0.6571739840263305377 ) ) ;
#16528 = CARTESIAN_POINT ( 'NONE',  ( 4.708802384804349650, 117.9017870880961851, 0.9536527796915015287 ) ) ;
#16529 = DIRECTION ( 'NONE',  ( -0.9998004120163610509, -4.016384292689131511E-17, -0.01997839162482749689 ) ) ;
#16530 = CIRCLE ( 'NONE', #15829, 5.080000000000006288 ) ;
#16531 = EDGE_CURVE ( 'NONE', #40888, #21156, #23782, .T. ) ;
#16532 = CARTESIAN_POINT ( 'NONE',  ( -3.715898061425088716, 116.6275173757784813, -0.03328880940299687452 ) ) ;
#16533 = EDGE_LOOP ( 'NONE', ( #14583, #8179, #28768, #31770 ) ) ;
#16534 = CARTESIAN_POINT ( 'NONE',  ( -7.937677187970164638, 121.7945880220786563, -1.052464246659149394 ) ) ;
#16535 = CARTESIAN_POINT ( 'NONE',  ( 5.611662049521669360, -14.50861037526213160, 3.104497901075802702 ) ) ;
#16536 = CARTESIAN_POINT ( 'NONE',  ( -5.232823448427346591, 121.2166884500396833, -0.3893023073710018545 ) ) ;
#16537 = CARTESIAN_POINT ( 'NONE',  ( 3.526842715273949214, -14.30601272375732513, 4.884018970202873788 ) ) ;
#16538 = ADVANCED_FACE ( 'NONE', ( #3233 ), #3443, .F. ) ;
#16539 = CARTESIAN_POINT ( 'NONE',  ( -13.85601021432062652, 120.6843904051541898, 0.7167389240433507114 ) ) ;
#16540 = CARTESIAN_POINT ( 'NONE',  ( 14.95453923199683111, 61.75387968257833649, 5.016499999999999737 ) ) ;
#16541 = CARTESIAN_POINT ( 'NONE',  ( 18.81533481972603283, 125.3161215262879580, 0.4318114027375014596 ) ) ;
#16542 = EDGE_LOOP ( 'NONE', ( #30605, #27265, #40094, #38708 ) ) ;
#16543 = CARTESIAN_POINT ( 'NONE',  ( 4.523211737919912601, 7.414965188139293950, 0.9565071382433593117 ) ) ;
#16544 = CARTESIAN_POINT ( 'NONE',  ( -4.434004255332462563, 105.1217594994107003, 2.985252168657458238 ) ) ;
#16545 = CARTESIAN_POINT ( 'NONE',  ( -14.95453923199683288, 61.75387968257833649, -5.016499999999999737 ) ) ;
#16546 = CARTESIAN_POINT ( 'NONE',  ( -1.925929944387235853E-31, 0.000000000000000000, 0.000000000000000000 ) ) ;
#16547 = CARTESIAN_POINT ( 'NONE',  ( 8.005068693524716394, 121.4516396534798162, 1.199299645920925972 ) ) ;
#16548 = CARTESIAN_POINT ( 'NONE',  ( -1.441504266290200897, 6.599927940091079748, -4.410093354674724964 ) ) ;
#16549 = CARTESIAN_POINT ( 'NONE',  ( 21.78097984573138390, 150.5404744109896171, 1.730106343981699268 ) ) ;
#16550 = CARTESIAN_POINT ( 'NONE',  ( -49.26674734213554530, 17.44270459986159594, -5.073646373245743746 ) ) ;
#16552 = CARTESIAN_POINT ( 'NONE',  ( 0.02874440110933674380, 158.8294072187990196, -1.438487372358303373 ) ) ;
#16551 = CARTESIAN_POINT ( 'NONE',  ( -3.682264917456323339, 71.97546620154574271, -0.07358041635423968885 ) ) ;
#16553 = VECTOR ( 'NONE', #36722, 1000.000000000000114 ) ;
#16554 = CARTESIAN_POINT ( 'NONE',  ( -0.5507456681092424144, 15.89564879194059799, -4.587442282481805300 ) ) ;
#16555 = CARTESIAN_POINT ( 'NONE',  ( -22.65971377182568602, 149.0844379882532849, -1.633711759839209243 ) ) ;
#16556 = ORIENTED_EDGE ( 'NONE', *, *, #12782, .T. ) ;
#16557 = VECTOR ( 'NONE', #28467, 1000.000000000000000 ) ;
#16558 = CARTESIAN_POINT ( 'NONE',  ( -2.954508604762049462, 156.0884104482065595, 0.2429312420959233720 ) ) ;
#16559 = CARTESIAN_POINT ( 'NONE',  ( 5.673832624563095450, -13.47712647082498272, 2.605829897212420754 ) ) ;
#16560 = CARTESIAN_POINT ( 'NONE',  ( -4.580899860306842264, 27.87760619330545708, 0.5121266511161914892 ) ) ;
#16561 = AXIS2_PLACEMENT_3D ( 'NONE', #30557, #33772, #4806 ) ;
#16562 = CARTESIAN_POINT ( 'NONE',  ( -0.1714850630699969736, 105.9761014636842731, -5.301312858626547886 ) ) ;
#16563 = ORIENTED_EDGE ( 'NONE', *, *, #33879, .T. ) ;
#16564 = CARTESIAN_POINT ( 'NONE',  ( 17.37713502592712445, 151.5007859583534753, 2.430116715062250687 ) ) ;
#16565 = DIRECTION ( 'NONE',  ( 1.011795553208986377E-16, 1.000000000000000000, -0.000000000000000000 ) ) ;
#16566 = CARTESIAN_POINT ( 'NONE',  ( -6.758592445694407663E-14, 130.0144662015457300, 5.650815781856659706E-18 ) ) ;
#16567 = CARTESIAN_POINT ( 'NONE',  ( -1.973526102370684487, 116.9869758084673208, 0.3704244399607084515 ) ) ;
#16568 = CARTESIAN_POINT ( 'NONE',  ( -5.424866478234207534, 26.46299946464603181, -6.465121161284864471 ) ) ;
#16569 = CARTESIAN_POINT ( 'NONE',  ( 16.92419414914112608, 122.6916909566506320, -0.1062714098145888658 ) ) ;
#16570 = CARTESIAN_POINT ( 'NONE',  ( -46.70910030332949248, 25.96830944048481982, 1.353001860315405924 ) ) ;
#16571 = CARTESIAN_POINT ( 'NONE',  ( -48.69154271504742582, 20.42972839736894386, 3.938715850604322721 ) ) ;
#16573 = ADVANCED_FACE ( 'NONE', ( #6015 ), #8140, .T. ) ;
#16572 = CARTESIAN_POINT ( 'NONE',  ( -4.962679952929507365, 117.4046820319011033, -1.029671477350346809 ) ) ;
#16574 = CARTESIAN_POINT ( 'NONE',  ( -51.34009458250667279, 14.66650723912346699, 4.800162786360129274 ) ) ;
#16575 = LINE ( 'NONE', #16144, #36184 ) ;
#16576 = CARTESIAN_POINT ( 'NONE',  ( -4.477012829077108513, 118.1289466633855199, 0.5423931779833521816 ) ) ;
#16577 = CARTESIAN_POINT ( 'NONE',  ( -17.14499999999999957, 71.11999999999999034, 5.016499999999999737 ) ) ;
#16578 = CIRCLE ( 'NONE', #31555, 3.175000000000001155 ) ;
#16579 = ORIENTED_EDGE ( 'NONE', *, *, #22521, .F. ) ;
#16580 = CARTESIAN_POINT ( 'NONE',  ( -0.06585476185879614308, 115.6909491485452435, -1.765419769167920094 ) ) ;
#16581 = EDGE_CURVE ( 'NONE', #11659, #28739, #38900, .T. ) ;
#16582 =( BOUNDED_CURVE ( )  B_SPLINE_CURVE ( 3, ( #25737, #35554, #29788, #26586 ),
 .UNSPECIFIED., .F., .T. ) 
 B_SPLINE_CURVE_WITH_KNOTS ( ( 4, 4 ),
 ( 3.141592653589792672, 4.712388980384688786 ),
 .UNSPECIFIED. ) 
 CURVE ( )  GEOMETRIC_REPRESENTATION_ITEM ( )  RATIONAL_B_SPLINE_CURVE ( ( 1.000000000000000000, 0.8047378541243650485, 0.8047378541243650485, 1.000000000000000000 ) ) 
 REPRESENTATION_ITEM ( '' )  );
#16583 = CARTESIAN_POINT ( 'NONE',  ( -8.291374016806893010, 120.0310598864996479, -1.449589630850732114 ) ) ;
#16584 = CARTESIAN_POINT ( 'NONE',  ( -4.994922087954134504, 114.3796182124986984, -1.954983995200229030 ) ) ;
#16585 = CARTESIAN_POINT ( 'NONE',  ( 4.502580129441241752, 118.1162376777982956, 0.7114035020871308790 ) ) ;
#16586 = CARTESIAN_POINT ( 'NONE',  ( -46.81070079724250377, 25.76746909427398435, -1.215830024444428892 ) ) ;
#16587 = CARTESIAN_POINT ( 'NONE',  ( -1.752245784495178649, 156.4219299504922844, -0.9069267871912082279 ) ) ;
#16588 = AXIS2_PLACEMENT_3D ( 'NONE', #20745, #13746, #769 ) ;
#16589 = CARTESIAN_POINT ( 'NONE',  ( -3.612350073381208393, 115.7029516324609233, -1.621358293364550063 ) ) ;
#16590 = CARTESIAN_POINT ( 'NONE',  ( 5.586884702347364673, 85.69146620154573668, 0.1116392523995368424 ) ) ;
#16591 = CARTESIAN_POINT ( 'NONE',  ( 5.946884660761559971, 118.9717589635377664, -0.3494607991981760753 ) ) ;
#16592 = CARTESIAN_POINT ( 'NONE',  ( -6.954653016369137575, 155.6889469082406947, -1.616181084571816085 ) ) ;
#16593 = CARTESIAN_POINT ( 'NONE',  ( -0.001367086239821354828, 156.3041635968983485, 0.06841458569046227067 ) ) ;
#16594 = CARTESIAN_POINT ( 'NONE',  ( 8.796322004575774400, 117.7098159678576366, -0.02677737093245648181 ) ) ;
#16595 = CARTESIAN_POINT ( 'NONE',  ( -15.72482850224671225, 145.6824189663691413, -0.1796683355943700655 ) ) ;
#16596 = CARTESIAN_POINT ( 'NONE',  ( -0.8472427164685307766, -8.777537934218566207, -4.544909406875613733 ) ) ;
#16597 = CARTESIAN_POINT ( 'NONE',  ( 9.660431270553193173, 118.1749183431956425, 0.7024802509354081126 ) ) ;
#16598 = CARTESIAN_POINT ( 'NONE',  ( 1.332716859069107315E-15, 13.84300000000000352, 0.000000000000000000 ) ) ;
#16599 = CARTESIAN_POINT ( 'NONE',  ( 3.141231902390079878, -14.40076222614043644, 1.273921468989656969 ) ) ;
#16600 = CIRCLE ( 'NONE', #1666, 0.7620000000000015650 ) ;
#16601 = CARTESIAN_POINT ( 'NONE',  ( -5.055620027408552986, 119.3892302351119810, 0.8859254200104713650 ) ) ;
#16602 = CARTESIAN_POINT ( 'NONE',  ( 0.1234711523483410095, 5.102374915558315571, -0.9659065422363407594 ) ) ;
#16603 = CARTESIAN_POINT ( 'NONE',  ( -23.20005416489669869, 148.7951734159264561, -1.060305963766562831 ) ) ;
#16604 = CARTESIAN_POINT ( 'NONE',  ( -0.3677562164248854293, -4.027846162062824753, 0.9036657059391408620 ) ) ;
#16605 = ORIENTED_EDGE ( 'NONE', *, *, #18079, .F. ) ;
#16606 = ORIENTED_EDGE ( 'NONE', *, *, #20652, .T. ) ;
#16607 = CARTESIAN_POINT ( 'NONE',  ( -46.25688858429104044, 20.73875112231585760, 4.700046123029338219 ) ) ;
#16608 = CARTESIAN_POINT ( 'NONE',  ( 4.979866836074831937, 117.8491495069952748, 0.7948704875671747105 ) ) ;
#16609 = DIRECTION ( 'NONE',  ( 0.000000000000000000, 0.000000000000000000, 1.000000000000000000 ) ) ;
#16610 = CARTESIAN_POINT ( 'NONE',  ( -16.19917940306807935, 146.4165046419237228, 0.6472847106673342843 ) ) ;
#16611 = CARTESIAN_POINT ( 'NONE',  ( 3.761132227337853351, -14.12294213130394027, 4.617837385609514733 ) ) ;
#16612 = CARTESIAN_POINT ( 'NONE',  ( 5.322365003948895890, 156.4258374981641282, -1.486226487625613712 ) ) ;
#16613 = CIRCLE ( 'NONE', #27509, 3.175000000000001155 ) ;
#16614 = CARTESIAN_POINT ( 'NONE',  ( -10.99314024304357673, 156.0189320485970086, -2.156370349642058759 ) ) ;
#16615 = DIRECTION ( 'NONE',  ( -0.8745520943968235761, 0.4849315768086558398, -5.691349986800547879E-16 ) ) ;
#16616 = CARTESIAN_POINT ( 'NONE',  ( 3.216637634036228821, -14.25892527173770752, 2.941440830758975888 ) ) ;
#16617 = CARTESIAN_POINT ( 'NONE',  ( -4.975175664203050907, 32.06598106186588382, 0.7459204072935272656 ) ) ;
#16618 = CARTESIAN_POINT ( 'NONE',  ( 2.930943089244447464, 156.0861408873597327, -0.1605890987591809260 ) ) ;
#16619 = ORIENTED_EDGE ( 'NONE', *, *, #33957, .T. ) ;
#16620 = DIRECTION ( 'NONE',  ( 0.8745520943968236871, -0.4849315768086559508, 6.829619984160659032E-16 ) ) ;
#16621 = DIRECTION ( 'NONE',  ( 0.000000000000000000, 0.000000000000000000, 1.000000000000000000 ) ) ;
#16622 = DIRECTION ( 'NONE',  ( 0.000000000000000000, 1.000000000000000000, 0.000000000000000000 ) ) ;
#16623 = DIRECTION ( 'NONE',  ( -0.4849315768086535083, -0.8745520943968250194, -1.030032898892974695E-16 ) ) ;
#16624 = CARTESIAN_POINT ( 'NONE',  ( 23.43370484584237445, 146.8275480241000253, 0.3132885061830184004 ) ) ;
#16625 = CARTESIAN_POINT ( 'NONE',  ( -5.634266555046488989, 117.9149360781225937, 0.5245629147119165170 ) ) ;
#16626 = CARTESIAN_POINT ( 'NONE',  ( -2.051901798287135037, 115.6909491485452577, 1.638078500307909247 ) ) ;
#16627 = LINE ( 'NONE', #17049, #41937 ) ;
#16628 = CARTESIAN_POINT ( 'NONE',  ( 1.020007333917743342, 39.20946620154573026, -1.249871353326013068 ) ) ;
#16629 = EDGE_CURVE ( 'NONE', #7830, #22451, #23672, .T. ) ;
#16630 = CARTESIAN_POINT ( 'NONE',  ( -0.01051220311291895665, 117.9844940561907265, 0.5260736299896251467 ) ) ;
#16631 = CARTESIAN_POINT ( 'NONE',  ( -4.024516124431025688, 26.91537645720152128, -2.298571904627217499 ) ) ;
#16632 = CARTESIAN_POINT ( 'NONE',  ( 5.644239659282993316, 25.55377913558855596, 6.252972086369320337 ) ) ;
#16633 = CARTESIAN_POINT ( 'NONE',  ( -2.163080554094883645, 116.7372139585571915, -0.4936440420418066743 ) ) ;
#16634 = CARTESIAN_POINT ( 'NONE',  ( -0.6121664022497388391, 114.3327162918516962, -2.181662845130500461 ) ) ;
#16635 = DIRECTION ( 'NONE',  ( -0.000000000000000000, -0.000000000000000000, -1.000000000000000000 ) ) ;
#16636 = CARTESIAN_POINT ( 'NONE',  ( 3.603687985131259541, 104.6144662015326077, 3.947868320610233628 ) ) ;
#16637 = CARTESIAN_POINT ( 'NONE',  ( -3.789191232057584902, 13.46218022696137773, 2.646434746401360893 ) ) ;
#16638 = FACE_OUTER_BOUND ( 'NONE', #12349, .T. ) ;
#16639 = CARTESIAN_POINT ( 'NONE',  ( -0.3704417442436215291, 117.3993836136686326, -1.500862690023503587 ) ) ;
#16640 = CARTESIAN_POINT ( 'NONE',  ( 3.114041961411902371, -14.44963006906317737, 3.768961988127400353 ) ) ;
#16641 = CARTESIAN_POINT ( 'NONE',  ( 0.1065646865914870872, 105.8844662015456777, -5.332932678536313809 ) ) ;
#16642 = CARTESIAN_POINT ( 'NONE',  ( -0.9959262657077846415, 116.9078805053781025, 0.3180477371503355744 ) ) ;
#16643 = CARTESIAN_POINT ( 'NONE',  ( 5.008579095102096979, 117.3966161975143052, -0.7759206776167619779 ) ) ;
#16644 = ORIENTED_EDGE ( 'NONE', *, *, #31107, .T. ) ;
#16645 = CARTESIAN_POINT ( 'NONE',  ( 5.586884702347364673, 98.39146620154573952, 0.1116392523995368424 ) ) ;
#16646 = VERTEX_POINT ( 'NONE', #6840 ) ;
#16647 = CARTESIAN_POINT ( 'NONE',  ( 3.009276887026297587, 39.20946620154573736, -1.210121013456480599 ) ) ;
#16648 = CARTESIAN_POINT ( 'NONE',  ( 3.172349117095228710, -15.63690262102951323, 5.390679387232247599 ) ) ;
#16649 = CARTESIAN_POINT ( 'NONE',  ( -19.78762832257856275, 149.1964539096042870, 1.700649111281397952 ) ) ;
#16650 = CARTESIAN_POINT ( 'NONE',  ( 13.99438190394152493, 121.2764344996515717, -0.9244547817413870661 ) ) ;
#16651 = CARTESIAN_POINT ( 'NONE',  ( 0.4398701176286285985, 29.43434963188315834, -0.8729469796826672123 ) ) ;
#16652 = CARTESIAN_POINT ( 'NONE',  ( -58.82993483412206359, -0.2576888758964282489, -0.02106341969870843475 ) ) ;
#16653 = ORIENTED_EDGE ( 'NONE', *, *, #26678, .T. ) ;
#16654 = DIRECTION ( 'NONE',  ( 0.9998004120163608288, 0.000000000000000000, 0.01997839162482749342 ) ) ;
#16655 = CARTESIAN_POINT ( 'NONE',  ( 0.9036232957555455636, 122.5862318000603182, 0.2430700419085215502 ) ) ;
#16656 = PRESENTATION_STYLE_ASSIGNMENT (( #6878 ) ) ;
#16657 = CARTESIAN_POINT ( 'NONE',  ( -2.594326071755724605, 120.1437993944865354, 0.4899928688880349492 ) ) ;
#16658 = CARTESIAN_POINT ( 'NONE',  ( -46.98357734554679155, 20.33138817508191210, 5.073745976080627607 ) ) ;
#16659 = CARTESIAN_POINT ( 'NONE',  ( 5.875153347143252880, 119.9178398404649926, -0.8959128733076280326 ) ) ;
#16660 = CARTESIAN_POINT ( 'NONE',  ( -17.27141581160028494, 128.5728276651957742, -2.069917288257624222 ) ) ;
#16661 = CARTESIAN_POINT ( 'NONE',  ( -58.37934292759150168, 0.9822739792931106662, -1.208960021102219340 ) ) ;
#16662 = ORIENTED_EDGE ( 'NONE', *, *, #7382, .F. ) ;
#16663 = CARTESIAN_POINT ( 'NONE',  ( 4.366462884195458471, 118.1827284966912686, -0.4455170831428560407 ) ) ;
#16664 = CARTESIAN_POINT ( 'NONE',  ( 12.13795026801524024, 151.9817061558079274, -0.5567646394148115796 ) ) ;
#16665 = ORIENTED_EDGE ( 'NONE', *, *, #19339, .T. ) ;
#16666 = CARTESIAN_POINT ( 'NONE',  ( -11.83432680469874221, 124.3826620800890339, -1.661842703385269626 ) ) ;
#16667 = CARTESIAN_POINT ( 'NONE',  ( 1.824651611884654967, -15.33505462125983598, 5.392305443003406751 ) ) ;
#16668 = EDGE_CURVE ( 'NONE', #37437, #37954, #28038, .T. ) ;
#16669 = CARTESIAN_POINT ( 'NONE',  ( 4.433447712847764066, 105.1217203547995069, -2.986091683647443595 ) ) ;
#16670 = CARTESIAN_POINT ( 'NONE',  ( -54.09072575248404036, 8.649776409421397361, 3.422340198163080327 ) ) ;
#16671 = AXIS2_PLACEMENT_3D ( 'NONE', #5920, #16471, #25282 ) ;
#16672 = CARTESIAN_POINT ( 'NONE',  ( -0.5832499861179958334, 10.72304255322087307, 4.598074068532726599 ) ) ;
#16673 = CARTESIAN_POINT ( 'NONE',  ( 10.71484998910085551, 123.2317624570580534, 1.496280440855932037 ) ) ;
#16674 = CARTESIAN_POINT ( 'NONE',  ( 1.398455114368189145, 34.89464803915915780, 0.3944493173928063090 ) ) ;
#16675 = EDGE_CURVE ( 'NONE', #10681, #20793, #25947, .T. ) ;
#16676 = CARTESIAN_POINT ( 'NONE',  ( -2.923568588381722844, 13.88697512809157786, 3.594856661414283394 ) ) ;
#16677 = CARTESIAN_POINT ( 'NONE',  ( 4.248167858406068476, 155.8413357349917021, 0.2489887396171408807 ) ) ;
#16678 = CARTESIAN_POINT ( 'NONE',  ( -46.38316532014830784, 26.05065462784526176, -1.524000000000014676 ) ) ;
#16679 = CARTESIAN_POINT ( 'NONE',  ( -55.00324375927522169, 6.200002331679180578, -1.420877854375708127 ) ) ;
#16680 = CARTESIAN_POINT ( 'NONE',  ( 6.758480964575337424, 78.81581826900307419, 3.179117336685197248 ) ) ;
#16681 = CARTESIAN_POINT ( 'NONE',  ( -0.2298130577371723104, 117.3993836757663729, 1.488868159487601872 ) ) ;
#16682 = CARTESIAN_POINT ( 'NONE',  ( 11.58677707360137710, 55.24500000000000455, -4.474811398758258285 ) ) ;
#16683 = CARTESIAN_POINT ( 'NONE',  ( -6.513165593194060347E-14, 68.92746620154572668, -8.865348866426607246E-18 ) ) ;
#16684 = CARTESIAN_POINT ( 'NONE',  ( -32.35167636075468778, 51.35580826818691236, -1.524000000000005128 ) ) ;
#16685 = FACE_OUTER_BOUND ( 'NONE', #6319, .T. ) ;
#16686 = CARTESIAN_POINT ( 'NONE',  ( -17.09698261757901960, 84.43312239790384410, -1.270000000000002904 ) ) ;
#16687 = CARTESIAN_POINT ( 'NONE',  ( -56.13924587166188473, 7.155854391526911051, 1.290439134121102782 ) ) ;
#16688 = CARTESIAN_POINT ( 'NONE',  ( -58.10099831372669854, 0.3475205698689753930, 0.9728495803591148405 ) ) ;
#16689 = EDGE_CURVE ( 'NONE', #13136, #19376, #7618, .T. ) ;
#16690 = CARTESIAN_POINT ( 'NONE',  ( -4.758755041967009269, 116.8068435238802465, 0.07043225793504331866 ) ) ;
#16691 = EDGE_LOOP ( 'NONE', ( #24933, #9504, #5783, #27825 ) ) ;
#16692 = CARTESIAN_POINT ( 'NONE',  ( -54.56940519185135230, 9.666406039105165604, -3.302709833357616365 ) ) ;
#16693 = CARTESIAN_POINT ( 'NONE',  ( 6.072382902230390123, 121.4395914931731113, 0.1186111012826013000 ) ) ;
#16694 = EDGE_LOOP ( 'NONE', ( #32638, #1834, #35385 ) ) ;
#16695 = CYLINDRICAL_SURFACE ( 'NONE', #7670, 9.048749999999998295 ) ;
#16696 = CARTESIAN_POINT ( 'NONE',  ( -2.896036792256268644, 156.0891579660883508, -0.1428477814196378037 ) ) ;
#16697 = CARTESIAN_POINT ( 'NONE',  ( 5.507117158935161072, -13.70471586423162336, 3.054220594615255191 ) ) ;
#16698 = CARTESIAN_POINT ( 'NONE',  ( -20.03018601867076853, 150.7967616730061593, 1.468133569223299961 ) ) ;
#16699 = CARTESIAN_POINT ( 'NONE',  ( -2.755274729907521980, 20.69627551736597226, -3.746277899328600558 ) ) ;
#16700 = CARTESIAN_POINT ( 'NONE',  ( 3.781797959329852521, 116.7736770086926867, 0.3417761088697102712 ) ) ;
#16701 = CARTESIAN_POINT ( 'NONE',  ( 15.25989735510956002, 148.0267574095444445, 0.5045397742221703341 ) ) ;
#16702 = CARTESIAN_POINT ( 'NONE',  ( -3.685501180670149424, 30.72893705507438611, -2.802369389919810772 ) ) ;
#16703 = CARTESIAN_POINT ( 'NONE',  ( -0.2306771026100957467, -3.802149480603859377, 0.9475509996518236555 ) ) ;
#16704 = CARTESIAN_POINT ( 'NONE',  ( -23.37772998923903600, 142.7868430859564626, -0.6200176421473858612 ) ) ;
#16705 = CARTESIAN_POINT ( 'NONE',  ( 5.241362157049057835, 57.14999999999999858, -5.310945289804168468 ) ) ;
#16706 = DIRECTION ( 'NONE',  ( -0.5810519254489896479, 0.8138664877804110409, 0.000000000000000000 ) ) ;
#16707 = ORIENTED_EDGE ( 'NONE', *, *, #31345, .F. ) ;
#16708 = CIRCLE ( 'NONE', #10596, 0.5080000000000014504 ) ;
#16709 = CARTESIAN_POINT ( 'NONE',  ( 8.725096631921111623, 117.9837440635962054, 0.7541645143275405028 ) ) ;
#16710 = EDGE_LOOP ( 'NONE', ( #38234, #22704, #32660, #6357 ) ) ;
#16711 = CARTESIAN_POINT ( 'NONE',  ( -17.58824906652093745, 148.8653046532945723, 1.619734885946522596 ) ) ;
#16712 = CARTESIAN_POINT ( 'NONE',  ( -57.83236317642370494, 0.8674604446124462021, -1.063638734186429291 ) ) ;
#16713 = CARTESIAN_POINT ( 'NONE',  ( 9.094277710717253882, 119.2843051134756536, 1.347562189204172034 ) ) ;
#16714 = CARTESIAN_POINT ( 'NONE',  ( 2.330377461923264004, 118.7486697826011977, -0.7097125967482103004 ) ) ;
#16715 = CARTESIAN_POINT ( 'NONE',  ( -0.3571511390000196573, -0.07365323586406080647, 0.9071407500242820721 ) ) ;
#16716 = CARTESIAN_POINT ( 'NONE',  ( -6.827620370266043182, 118.1252062928739832, -1.028125137227138275 ) ) ;
#16717 = CARTESIAN_POINT ( 'NONE',  ( 4.578866339686846310, 118.0740741925940256, -0.5988308625876450630 ) ) ;
#16718 = DIRECTION ( 'NONE',  ( 0.9998004120163610509, 4.016384292689131511E-17, 0.01997839162482749689 ) ) ;
#16719 = EDGE_CURVE ( 'NONE', #21134, #11121, #3981, .T. ) ;
#16720 = CARTESIAN_POINT ( 'NONE',  ( 10.20798870728732410, 124.0743415861677903, -0.7134647857254746706 ) ) ;
#16721 = CARTESIAN_POINT ( 'NONE',  ( -8.054407255016492684, 122.8529229587361442, -0.1293742239074501532 ) ) ;
#16722 = ORIENTED_EDGE ( 'NONE', *, *, #40219, .T. ) ;
#16723 = CARTESIAN_POINT ( 'NONE',  ( -4.224706347173693644, 119.5670751559891585, -0.9504096833562338809 ) ) ;
#16724 = CARTESIAN_POINT ( 'NONE',  ( 5.328887433758706216, -15.24262819705347916, -0.4233796293290443269 ) ) ;
#16725 = DIRECTION ( 'NONE',  ( 0.9998004120163608288, 0.000000000000000000, 0.01997839162482749342 ) ) ;
#16726 = CARTESIAN_POINT ( 'NONE',  ( -4.624492705069667586, 117.9598748055318822, -0.9307939849546735811 ) ) ;
#16727 = EDGE_CURVE ( 'NONE', #11005, #40169, #30045, .T. ) ;
#16728 = CARTESIAN_POINT ( 'NONE',  ( -42.33919149967392315, 22.05006338260229271, -1.842566675324098568 ) ) ;
#16729 = CARTESIAN_POINT ( 'NONE',  ( 4.144720667518057233, 118.2390924077483589, 0.4001709429842503218 ) ) ;
#16730 = B_SPLINE_SURFACE_WITH_KNOTS ( 'NONE', 3, 3, ( 
 ( #25539, #23156, #19981, #31873, #6791, #32144 ),
 ( #12957, #32349, #2976, #25950, #15730, #15939 ),
 ( #35557, #16572, #6373, #39167, #35764, #9974 ),
 ( #22947, #28735, #32780, #8624, #8201, #630 ) ),
 .UNSPECIFIED., .F., .F., .F.,
 ( 4, 4 ),
 ( 4, 2, 4 ),
 ( 0.000000000000000000, 1.000000000000000000 ),
 ( 0.000000000000000000, 0.5000000000000000000, 1.000000000000000000 ),
 .UNSPECIFIED. ) ;
#16731 = CARTESIAN_POINT ( 'NONE',  ( 18.01525633490669520, 148.5173242358814321, 2.382443637188214502 ) ) ;
#16732 = DIRECTION ( 'NONE',  ( -5.188838149069472160E-16, 1.699382548006136559E-16, 1.000000000000000000 ) ) ;
#16733 = CARTESIAN_POINT ( 'NONE',  ( 20.51686376604209983, 129.1072961674477710, 0.4099757654675941221 ) ) ;
#16734 = CARTESIAN_POINT ( 'NONE',  ( -4.107119205180256749, 117.8719421043398370, 0.6926522829710091145 ) ) ;
#16735 = CARTESIAN_POINT ( 'NONE',  ( 8.391066749008803782, -15.30525627429770097, -0.4359234444501501327 ) ) ;
#16736 = CARTESIAN_POINT ( 'NONE',  ( 8.816380758798560535, 123.2701452714374568, 0.6637701367642926398 ) ) ;
#16737 = AXIS2_PLACEMENT_3D ( 'NONE', #15132, #2388, #34969 ) ;
#16738 = CARTESIAN_POINT ( 'NONE',  ( 0.3479910049260485638, 116.9201722098172382, -0.3032510685202791101 ) ) ;
#16739 = FACE_OUTER_BOUND ( 'NONE', #21098, .T. ) ;
#16740 = EDGE_LOOP ( 'NONE', ( #34894, #35185, #33492, #27714 ) ) ;
#16741 = CARTESIAN_POINT ( 'NONE',  ( -58.36969448265841720, -0.2913820931539540249, 0.003449905599825503141 ) ) ;
#16742 = EDGE_CURVE ( 'NONE', #37219, #42027, #31404, .T. ) ;
#16743 = CARTESIAN_POINT ( 'NONE',  ( -8.217147260422519750, 117.5004391570743394, -0.1493243188240318264 ) ) ;
#16744 = ORIENTED_EDGE ( 'NONE', *, *, #4875, .F. ) ;
#16745 = CARTESIAN_POINT ( 'NONE',  ( -8.061441164751348865, 121.1678581073247614, -1.290394762592997679 ) ) ;
#16746 = DIRECTION ( 'NONE',  ( -5.188838149069472160E-16, 1.699382548006136559E-16, 1.000000000000000000 ) ) ;
#16747 = CARTESIAN_POINT ( 'NONE',  ( -9.229671467331892032, 123.9961275534082148, -0.5040434471971627639 ) ) ;
#16748 = CARTESIAN_POINT ( 'NONE',  ( 3.649535173467634674, -14.21384370944696407, 4.751373335446510637 ) ) ;
#16749 = CARTESIAN_POINT ( 'NONE',  ( -18.94714202558217764, 128.6554162386474047, 0.8647899522199680167 ) ) ;
#16750 = CARTESIAN_POINT ( 'NONE',  ( -6.266702236064261911, 78.85741254032745928, -4.063604302808976776 ) ) ;
#16751 = CARTESIAN_POINT ( 'NONE',  ( 16.85465591277202080, 155.2173118157008673, 0.4068649486066870935 ) ) ;
#16752 = VERTEX_POINT ( 'NONE', #13856 ) ;
#16753 = CARTESIAN_POINT ( 'NONE',  ( 4.560200836559435977, -11.68919918208664122, 0.6963878748952898601 ) ) ;
#16754 = CARTESIAN_POINT ( 'NONE',  ( -2.432703290510899841, 105.1243935390225204, 4.756760888922076269 ) ) ;
#16755 = DIRECTION ( 'NONE',  ( 5.188838149069472160E-16, -1.699382548006136559E-16, -1.000000000000000000 ) ) ;
#16756 = DIRECTION ( 'NONE',  ( -0.8745520943968241312, 0.4849315768086548961, -5.424246918827962036E-16 ) ) ;
#16757 = CARTESIAN_POINT ( 'NONE',  ( -8.197999847188267353, 120.7315320437793531, 1.065923837117515260 ) ) ;
#16758 = ADVANCED_FACE ( 'NONE', ( #467 ), #18463, .T. ) ;
#16759 = CARTESIAN_POINT ( 'NONE',  ( 4.506137822554599381, 3.376467715207942533, 1.027655576270160243 ) ) ;
#16760 = CARTESIAN_POINT ( 'NONE',  ( 14.51227343941606485, 121.4416029531759591, 1.418621967605989909 ) ) ;
#16761 = CARTESIAN_POINT ( 'NONE',  ( 15.72550100231830150, 145.6881679641598453, 0.3142329346387512934 ) ) ;
#16763 = CARTESIAN_POINT ( 'NONE',  ( 18.41670328667946421, 131.7683309214445728, -1.453117541724253448 ) ) ;
#16762 = CARTESIAN_POINT ( 'NONE',  ( -4.466782427718574588, 71.06098887363195615, 1.524000000000005128 ) ) ;
#16764 = CARTESIAN_POINT ( 'NONE',  ( -2.734508853367146219, 0.3528594962865297391, 3.724956791467788353 ) ) ;
#16765 = CARTESIAN_POINT ( 'NONE',  ( -22.33788829447793489, 150.2360280492587776, -1.519312068210846078 ) ) ;
#16766 = VERTEX_POINT ( 'NONE', #36659 ) ;
#16767 = CARTESIAN_POINT ( 'NONE',  ( -7.869802931810743196, 122.7053923345238502, -0.1572573916676445194 ) ) ;
#16768 = ORIENTED_EDGE ( 'NONE', *, *, #7082, .F. ) ;
#16769 = VECTOR ( 'NONE', #38956, 1000.000000000000000 ) ;
#16770 = CARTESIAN_POINT ( 'NONE',  ( -12.13843755257585144, 130.5412724693565849, 0.1686832038582291304 ) ) ;
#16771 = EDGE_CURVE ( 'NONE', #37389, #32811, #11601, .T. ) ;
#16772 = CARTESIAN_POINT ( 'NONE',  ( 5.747688368404943127, -13.35872296688338245, 2.372087187842143674 ) ) ;
#16773 = LINE ( 'NONE', #23141, #13158 ) ;
#16774 = EDGE_CURVE ( 'NONE', #31966, #6546, #36107, .T. ) ;
#16775 = CARTESIAN_POINT ( 'NONE',  ( -0.9968812942979460301, 106.0882118856391259, -5.244929698535035989 ) ) ;
#16776 = EDGE_LOOP ( 'NONE', ( #24047, #1707, #15641, #23296 ) ) ;
#16777 = CARTESIAN_POINT ( 'NONE',  ( 4.990993783036389964, 119.0545008048120366, 1.104648745759416295 ) ) ;
#16778 = CARTESIAN_POINT ( 'NONE',  ( -14.50851225146815437, 78.09971119798315442, 1.904999999999988258 ) ) ;
#16779 = DIRECTION ( 'NONE',  ( 5.188838149069472160E-16, -1.699382548006136559E-16, -1.000000000000000000 ) ) ;
#16780 = VECTOR ( 'NONE', #11117, 1000.000000000000000 ) ;
#16781 = CARTESIAN_POINT ( 'NONE',  ( -14.74755344529033962, 121.0688405154646858, 0.6244351273456011375 ) ) ;
#16782 = CARTESIAN_POINT ( 'NONE',  ( -5.272568914482754998, 19.56627864152888208, 6.568537450970175939 ) ) ;
#16783 = CARTESIAN_POINT ( 'NONE',  ( 12.30032609686865186, 128.4316967252784991, 1.345898664372764175 ) ) ;
#16784 = EDGE_CURVE ( 'NONE', #1073, #38342, #36028, .T. ) ;
#16785 = CARTESIAN_POINT ( 'NONE',  ( 23.20995092461732057, 148.9919839608952827, -0.1323997120335723976 ) ) ;
#16786 = CARTESIAN_POINT ( 'NONE',  ( -5.511339492711898380, 56.51500000000000767, -5.111277471823950869 ) ) ;
#16787 = VECTOR ( 'NONE', #8879, 1000.000000000000000 ) ;
#16788 = CARTESIAN_POINT ( 'NONE',  ( -46.68753544603657701, 26.01473869131327277, 1.331541039591896070 ) ) ;
#16789 = CARTESIAN_POINT ( 'NONE',  ( -47.17284909187768704, 24.49633334977720978, 1.858123130129375244 ) ) ;
#16790 = DIRECTION ( 'NONE',  ( -0.8745520943968250194, 0.4849315768086532863, -5.361993529360574930E-16 ) ) ;
#16791 = CARTESIAN_POINT ( 'NONE',  ( -48.98489377192316852, 18.65252824715059177, 5.272350768541908650 ) ) ;
#16792 = CARTESIAN_POINT ( 'NONE',  ( -58.67922015684681014, -0.3140008337426106744, 0.3102499017298660511 ) ) ;
#16793 = CARTESIAN_POINT ( 'NONE',  ( -4.552334805148916530, 118.1085767403579467, 0.4996156392678010594 ) ) ;
#16794 = CARTESIAN_POINT ( 'NONE',  ( -12.21488373879589240, 55.24499999999999034, -4.381499999999999950 ) ) ;
#16795 = AXIS2_PLACEMENT_3D ( 'NONE', #12195, #34781, #31362 ) ;
#16796 = ORIENTED_EDGE ( 'NONE', *, *, #10866, .F. ) ;
#16797 = CARTESIAN_POINT ( 'NONE',  ( -43.93316818929329770, 24.49458088220322338, 1.523999999999992916 ) ) ;
#16798 = CARTESIAN_POINT ( 'NONE',  ( 3.813032422245561825, 118.9366574157493943, -0.7812632686729226172 ) ) ;
#16799 = CARTESIAN_POINT ( 'NONE',  ( -3.406460098309205264, 108.6786390861269922, -4.123178694279357792 ) ) ;
#16800 = CARTESIAN_POINT ( 'NONE',  ( 4.546980637774593603, 118.0358567185017762, 0.8570574294820361150 ) ) ;
#16801 = CARTESIAN_POINT ( 'NONE',  ( -12.64766777886155857, 130.7634385742845780, -1.140803344710751288 ) ) ;
#16802 = CARTESIAN_POINT ( 'NONE',  ( -10.57002714855771863, 82.40335727708655611, 1.269999999999999796 ) ) ;
#16803 = CARTESIAN_POINT ( 'NONE',  ( 0.8540871238041118918, 117.3993835805474362, -1.452928456153284698 ) ) ;
#16804 = CARTESIAN_POINT ( 'NONE',  ( 5.516342712684529026, 117.4962825466697467, -0.6091453463174707483 ) ) ;
#16805 = EDGE_CURVE ( 'NONE', #10192, #20421, #17022, .T. ) ;
#16806 = CARTESIAN_POINT ( 'NONE',  ( -1.917342111448811393, 156.7095495334699535, -1.310369884728256995 ) ) ;
#16807 = CARTESIAN_POINT ( 'NONE',  ( 5.329288917532060132, 116.0444662015457453, 0.2890495193807575691 ) ) ;
#16808 = CARTESIAN_POINT ( 'NONE',  ( -19.68500000000000227, 71.11999999999999034, 5.714999999999998970 ) ) ;
#16809 = CARTESIAN_POINT ( 'NONE',  ( 7.991391493690734649, 121.7106681566311579, -0.7744224044265761719 ) ) ;
#16810 = CARTESIAN_POINT ( 'NONE',  ( -8.711945433812360307, 123.6715832479121673, -0.08701538749149796692 ) ) ;
#16811 = CARTESIAN_POINT ( 'NONE',  ( -0.5496829067194369811, 0.7180641350488168317, -4.598301960397928489 ) ) ;
#16812 = CARTESIAN_POINT ( 'NONE',  ( -0.01133159106151370929, 159.5297144918048673, 0.5670791535570577357 ) ) ;
#16813 = FACE_OUTER_BOUND ( 'NONE', #30861, .T. ) ;
#16814 = CARTESIAN_POINT ( 'NONE',  ( 3.190981477959303980, -15.14443901668413517, 3.594454035019850835 ) ) ;
#16815 = CARTESIAN_POINT ( 'NONE',  ( -16.91343413265456874, 151.2926467857828072, 1.744909534579184518 ) ) ;
#16816 = CARTESIAN_POINT ( 'NONE',  ( -0.1559983344249278314, 9.848737885527594216, 0.9609112391775298523 ) ) ;
#16817 = CARTESIAN_POINT ( 'NONE',  ( -3.798364743159273083, 116.8316721669309572, -0.3950458664356921168 ) ) ;
#16818 = CIRCLE ( 'NONE', #27008, 3.175000000000001155 ) ;
#16819 = CARTESIAN_POINT ( 'NONE',  ( -0.3022039251088723399, 24.96921649940425425, -0.9259629999792299282 ) ) ;
#16820 = ORIENTED_EDGE ( 'NONE', *, *, #34009, .F. ) ;
#16821 = CARTESIAN_POINT ( 'NONE',  ( -47.30388380253317138, 17.78501317193704168, 2.251402236601635742 ) ) ;
#16822 = CARTESIAN_POINT ( 'NONE',  ( 6.667064533335116394, 121.2389289720308199, 0.3413157713140476113 ) ) ;
#16823 = CARTESIAN_POINT ( 'NONE',  ( -6.293976855803995463, 155.3815620563194955, 0.6499927463934688232 ) ) ;
#16824 = CARTESIAN_POINT ( 'NONE',  ( 4.181132250215417123, -13.15738584483822038, 3.071181452022354819 ) ) ;
#16825 = CARTESIAN_POINT ( 'NONE',  ( 17.54876304910989049, 147.2926247242496345, -1.462364720961515818 ) ) ;
#16826 = CARTESIAN_POINT ( 'NONE',  ( -17.10357040864165512, 151.3967157021085654, -2.430234537686703611 ) ) ;
#16827 = CARTESIAN_POINT ( 'NONE',  ( 1.041310694851599550, 104.6144662015456817, 4.721824808304355692 ) ) ;
#16828 = ADVANCED_FACE ( 'NONE', ( #40071 ), #2077, .T. ) ;
#16829 = CARTESIAN_POINT ( 'NONE',  ( 3.205266406700632675, -14.32095172213143641, 3.103221849221895035 ) ) ;
#16830 = CARTESIAN_POINT ( 'NONE',  ( 0.02537255736346739204, 39.20946620154573026, -1.269746523260778748 ) ) ;
#16831 = CARTESIAN_POINT ( 'NONE',  ( 3.740144479511048559, 121.0798372856833538, 0.007817740762067634797 ) ) ;
#16832 = CIRCLE ( 'NONE', #13435, 9.048749999999998295 ) ;
#16833 = ORIENTED_EDGE ( 'NONE', *, *, #8614, .T. ) ;
#16834 = CARTESIAN_POINT ( 'NONE',  ( -4.369275640764541002, 112.0482830817664137, 2.684166018868272552 ) ) ;
#16835 = CARTESIAN_POINT ( 'NONE',  ( 1.038904431729710920, 105.9875614017122274, 5.236931198412617228 ) ) ;
#16836 = DIRECTION ( 'NONE',  ( -0.8745520943968243532, 0.4849315768086547296, -5.361993529360573944E-16 ) ) ;
#16837 = DIRECTION ( 'NONE',  ( -0.000000000000000000, -0.000000000000000000, -1.000000000000000000 ) ) ;
#16838 = CARTESIAN_POINT ( 'NONE',  ( 13.43120660244749942, 156.9273374874128137, 0.2039374989780119718 ) ) ;
#16839 =( BOUNDED_SURFACE ( )  B_SPLINE_SURFACE ( 3, 2, ( 
 ( #8350, #30295, #4964 ),
 ( #36915, #33932, #11123 ),
 ( #21320, #10909, #24111 ),
 ( #17713, #4761, #34348 ),
 ( #20484, #26894, #7733 ),
 ( #23899, #932, #30712 ),
 ( #30506, #37119, #37527 ),
 ( #5179, #18132, #33510 ),
 ( #27530, #1561, #21113 ),
 ( #4344, #13904, #17306 ) ),
 .UNSPECIFIED., .F., .F., .F. ) 
 B_SPLINE_SURFACE_WITH_KNOTS ( ( 4, 2, 2, 2, 4 ),
 ( 3, 3 ),
 ( 3.141592653589792672, 3.534291735288516811, 3.926990816987241395, 4.319689898685965090, 4.712388980384689674 ),
 ( 0.000000000000000000, 1.000000000000000000 ),
 .UNSPECIFIED. ) 
 GEOMETRIC_REPRESENTATION_ITEM ( )  RATIONAL_B_SPLINE_SURFACE ( (
 ( 1.000000000000000000, 0.7572803591334824613, 1.000000000000000000),
 ( 1.000000000000000000, 0.7572851909592176467, 1.000000000000000000),
 ( 1.000000000000000000, 0.7560206254140762194, 1.000000000000000000),
 ( 1.000000000000000000, 0.7511365686956508192, 1.000000000000000000),
 ( 1.000000000000000000, 0.7475127447244064305, 1.000000000000000000),
 ( 1.000000000000000000, 0.7383589052088851412, 1.000000000000000000),
 ( 1.000000000000000000, 0.7328301610707728120, 1.000000000000000000),
 ( 1.000000000000000000, 0.7206031636698049248, 1.000000000000000000),
 ( 1.000000000000000000, 0.7139102541742058383, 1.000000000000000000),
 ( 1.000000000000000000, 0.7071067811865475727, 1.000000000000000000) ) ) 
 REPRESENTATION_ITEM ( '' )  SURFACE ( )  );
#16840 = CARTESIAN_POINT ( 'NONE',  ( -5.516342712684657812, 117.4962825466697467, 0.6091453463174709704 ) ) ;
#16841 = AXIS2_PLACEMENT_3D ( 'NONE', #26993, #41621, #12000 ) ;
#16842 = CARTESIAN_POINT ( 'NONE',  ( -2.215833297304112381, 118.7629491485454167, 1.137586326187810082 ) ) ;
#16843 = DIRECTION ( 'NONE',  ( -5.206863593109713661E-17, 1.000000000000000000, -1.077750396879097183E-30 ) ) ;
#16844 = CARTESIAN_POINT ( 'NONE',  ( -4.169593158777295194, 32.11536586671030591, 0.7217217036562449950 ) ) ;
#16845 = CARTESIAN_POINT ( 'NONE',  ( 13.64080552068789487, 122.3361261571837986, 1.764911742735522537 ) ) ;
#16846 = CARTESIAN_POINT ( 'NONE',  ( -1.535301415185580609, 19.99377045568717293, 4.360315235486975638 ) ) ;
#16847 = CARTESIAN_POINT ( 'NONE',  ( 5.972130579385131810, 18.43406553185754504, -5.949252452957764170 ) ) ;
#16848 = CARTESIAN_POINT ( 'NONE',  ( -8.629662989089693426, 118.4205806735777600, -1.047178699074468033 ) ) ;
#16849 = CARTESIAN_POINT ( 'NONE',  ( -1.600579373210057055, 119.3928400758114918, -0.6828601607076613123 ) ) ;
#16850 = CARTESIAN_POINT ( 'NONE',  ( -5.809014734623222154, 78.89492211486511053, 5.027281507146216910 ) ) ;
#16851 = CARTESIAN_POINT ( 'NONE',  ( -23.94760723868026631, 77.08694321397520355, -1.270000000000005347 ) ) ;
#16852 = CYLINDRICAL_SURFACE ( 'NONE', #2332, 0.2540000000000051106 ) ;
#16853 = CARTESIAN_POINT ( 'NONE',  ( 3.935102970030661673, 16.48578375386999539, 2.424025302511324309 ) ) ;
#16854 = DIRECTION ( 'NONE',  ( -1.000000000000000000, 9.627370216492862708E-17, 0.000000000000000000 ) ) ;
#16855 = FACE_OUTER_BOUND ( 'NONE', #30456, .T. ) ;
#16856 = CARTESIAN_POINT ( 'NONE',  ( 2.843374750741399559, -13.00285448706176084, 0.5077109796929276664 ) ) ;
#16857 = CARTESIAN_POINT ( 'NONE',  ( 2.312669815851102317, 124.5312663981120380, 0.02133033151766260474 ) ) ;
#16858 = CARTESIAN_POINT ( 'NONE',  ( -3.862028650946987884, 117.0275016673472663, 0.3788463918649359052 ) ) ;
#16859 = CARTESIAN_POINT ( 'NONE',  ( 4.854370033424973307, 117.4083523622822298, -0.9982548204258623326 ) ) ;
#16860 = ORIENTED_EDGE ( 'NONE', *, *, #12063, .F. ) ;
#16861 = DIRECTION ( 'NONE',  ( 0.3256999990547836399, 0.9454731675810339464, 0.000000000000000000 ) ) ;
#16862 = ORIENTED_EDGE ( 'NONE', *, *, #20903, .T. ) ;
#16863 = CARTESIAN_POINT ( 'NONE',  ( -6.784104592523965728E-14, 136.3644662015457527, 7.159772606002533724E-18 ) ) ;
#16864 = CARTESIAN_POINT ( 'NONE',  ( 4.918313631922730522, -15.33159817589810281, -0.1794070962640156031 ) ) ;
#16865 = CARTESIAN_POINT ( 'NONE',  ( -16.44572402506200248, 128.5611466799914240, 1.520858254922803354 ) ) ;
#16866 = CARTESIAN_POINT ( 'NONE',  ( 10.89609060007105867, 119.5270080912504653, -0.8636533125102805464 ) ) ;
#16867 = CARTESIAN_POINT ( 'NONE',  ( 4.560362914109654220, -11.68884639558073069, 0.6953251057713033534 ) ) ;
#16868 = CARTESIAN_POINT ( 'NONE',  ( -58.70775671454279632, -0.3148938609545903211, -0.2814231133491895132 ) ) ;
#16869 = ORIENTED_EDGE ( 'NONE', *, *, #27165, .T. ) ;
#16870 = DIRECTION ( 'NONE',  ( -0.8745520943968235761, 0.4849315768086558398, -4.268512490100410909E-16 ) ) ;
#16871 = CARTESIAN_POINT ( 'NONE',  ( 2.269084004857000458, 124.1308405194309188, 0.09931761310301601142 ) ) ;
#16872 = CARTESIAN_POINT ( 'NONE',  ( -4.773351466264551313, 117.6315869056820418, 0.9547913690014270260 ) ) ;
#16873 = CARTESIAN_POINT ( 'NONE',  ( -0.8386157876100502895, 156.7682548876429109, 1.206618248707300056 ) ) ;
#16874 = CARTESIAN_POINT ( 'NONE',  ( -3.682264917456322895, 63.84746620154572838, -0.07358041635423923088 ) ) ;
#16875 = CARTESIAN_POINT ( 'NONE',  ( 17.81946051592193925, 148.9562551477873740, -1.662425298156809284 ) ) ;
#16876 = CARTESIAN_POINT ( 'NONE',  ( -10.35908644403310142, 120.1444133044471556, -1.518303869478637491 ) ) ;
#16877 = FACE_BOUND ( 'NONE', #25379, .T. ) ;
#16878 = ORIENTED_EDGE ( 'NONE', *, *, #26845, .F. ) ;
#16879 = CARTESIAN_POINT ( 'NONE',  ( 4.514071185496203675, 118.1172072462845648, -0.5456106512196506886 ) ) ;
#16880 = CARTESIAN_POINT ( 'NONE',  ( 10.74829939017195635, 126.1521286088116369, -0.3663887985317100804 ) ) ;
#16881 = EDGE_LOOP ( 'NONE', ( #7966, #38209, #30590, #22905 ) ) ;
#16882 = CARTESIAN_POINT ( 'NONE',  ( 3.411949332026259274, -14.94726182254324520, 2.206293558762954188 ) ) ;
#16883 = CARTESIAN_POINT ( 'NONE',  ( 5.040103533774599853, 105.1217021379421084, -1.780561253959252577 ) ) ;
#16884 = CARTESIAN_POINT ( 'NONE',  ( -58.33447198145985624, -0.2173903971932067414, 0.2351149084158423719 ) ) ;
#16885 = CARTESIAN_POINT ( 'NONE',  ( 0.02375515148176195884, 10.92298121479113426, 4.626086752085273979 ) ) ;
#16886 = CARTESIAN_POINT ( 'NONE',  ( 4.298694136813140609, 120.0471566133196291, 0.8457497992440220491 ) ) ;
#16887 = CARTESIAN_POINT ( 'NONE',  ( -2.817352878905182489, 30.99554970294005685, 0.7112045236633145473 ) ) ;
#16888 = CARTESIAN_POINT ( 'NONE',  ( -0.2480930319908794535, 10.21371511114847053, -4.635561276548324727 ) ) ;
#16889 = CARTESIAN_POINT ( 'NONE',  ( 15.73804366022553403, 146.9052959264698757, 0.5443085878246290976 ) ) ;
#16890 = DIRECTION ( 'NONE',  ( 0.9998004120163608288, 0.000000000000000000, 0.01997839162482760791 ) ) ;
#16891 = CARTESIAN_POINT ( 'NONE',  ( -54.95604735203036029, 6.474113128985478305, -1.942216106931691444 ) ) ;
#16892 = CARTESIAN_POINT ( 'NONE',  ( -2.153613147569079178, 116.3508512159758226, -0.2939559217719306949 ) ) ;
#16893 = CARTESIAN_POINT ( 'NONE',  ( -0.02983097946891718685, 117.3993836135855418, 1.492864285907047561 ) ) ;
#16894 = CARTESIAN_POINT ( 'NONE',  ( -46.89996537977940960, 25.36638690764230475, -1.726091171922216727 ) ) ;
#16895 = CARTESIAN_POINT ( 'NONE',  ( -48.12344719333864163, 19.06868139646365634, 5.226126700700302941 ) ) ;
#16896 = CARTESIAN_POINT ( 'NONE',  ( -29.05311006333617740, 61.33684941847489114, -1.524000000000005128 ) ) ;
#16897 = B_SPLINE_CURVE_WITH_KNOTS ( 'NONE', 3,
 ( #7351, #17340, #26514, #33336 ),
 .UNSPECIFIED., .F., .F.,
 ( 4, 4 ),
 ( 0.000000000000000000, 0.5094958736258423659 ),
 .UNSPECIFIED. ) ;
#16898 = CYLINDRICAL_SURFACE ( 'NONE', #17791, 0.5080000000000000071 ) ;
#16899 = LINE ( 'NONE', #32681, #3529 ) ;
#16900 = DIRECTION ( 'NONE',  ( 5.206863593109713661E-17, -1.000000000000000000, 1.077750396879097183E-30 ) ) ;
#16901 = CARTESIAN_POINT ( 'NONE',  ( -58.76922381231047865, 0.08391971067571446508, 0.07695160083611271573 ) ) ;
#16902 = CARTESIAN_POINT ( 'NONE',  ( -58.07447437077728125, 1.735896131820596766, 1.499107834811089113 ) ) ;
#16903 = CARTESIAN_POINT ( 'NONE',  ( -16.78241155767117476, 155.2615993841311877, 0.07296080027729320849 ) ) ;
#16904 = ORIENTED_EDGE ( 'NONE', *, *, #1190, .F. ) ;
#16905 = CARTESIAN_POINT ( 'NONE',  ( -57.34105142390578891, 4.241571993195719870, -1.052207516753799910E-14 ) ) ;
#16906 = CARTESIAN_POINT ( 'NONE',  ( -7.792461912600263219, 122.5708967970961538, -0.3530462997155650595 ) ) ;
#16907 = TOROIDAL_SURFACE ( 'NONE', #6764, 0.7620000000000000107, 0.2540000000000000036 ) ;
#16908 = VERTEX_POINT ( 'NONE', #20025 ) ;
#16909 = DIRECTION ( 'NONE',  ( -9.627370216492862708E-17, -1.000000000000000000, 0.000000000000000000 ) ) ;
#16910 = CARTESIAN_POINT ( 'NONE',  ( -8.959768907663441695, 123.9105667600146177, -0.2128205007565311946 ) ) ;
#16911 = CARTESIAN_POINT ( 'NONE',  ( 6.089492611447847814, -14.32660765653466584, 1.811095812122764270 ) ) ;
#16912 = AXIS2_PLACEMENT_3D ( 'NONE', #29284, #39092, #9894 ) ;
#16913 = CARTESIAN_POINT ( 'NONE',  ( -13.92608219098140232, 121.7708260186165177, 1.076920499313079871 ) ) ;
#16914 = CARTESIAN_POINT ( 'NONE',  ( 1.141857472271699425, 24.90688314728938835, 4.478778191171412182 ) ) ;
#16915 = CARTESIAN_POINT ( 'NONE',  ( 23.26560126724718813, 148.8247458934765461, 0.9199859812867274833 ) ) ;
#16916 = CARTESIAN_POINT ( 'NONE',  ( 2.086111074717174940, -15.67854476527870489, 5.662254629584102972 ) ) ;
#16917 = CARTESIAN_POINT ( 'NONE',  ( -29.35745042155304674, 66.56063108281016127, 1.269999999999993801 ) ) ;
#16918 = CARTESIAN_POINT ( 'NONE',  ( -0.9742996550080020857, -5.754034560434002188, 0.05241923913101136784 ) ) ;
#16919 = CARTESIAN_POINT ( 'NONE',  ( -21.86057864824949704, 151.4416708234707301, -0.7622892283599552732 ) ) ;
#16920 = CARTESIAN_POINT ( 'NONE',  ( -48.40208230357499275, 18.68930050447353253, -5.198873216397010388 ) ) ;
#16921 = FACE_OUTER_BOUND ( 'NONE', #29232, .T. ) ;
#16922 = VERTEX_POINT ( 'NONE', #17260 ) ;
#16923 = CARTESIAN_POINT ( 'NONE',  ( -8.779664665387997502, 117.8111546309878293, 0.2055069415728331406 ) ) ;
#16924 = CARTESIAN_POINT ( 'NONE',  ( -17.99030040960602506, 148.1388135707062474, 1.617688361210429804 ) ) ;
#16925 = CARTESIAN_POINT ( 'NONE',  ( -58.06141239495070749, 0.3713401805837863723, -0.7746908926762229308 ) ) ;
#16926 = CARTESIAN_POINT ( 'NONE',  ( 21.20529034131888224, 148.8133262010608462, 2.309157841868048511 ) ) ;
#16927 = CARTESIAN_POINT ( 'NONE',  ( 1.091998727716591455, 158.1148137021529578, -1.603323485041850072 ) ) ;
#16928 = CARTESIAN_POINT ( 'NONE',  ( 0.6341690014321406110, -14.98600045789189394, -0.7374838701073263003 ) ) ;
#16929 = CARTESIAN_POINT ( 'NONE',  ( -12.43770564682712632, 156.7420262770442037, -1.659670365993107133 ) ) ;
#16930 = CARTESIAN_POINT ( 'NONE',  ( 4.719769988271771410, 117.9725737481287098, -0.6355710737933278898 ) ) ;
#16931 = DIRECTION ( 'NONE',  ( 4.017660918040594346E-17, -1.000000000000000000, -2.376309959284834438E-19 ) ) ;
#16932 = ADVANCED_FACE ( 'NONE', ( #10867 ), #19744, .T. ) ;
#16933 = CARTESIAN_POINT ( 'NONE',  ( 9.755760200704601814, 153.9716628027005925, -0.9476658408544211820 ) ) ;
#16934 = CARTESIAN_POINT ( 'NONE',  ( -9.191399985966498321, 124.2403664864748549, -0.1492717680338158659 ) ) ;
#16935 = ORIENTED_EDGE ( 'NONE', *, *, #40233, .T. ) ;
#16936 = CARTESIAN_POINT ( 'NONE',  ( -8.426631749355234291, 120.7201681212196291, -1.435507493075423691 ) ) ;
#16937 = CARTESIAN_POINT ( 'NONE',  ( 4.909888997889673590, -15.31669448615230422, -0.4577950299049654559 ) ) ;
#16938 = CARTESIAN_POINT ( 'NONE',  ( 3.174366308151880922, 104.6144662015457243, 0.06343139340882769650 ) ) ;
#16939 = CARTESIAN_POINT ( 'NONE',  ( -4.704478397100538167, 117.9644704501329784, -0.8020208166650271142 ) ) ;
#16940 = CARTESIAN_POINT ( 'NONE',  ( -51.81113891419111894, 13.24950054771400332, -4.495723625053127392 ) ) ;
#16941 = LINE ( 'NONE', #23526, #2088 ) ;
#16942 = CARTESIAN_POINT ( 'NONE',  ( 5.693059210196379283, 156.8407539676644546, 1.898889529600695791 ) ) ;
#16943 = CARTESIAN_POINT ( 'NONE',  ( -2.579283729523311308, 34.63205429821886838, 0.7922911722492685938 ) ) ;
#16944 = AXIS2_PLACEMENT_3D ( 'NONE', #30165, #27179, #4831 ) ;
#16945 = CARTESIAN_POINT ( 'NONE',  ( 5.775410652799734201, 116.9337168780244696, 0.1011920919882985798 ) ) ;
#16946 = CARTESIAN_POINT ( 'NONE',  ( 2.510961470319720501, 15.29743382693132148, 8.092466016612050339 ) ) ;
#16947 = CARTESIAN_POINT ( 'NONE',  ( 3.666883307181533436, 120.9289264519876070, 0.3209655359951391063 ) ) ;
#16948 = CARTESIAN_POINT ( 'NONE',  ( 22.42204277426964154, 149.9331680011685251, -0.7277228188736588610 ) ) ;
#16949 = CARTESIAN_POINT ( 'NONE',  ( -43.35906100199900948, 21.49635880980144265, -2.252931129856535097 ) ) ;
#16950 = ORIENTED_EDGE ( 'NONE', *, *, #37873, .T. ) ;
#16951 = DIRECTION ( 'NONE',  ( 5.188838149069472160E-16, -1.699382548006136559E-16, -1.000000000000000000 ) ) ;
#16952 = CARTESIAN_POINT ( 'NONE',  ( -16.14921358636499704, 121.2501203052637493, -0.2714571880805007331 ) ) ;
#16953 = ORIENTED_EDGE ( 'NONE', *, *, #21517, .T. ) ;
#16954 = CARTESIAN_POINT ( 'NONE',  ( -6.632770492600033485, 120.7515164533844398, -1.069572372112960634 ) ) ;
#16955 = DIRECTION ( 'NONE',  ( 0.9998004120163608288, 4.016384292689131511E-17, 0.01997839162482749342 ) ) ;
#16956 = CARTESIAN_POINT ( 'NONE',  ( -9.178653662903588639, 123.9301100385560943, -0.5015510438870897092 ) ) ;
#16957 = CARTESIAN_POINT ( 'NONE',  ( 2.228616319073483787, -14.90713850702725374, 5.562102343610016320 ) ) ;
#16958 = CARTESIAN_POINT ( 'NONE',  ( -21.25505906629481245, 136.5942649496780632, 0.9712689567086304487 ) ) ;
#16959 = CARTESIAN_POINT ( 'NONE',  ( -11.83539255247756117, 152.0195595274622349, -0.2364993098673504601 ) ) ;
#16960 = CARTESIAN_POINT ( 'NONE',  ( -0.001319893060215945229, 116.4580521601689185, 0.06605284600166366760 ) ) ;
#16961 = ORIENTED_EDGE ( 'NONE', *, *, #31930, .F. ) ;
#16962 = CARTESIAN_POINT ( 'NONE',  ( -3.178183004559932190, -7.902942162671289239, -3.366045245292264010 ) ) ;
#16963 = CARTESIAN_POINT ( 'NONE',  ( 4.250140209130199409, 105.1218014449359117, 3.241604550325138501 ) ) ;
#16964 = CARTESIAN_POINT ( 'NONE',  ( -6.059261036834082681, 78.87450423423038615, 5.016499999999999737 ) ) ;
#16965 = CYLINDRICAL_SURFACE ( 'NONE', #32637, 0.6350000000000006750 ) ;
#16966 = CARTESIAN_POINT ( 'NONE',  ( 8.238225305713989144, 120.2906795671698319, 1.445116664898250303 ) ) ;
#16967 = VECTOR ( 'NONE', #40412, 1000.000000000000114 ) ;
#16968 = CARTESIAN_POINT ( 'NONE',  ( 1.294644163514462987, -7.843371450943685375, 4.453423563430108700 ) ) ;
#16969 = CARTESIAN_POINT ( 'NONE',  ( 14.92730792698318076, 121.5307057168427605, 1.330945954902035044 ) ) ;
#16970 = CARTESIAN_POINT ( 'NONE',  ( -58.13403979463072346, 0.7724927387370850163, -1.216435378340507745 ) ) ;
#16972 = CARTESIAN_POINT ( 'NONE',  ( 15.69714418277264123, 125.4375369430449609, -1.335551531390729130 ) ) ;
#16971 = LINE ( 'NONE', #13786, #24319 ) ;
#16973 = CARTESIAN_POINT ( 'NONE',  ( 1.583070580811935191, 1.852152477310867074, 4.353984577079609508 ) ) ;
#16974 = CARTESIAN_POINT ( 'NONE',  ( -22.16805208646096403, 150.4821223471089411, -1.513879355785526348 ) ) ;
#16975 = ADVANCED_FACE ( 'NONE', ( #14262 ), #36239, .T. ) ;
#16976 = VERTEX_POINT ( 'NONE', #39645 ) ;
#16977 = CARTESIAN_POINT ( 'NONE',  ( -11.92666644034625278, 151.9662372315928280, 0.1848526535252738023 ) ) ;
#16978 = CARTESIAN_POINT ( 'NONE',  ( 4.841517317049865987, -14.78816330421856051, 4.356870016251622957 ) ) ;
#16979 = CARTESIAN_POINT ( 'NONE',  ( -41.09670346151922615, 23.04688172092959775, 1.270085369932517194 ) ) ;
#16980 = DIRECTION ( 'NONE',  ( 0.9998004120163609398, 0.000000000000000000, 0.01997839162482749689 ) ) ;
#16981 = EDGE_CURVE ( 'NONE', #24940, #32109, #10026, .T. ) ;
#16982 = ORIENTED_EDGE ( 'NONE', *, *, #31827, .T. ) ;
#16983 = CARTESIAN_POINT ( 'NONE',  ( 13.59052456474551640, 154.1626644387825991, 2.292254590369200873 ) ) ;
#16984 = PLANE ( 'NONE',  #1150 ) ;
#16985 = CARTESIAN_POINT ( 'NONE',  ( 4.756847264626144600, 117.4019737204766329, 1.206737312781331672 ) ) ;
#16986 = CARTESIAN_POINT ( 'NONE',  ( -6.900334503690650934, 117.6856483911789581, 0.5402308543058539358 ) ) ;
#16987 = CARTESIAN_POINT ( 'NONE',  ( -4.837940364245437941, 10.07446788996644038, 6.911991265526966188 ) ) ;
#16988 = CARTESIAN_POINT ( 'NONE',  ( 9.867978122178516998, 123.6875948057429895, 1.092113756099770239 ) ) ;
#16989 = DIRECTION ( 'NONE',  ( -0.9998004120163608288, 0.000000000000000000, -0.01997839162482749342 ) ) ;
#16990 = AXIS2_PLACEMENT_3D ( 'NONE', #19921, #20124, #17358 ) ;
#16991 = PRODUCT_RELATED_PRODUCT_CATEGORY ( 'part', '', ( #1125 ) ) ;
#16992 = CARTESIAN_POINT ( 'NONE',  ( 15.29680631459140017, 120.8527393138689376, -0.2092734171533191523 ) ) ;
#16993 = DIRECTION ( 'NONE',  ( -0.1728608224830406603, 0.000000000000000000, -0.9849462604886047856 ) ) ;
#16994 = CARTESIAN_POINT ( 'NONE',  ( -57.92433820120297838, 0.6686165507389044693, 0.9561099433084984112 ) ) ;
#16995 = CARTESIAN_POINT ( 'NONE',  ( -47.42394374581075311, 23.94708628835674702, 1.773793246466830453 ) ) ;
#16996 = CARTESIAN_POINT ( 'NONE',  ( 5.101394537142137864, 113.7221017772263423, -1.664686724803478679 ) ) ;
#16997 = CARTESIAN_POINT ( 'NONE',  ( -56.34046819891496938, 4.202508019718290022, 2.501728563949842776 ) ) ;
#16998 = CARTESIAN_POINT ( 'NONE',  ( -58.64399535964418675, -0.3105835279867479315, 0.3406522351893582767 ) ) ;
#16999 = EDGE_CURVE ( 'NONE', #22644, #22759, #14472, .T. ) ;
#17000 = CARTESIAN_POINT ( 'NONE',  ( -4.429393387400064164, 118.1654609044154824, 0.4666533859188604083 ) ) ;
#17001 = DIRECTION ( 'NONE',  ( -0.8745520943968249084, 0.4849315768086533418, -5.271987356194193006E-16 ) ) ;
#17002 = ORIENTED_EDGE ( 'NONE', *, *, #14689, .T. ) ;
#17003 = CARTESIAN_POINT ( 'NONE',  ( -47.07934102874904170, 22.98505637820369429, 3.579966862081928713 ) ) ;
#17004 = EDGE_CURVE ( 'NONE', #19659, #11397, #25865, .T. ) ;
#17005 = CARTESIAN_POINT ( 'NONE',  ( -3.956238299408818104, 119.1072596976981686, -0.9222601227749728237 ) ) ;
#17006 = CARTESIAN_POINT ( 'NONE',  ( -5.328278062783084579, 116.9387654363850260, -0.9571818161585842200 ) ) ;
#17007 = CARTESIAN_POINT ( 'NONE',  ( 4.488792732110129968, 118.1174534351576710, 0.7255436720916952353 ) ) ;
#17008 = CARTESIAN_POINT ( 'NONE',  ( -3.609032566395439012, 120.7384399880717467, -0.4518473439704069894 ) ) ;
#17009 = CARTESIAN_POINT ( 'NONE',  ( -0.7314521050140387892, 115.7029491485454002, -1.756324785531854671 ) ) ;
#17010 = EDGE_CURVE ( 'NONE', #29909, #5595, #18084, .T. ) ;
#17011 = CARTESIAN_POINT ( 'NONE',  ( 1.101716543613451726, 118.1651004027584122, -0.8326739446211146589 ) ) ;
#17012 = CARTESIAN_POINT ( 'NONE',  ( 6.342742252399900416, 120.0627515544778134, -0.2010047130458858800 ) ) ;
#17013 = CARTESIAN_POINT ( 'NONE',  ( -6.520514997712391292, 120.9817801663137971, -0.9553606176145342799 ) ) ;
#17014 = CARTESIAN_POINT ( 'NONE',  ( -4.171990346301578612, 104.6144662015457385, -4.124402238216698713 ) ) ;
#17015 = DIRECTION ( 'NONE',  ( -0.8745520943968249084, 0.4849315768086533418, -5.311926654347176508E-16 ) ) ;
#17016 = CARTESIAN_POINT ( 'NONE',  ( -11.32337086946255056, 78.46996359545325106, -1.269999999999998908 ) ) ;
#17017 = CARTESIAN_POINT ( 'NONE',  ( -1.558514902584574369, 156.2615677632183235, 0.04594967285455571482 ) ) ;
#17018 = CARTESIAN_POINT ( 'NONE',  ( -3.174366308152012817, 95.34346620154573770, -0.06343139340882730792 ) ) ;
#17019 = CARTESIAN_POINT ( 'NONE',  ( 22.14168286312773404, 150.6715983490228723, 1.403651840795991035 ) ) ;
#17020 = CYLINDRICAL_SURFACE ( 'NONE', #21108, 0.2539999999999937863 ) ;
#17021 = CARTESIAN_POINT ( 'NONE',  ( 2.463764682325012778, -15.17880951736275108, 4.811303307383569816 ) ) ;
#17022 = CIRCLE ( 'NONE', #25211, 0.3810000000000007825 ) ;
#17023 = CARTESIAN_POINT ( 'NONE',  ( -6.683041398157647528, 119.8184877057495754, 1.002300253150233633 ) ) ;
#17024 = CARTESIAN_POINT ( 'NONE',  ( -0.7316449863892299232, -12.60219034754442902, -0.6469547163463490458 ) ) ;
#17025 = CARTESIAN_POINT ( 'NONE',  ( -22.25501949494962517, 137.0232865695268458, -1.151097374996565392 ) ) ;
#17026 = CARTESIAN_POINT ( 'NONE',  ( -0.9739946362265716751, -5.975847910206034896, -0.08934465120823924245 ) ) ;
#17027 = ORIENTED_EDGE ( 'NONE', *, *, #4507, .F. ) ;
#17028 = CARTESIAN_POINT ( 'NONE',  ( -44.02811856515548783, 21.20684991433588351, 2.650346054289406172 ) ) ;
#17029 = CARTESIAN_POINT ( 'NONE',  ( 4.902456202885992376, 117.5302216577071874, 0.8631654989601055261 ) ) ;
#17030 = SHAPE_DEFINITION_REPRESENTATION ( #7581, #22056 ) ;
#17031 = CARTESIAN_POINT ( 'NONE',  ( -13.98505335951055706, 150.2679186505038160, 0.6609695396245746091 ) ) ;
#17032 = CARTESIAN_POINT ( 'NONE',  ( 4.970078376064472003, -11.71998231623441100, 0.7442660586517341192 ) ) ;
#17033 = CARTESIAN_POINT ( 'NONE',  ( 7.187319939301631599, 155.7895407640516510, -1.441898956427383416 ) ) ;
#17034 = CARTESIAN_POINT ( 'NONE',  ( -19.27109647334615161, 148.6897983921382433, -2.507318192549734537 ) ) ;
#17035 = CARTESIAN_POINT ( 'NONE',  ( -4.780813784901702057, 104.6144662015457243, 0.7323647157448879286 ) ) ;
#17036 = CARTESIAN_POINT ( 'NONE',  ( 2.237742905438162122, -15.06201634873256801, 5.120316289255383069 ) ) ;
#17037 = FACE_OUTER_BOUND ( 'NONE', #2956, .T. ) ;
#17038 = CARTESIAN_POINT ( 'NONE',  ( 8.102825354745226250, 122.8525693413601800, 0.01624079103423765880 ) ) ;
#17039 = VERTEX_POINT ( 'NONE', #4713 ) ;
#17040 = FACE_OUTER_BOUND ( 'NONE', #30924, .T. ) ;
#17041 = CARTESIAN_POINT ( 'NONE',  ( -23.69188486464780752, 78.08202335040543574, -1.524000000000005350 ) ) ;
#17042 = CARTESIAN_POINT ( 'NONE',  ( -15.71196903609989626, 80.05455644220629097, -1.524000000000001798 ) ) ;
#17043 = AXIS2_PLACEMENT_3D ( 'NONE', #42043, #5847, #32019 ) ;
#17044 = CARTESIAN_POINT ( 'NONE',  ( -5.036351857865265735, 117.3993844875897139, 0.5494637324817667201 ) ) ;
#17045 = EDGE_CURVE ( 'NONE', #5326, #3481, #24063, .T. ) ;
#17046 = CARTESIAN_POINT ( 'NONE',  ( 16.85745507829906131, 155.2173118157008673, 0.2667832593600953928 ) ) ;
#17047 = DIRECTION ( 'NONE',  ( 5.188838149069472160E-16, -1.699382548006136559E-16, -1.000000000000000000 ) ) ;
#17048 = CARTESIAN_POINT ( 'NONE',  ( 1.889907755066986716, -15.70955065773127401, 5.776080436909005300 ) ) ;
#17049 = CARTESIAN_POINT ( 'NONE',  ( -23.49500000000000455, 71.11999999999999034, 5.016499999999999737 ) ) ;
#17050 = DIRECTION ( 'NONE',  ( 5.188838149069472160E-16, -1.699382548006136559E-16, -1.000000000000000000 ) ) ;
#17051 = CARTESIAN_POINT ( 'NONE',  ( 20.10333444936986069, 149.6821479856479300, 2.421853341415478589 ) ) ;
#17052 = VERTEX_POINT ( 'NONE', #2135 ) ;
#17053 = CARTESIAN_POINT ( 'NONE',  ( -2.203247880972440065, 24.02835216854757405, 8.161197317184477384 ) ) ;
#17054 = CARTESIAN_POINT ( 'NONE',  ( 5.518253758338024895, 117.5767191514016758, -0.7526249397660861318 ) ) ;
#17055 = CARTESIAN_POINT ( 'NONE',  ( -3.148404055480067409, 118.0279923103727242, -0.8990514348027989211 ) ) ;
#17056 = CARTESIAN_POINT ( 'NONE',  ( -5.692269266618634305, 78.90431106374057890, 5.047924920909140134 ) ) ;
#17057 = CARTESIAN_POINT ( 'NONE',  ( -4.002141586467248047, 110.9560809575028912, -3.257691571474720771 ) ) ;
#17058 = CARTESIAN_POINT ( 'NONE',  ( -4.573472120527176443, 105.1215731529328821, 2.768881509815038999 ) ) ;
#17059 = CARTESIAN_POINT ( 'NONE',  ( 4.513502956352341222, 8.064680226961385756, -0.9949261897555528034 ) ) ;
#17060 = EDGE_CURVE ( 'NONE', #16254, #39389, #12944, .T. ) ;
#17061 = DIRECTION ( 'NONE',  ( 0.000000000000000000, 0.000000000000000000, -1.000000000000000000 ) ) ;
#17062 = CARTESIAN_POINT ( 'NONE',  ( -3.882979742979310700, 109.3893691838257354, -3.664566828557135114 ) ) ;
#17063 = CARTESIAN_POINT ( 'NONE',  ( 2.870361413894247260, -14.70454541201141119, 4.341408117703424274 ) ) ;
#17064 = CARTESIAN_POINT ( 'NONE',  ( 5.854232237047439114, 124.7508695889173111, 0.1141955550013107751 ) ) ;
#17065 = CARTESIAN_POINT ( 'NONE',  ( -15.53115535783876489, 121.4967652112180048, 0.4657050394012309802 ) ) ;
#17066 = EDGE_CURVE ( 'NONE', #3855, #21812, #27902, .T. ) ;
#17067 = CARTESIAN_POINT ( 'NONE',  ( 5.913343974131921144, 116.9636705803897456, 0.1181626845772993789 ) ) ;
#17068 = CARTESIAN_POINT ( 'NONE',  ( -25.97603047661466036, 74.27059221564131519, -1.270000000000006013 ) ) ;
#17069 = ORIENTED_EDGE ( 'NONE', *, *, #39197, .F. ) ;
#17070 = CARTESIAN_POINT ( 'NONE',  ( -5.208855653336853742, 31.38455280743060527, -0.6720767434146609487 ) ) ;
#17071 = CARTESIAN_POINT ( 'NONE',  ( 2.830806653267172734, -15.77471167405206032, 5.191726263073638492 ) ) ;
#17072 = CARTESIAN_POINT ( 'NONE',  ( -20.31268976784564373, 148.7458375694471044, 1.664162616495830305 ) ) ;
#17073 = AXIS2_PLACEMENT_3D ( 'NONE', #6509, #9903, #32708 ) ;
#17074 = CARTESIAN_POINT ( 'NONE',  ( -1.251853189678833411, -4.679435864505671283, 4.458631606201990394 ) ) ;
#17075 = CARTESIAN_POINT ( 'NONE',  ( -58.63704644534278998, -0.3018330928726550844, -0.3571578142998330097 ) ) ;
#17076 = ORIENTED_EDGE ( 'NONE', *, *, #24320, .T. ) ;
#17077 = CARTESIAN_POINT ( 'NONE',  ( -58.35171525856278407, -0.2536858515839318651, -0.1680674994487795226 ) ) ;
#17078 = CARTESIAN_POINT ( 'NONE',  ( 1.788686868885968506, 120.9773948236336878, 0.4149341611056207579 ) ) ;
#17079 =( NAMED_UNIT ( * ) SI_UNIT ( $, .STERADIAN. ) SOLID_ANGLE_UNIT ( ) );
#17080 = CARTESIAN_POINT ( 'NONE',  ( -17.00008652715119695, 148.0818255213264365, 1.363822447394349213 ) ) ;
#17081 = DIRECTION ( 'NONE',  ( 1.000000000000000000, 0.000000000000000000, 0.000000000000000000 ) ) ;
#17082 = CARTESIAN_POINT ( 'NONE',  ( 2.445625216771064814, 119.3768144667271542, -0.6598031440805111059 ) ) ;
#17083 = TOROIDAL_SURFACE ( 'NONE', #20443, 0.3810000000000000608, 0.2540000000000000036 ) ;
#17084 = CARTESIAN_POINT ( 'NONE',  ( -12.98660267081559105, 122.0079276396459704, -1.762897954238471954 ) ) ;
#17085 = CARTESIAN_POINT ( 'NONE',  ( -10.73808814597608574, 77.14487411131506178, 1.270000000000000684 ) ) ;
#17086 = CARTESIAN_POINT ( 'NONE',  ( 4.117406091950198466, 118.2429491485453354, -0.1872858632366372345 ) ) ;
#17087 = CARTESIAN_POINT ( 'NONE',  ( 16.01386893308418635, 146.3393691146323761, -0.4087692286948388376 ) ) ;
#17088 = EDGE_LOOP ( 'NONE', ( #13252, #34853, #22935, #10551 ) ) ;
#17089 = CARTESIAN_POINT ( 'NONE',  ( 2.102798109511007318, -15.25784609616889753, 5.176374340497880588 ) ) ;
#17090 = CARTESIAN_POINT ( 'NONE',  ( 0.1605948352954452707, 105.1223807299189588, -5.342326028501328317 ) ) ;
#17091 = CARTESIAN_POINT ( 'NONE',  ( -58.35474420885229563, -0.2600319066115991395, 0.1537082109190309465 ) ) ;
#17092 = CARTESIAN_POINT ( 'NONE',  ( -4.027482788729651375, -0.2968512080594384317, 2.264360808822050597 ) ) ;
#17093 = CARTESIAN_POINT ( 'NONE',  ( 11.37357585002882843, 124.5424752485109963, 1.510439678823544574 ) ) ;
#17094 = CARTESIAN_POINT ( 'NONE',  ( 2.744290041233341970, 37.36458345705863593, -0.9092844709908223244 ) ) ;
#17095 = CIRCLE ( 'NONE', #32076, 0.6350000000000001199 ) ;
#17096 = CARTESIAN_POINT ( 'NONE',  ( 0.1710433496020407063, 14.98650505531991506, 4.637963194678765610 ) ) ;
#17097 = CARTESIAN_POINT ( 'NONE',  ( 15.72281364106769352, 146.8976350983841144, 0.3655119725415951204 ) ) ;
#17098 = DIRECTION ( 'NONE',  ( 0.8620390596215063983, 0.5065490486308654727, 0.01722559195018080053 ) ) ;
#17099 = EDGE_CURVE ( 'NONE', #22469, #30132, #39509, .T. ) ;
#17100 = CARTESIAN_POINT ( 'NONE',  ( -51.79385399617232366, 10.81633633057992050, -0.6965991018155879289 ) ) ;
#17101 = CARTESIAN_POINT ( 'NONE',  ( -8.788814435013840409, 117.7123315311960710, -0.3507367455258986189 ) ) ;
#17102 = CARTESIAN_POINT ( 'NONE',  ( 5.586884702347363785, 117.3144662015457271, 0.1116392523995368424 ) ) ;
#17103 = AXIS2_PLACEMENT_3D ( 'NONE', #34658, #18873, #37424 ) ;
#17104 = CARTESIAN_POINT ( 'NONE',  ( -4.855072294470597072, 115.7029491485453718, 1.279409886141102071 ) ) ;
#17105 = CARTESIAN_POINT ( 'NONE',  ( -10.75478607932181241, 82.07015292912137738, -1.269999999999999130 ) ) ;
#17106 = CARTESIAN_POINT ( 'NONE',  ( -31.81160527991017872, 53.04071001975501076, -1.523999999997152521 ) ) ;
#17107 = CARTESIAN_POINT ( 'NONE',  ( -0.9514613986627886710, 10.21077804425927305, -8.405459466743828045 ) ) ;
#17108 = EDGE_CURVE ( 'NONE', #40141, #38260, #13605, .T. ) ;
#17109 = CARTESIAN_POINT ( 'NONE',  ( 1.247998466936323035E-15, 12.96302561210691806, 0.000000000000000000 ) ) ;
#17110 = DIRECTION ( 'NONE',  ( -5.188838149069472160E-16, 1.699382548006136559E-16, 1.000000000000000000 ) ) ;
#17111 = CARTESIAN_POINT ( 'NONE',  ( -58.13344828981739454, 1.721081384412917359, 0.8123818723938425190 ) ) ;
#17112 = CARTESIAN_POINT ( 'NONE',  ( 14.73199999999999932, 12.96416000000000146, 0.000000000000000000 ) ) ;
#17113 = CARTESIAN_POINT ( 'NONE',  ( -3.265120802789957200, 159.4600617640778353, 0.2122772200314293756 ) ) ;
#17114 = VERTEX_POINT ( 'NONE', #16136 ) ;
#17115 = CARTESIAN_POINT ( 'NONE',  ( -56.26154134542980501, 7.775270144418685803, -1.077953313861507864E-14 ) ) ;
#17116 = CARTESIAN_POINT ( 'NONE',  ( 7.795928871158808171, 122.5882798252810062, 0.001158467290666534508 ) ) ;
#17117 = ORIENTED_EDGE ( 'NONE', *, *, #33964, .T. ) ;
#17118 = DIRECTION ( 'NONE',  ( -0.8745520943968235761, 0.4849315768086558953, -5.361993529360570985E-16 ) ) ;
#17119 = CARTESIAN_POINT ( 'NONE',  ( -14.67383990354524492, 148.8475317811793559, -0.3438330757172305407 ) ) ;
#17120 = CARTESIAN_POINT ( 'NONE',  ( 6.086938242954471612, -13.85866328171454853, 1.967354546201298682 ) ) ;
#17121 = AXIS2_PLACEMENT_3D ( 'NONE', #27547, #24337, #34158 ) ;
#17122 = CARTESIAN_POINT ( 'NONE',  ( -21.15257933310689253, 148.4376209648218321, 1.514591261405503930 ) ) ;
#17123 = CARTESIAN_POINT ( 'NONE',  ( 3.979181138743986601, 26.09377549647152961, 2.406711837290479661 ) ) ;
#17124 = CARTESIAN_POINT ( 'NONE',  ( 3.764301891765636121, 116.7207137014398626, 0.2841661138181406088 ) ) ;
#17125 = CARTESIAN_POINT ( 'NONE',  ( -6.453647670433203483E-14, 66.13346620154574396, 1.207165459738467839E-19 ) ) ;
#17126 = CARTESIAN_POINT ( 'NONE',  ( -30.04222987988044835, 57.94556081694326366, 1.269999999999993801 ) ) ;
#17127 = CARTESIAN_POINT ( 'NONE',  ( 0.2014313232957813393, -8.551994341567581870, -0.9548264729560895780 ) ) ;
#17128 = CARTESIAN_POINT ( 'NONE',  ( -1.837930215757131558, 116.5452236745340429, -0.1764961812833932275 ) ) ;
#17129 = CARTESIAN_POINT ( 'NONE',  ( 5.177913976931212581, 57.15000000000004832, -5.372100000000001430 ) ) ;
#17130 = CARTESIAN_POINT ( 'NONE',  ( 4.937033159817793226, 117.4086831280190637, 1.082238659715207607 ) ) ;
#17131 = CARTESIAN_POINT ( 'NONE',  ( 8.759280421985048193, 117.8332167676661868, 0.5881991161353357089 ) ) ;
#17132 = CARTESIAN_POINT ( 'NONE',  ( -2.123774309200991972, 157.0334531201187644, 1.456117127909798414 ) ) ;
#17133 = CARTESIAN_POINT ( 'NONE',  ( -57.73431293437639056, 1.079294370200192699, -1.168893109563275301 ) ) ;
#17134 = CARTESIAN_POINT ( 'NONE',  ( 21.11954758237290619, 149.1058327099893290, 2.305704729659640240 ) ) ;
#17135 = CARTESIAN_POINT ( 'NONE',  ( 19.58040708638629468, 147.7952244890416296, -1.737278836974155416 ) ) ;
#17136 = CARTESIAN_POINT ( 'NONE',  ( -0.02964290590182637811, -9.142985105544495283, 0.9735349185509928338 ) ) ;
#17137 = CARTESIAN_POINT ( 'NONE',  ( -21.44537552191025753, 145.9698620541949765, -2.253500464710097795 ) ) ;
#17138 = B_SPLINE_CURVE_WITH_KNOTS ( 'NONE', 3,
 ( #4121, #919, #36690, #10692, #7724, #16658, #10064, #14096, #20690, #33715, #4536, #17498, #1337, #26248, #39257, #23035, #37733, #8341, #1757, #33919, #34550, #11113, #27520, #24730 ),
 .UNSPECIFIED., .F., .F.,
 ( 4, 2, 2, 2, 2, 2, 2, 2, 2, 2, 2, 4 ),
 ( 0.000000000000000000, 0.0005547041830063565359, 0.001109408366012713072, 0.001664112549019069716, 0.002218816732025426144, 0.003328225098038139432, 0.004437633464050852287, 0.005547041830063565576, 0.006656450196076278865, 0.007211154379082635076, 0.007765858562088991286, 0.008875266928101688962 ),
 .UNSPECIFIED. ) ;
#17139 = CARTESIAN_POINT ( 'NONE',  ( -42.79661761208809168, 21.81806929429799879, -2.089873509012822428 ) ) ;
#17140 = CIRCLE ( 'NONE', #37534, 0.2540000000000000036 ) ;
#17141 = CARTESIAN_POINT ( 'NONE',  ( 4.755892522628037966, 104.6144662015434932, 2.421412838250809774 ) ) ;
#17142 = CARTESIAN_POINT ( 'NONE',  ( 7.181592176188103416, 121.6016026263613838, -0.5649366106928355169 ) ) ;
#17143 = CARTESIAN_POINT ( 'NONE',  ( 7.819172660177973633, 122.4257783361165366, 0.5980713627250896502 ) ) ;
#17144 = VERTEX_POINT ( 'NONE', #12126 ) ;
#17145 = CARTESIAN_POINT ( 'NONE',  ( -8.285153246922989823, 121.0263440914440736, -1.363535410649704627 ) ) ;
#17146 = CARTESIAN_POINT ( 'NONE',  ( 2.197863461560763287, -15.74995721546218519, 5.600911867769769792 ) ) ;
#17147 = CARTESIAN_POINT ( 'NONE',  ( -58.85052583756497313, -0.2027389052197895725, -7.881329963315141238E-15 ) ) ;
#17148 = CARTESIAN_POINT ( 'NONE',  ( -4.590648100572289003, 117.9758294621954064, -0.9228213078436219297 ) ) ;
#17149 = CARTESIAN_POINT ( 'NONE',  ( -49.13940628111213016, 17.59503125033257120, -5.062072503518689537 ) ) ;
#17150 = B_SPLINE_CURVE_WITH_KNOTS ( 'NONE', 3,
 ( #23792, #26798, #10810, #23579, #11226, #14414, #36813, #36399, #17821, #33826, #27421, #4449, #30613, #40435, #39807, #33201, #30197, #21014 ),
 .UNSPECIFIED., .F., .F.,
 ( 4, 2, 1, 1, 2, 2, 2, 2, 2, 4 ),
 ( -5.999999999820153193E-08, 0.0006526371903139581345, 0.001305334380627914612, 0.002610728761255789402, 0.003916123141883664192, 0.005221517522511539416, 0.01044309504502295531, 0.01305388380627865198, 0.01566467256753434692, 0.02088625009004572639 ),
 .UNSPECIFIED. ) ;
#17151 = CARTESIAN_POINT ( 'NONE',  ( -23.91048590848665611, 81.84235438443283783, -1.524000000000006239 ) ) ;
#17152 = CARTESIAN_POINT ( 'NONE',  ( 11.58692091624685183, 123.4149316504530702, 1.682406715187617419 ) ) ;
#17153 = CARTESIAN_POINT ( 'NONE',  ( 0.03519895179118932155, 115.7029491485452866, -1.761499482103553449 ) ) ;
#17154 = VECTOR ( 'NONE', #37970, 1000.000000000000227 ) ;
#17155 = CARTESIAN_POINT ( 'NONE',  ( 17.29948542670041078, 122.7677429521249053, 0.3279718759250788152 ) ) ;
#17156 = CARTESIAN_POINT ( 'NONE',  ( -8.041749784432907333, 11.96416136180153345, -2.598976288244244870 ) ) ;
#17157 = CARTESIAN_POINT ( 'NONE',  ( 7.635798533888219275, 122.3449549946481056, 0.5106263504299668465 ) ) ;
#17158 = CARTESIAN_POINT ( 'NONE',  ( 14.96085986107146226, 121.2513550155162960, -0.6271060280491597139 ) ) ;
#17159 = CARTESIAN_POINT ( 'NONE',  ( -46.91190649557952952, 20.26356613537010887, -4.963267847376400255 ) ) ;
#17160 = DIRECTION ( 'NONE',  ( -1.000000000000000000, 1.044409991968847425E-16, 0.000000000000000000 ) ) ;
#17161 = TOROIDAL_SURFACE ( 'NONE', #8997, 0.7620000000000000107, 0.2540000000000000036 ) ;
#17162 = EDGE_CURVE ( 'NONE', #14331, #15131, #6165, .T. ) ;
#17163 = CARTESIAN_POINT ( 'NONE',  ( -18.81756541077873734, 125.3161215262879580, -0.3201835051929644016 ) ) ;
#17164 = ORIENTED_EDGE ( 'NONE', *, *, #12808, .T. ) ;
#17165 = CARTESIAN_POINT ( 'NONE',  ( -5.198628926520693305, 120.3590328494841231, -0.8315808706636761416 ) ) ;
#17166 = CARTESIAN_POINT ( 'NONE',  ( -46.78089565521672455, 25.32111429335394348, -1.738356225806591882 ) ) ;
#17167 = ORIENTED_EDGE ( 'NONE', *, *, #26607, .F. ) ;
#17168 = DIRECTION ( 'NONE',  ( -0.6825627711659328911, -0.7308269722843309113, -2.299753143848213649E-16 ) ) ;
#17169 = CARTESIAN_POINT ( 'NONE',  ( -15.70678031088822202, 147.2451778420852406, -0.7656494529899995349 ) ) ;
#17170 = CARTESIAN_POINT ( 'NONE',  ( 4.589616127059429118, -13.46842606041413681, 3.597705605327369494 ) ) ;
#17171 = CARTESIAN_POINT ( 'NONE',  ( -1.068372181839257751, 117.3444111807523882, 0.4585463030235088500 ) ) ;
#17172 = CARTESIAN_POINT ( 'NONE',  ( -41.09676540851937432, 23.04694042099054840, 1.523999999999987587 ) ) ;
#17173 = CARTESIAN_POINT ( 'NONE',  ( 3.725034515352382503, 116.6403000632267464, 0.1520601685204153175 ) ) ;
#17174 = VERTEX_POINT ( 'NONE', #25326 ) ;
#17175 = CARTESIAN_POINT ( 'NONE',  ( -4.288638401707804526, -7.253218809911426312, -1.756103832032595680 ) ) ;
#17176 = CARTESIAN_POINT ( 'NONE',  ( -20.69846590548381826, 152.5542719854981044, -0.4384689201006752857 ) ) ;
#17177 = CARTESIAN_POINT ( 'NONE',  ( -6.059261036834486802, 71.63300248836199557, 5.016499999999999737 ) ) ;
#17178 = DIRECTION ( 'NONE',  ( 0.9891443546370349837, 0.000000000000000000, -0.1469470846586742874 ) ) ;
#17179 = EDGE_LOOP ( 'NONE', ( #22662, #41671, #14645, #16175, #23620, #7986, #39041, #26256, #13352, #6751, #42050, #41305 ) ) ;
#17180 = CARTESIAN_POINT ( 'NONE',  ( -4.860571518730761653, 119.0032906492853328, 0.8981773809672630726 ) ) ;
#17181 = CARTESIAN_POINT ( 'NONE',  ( 2.776928087254650013, 2.301956178644051221, 3.707541451904531105 ) ) ;
#17182 = CARTESIAN_POINT ( 'NONE',  ( 22.23208127788751298, 149.2301036976659816, 1.887777678714757990 ) ) ;
#17183 = CARTESIAN_POINT ( 'NONE',  ( -58.80981292533109439, -0.2807566353365542611, -0.1195710083432118126 ) ) ;
#17185 = CARTESIAN_POINT ( 'NONE',  ( 20.75411281516084117, 147.9587796579421308, -1.616985229673752578 ) ) ;
#17184 = DIRECTION ( 'NONE',  ( 0.01997839162482749689, 1.040247600000945640E-18, -0.9998004120163610509 ) ) ;
#17186 = CARTESIAN_POINT ( 'NONE',  ( 4.587442282481145384, -5.694351208059624803, -0.5507456681084095251 ) ) ;
#17187 = CARTESIAN_POINT ( 'NONE',  ( 0.006942562093231309170, 117.0978366787122127, -0.3474341964894883117 ) ) ;
#17188 = ORIENTED_EDGE ( 'NONE', *, *, #15412, .T. ) ;
#17189 = B_SPLINE_CURVE_WITH_KNOTS ( 'NONE', 3,
 ( #24906, #41325, #5135, #21690 ),
 .UNSPECIFIED., .F., .F.,
 ( 4, 4 ),
 ( 0.02839955696672210456, 1.000000000000000000 ),
 .UNSPECIFIED. ) ;
#17190 = CARTESIAN_POINT ( 'NONE',  ( -15.68661553393327779, 147.2319784351455780, 0.01612984191841678600 ) ) ;
#17191 = CARTESIAN_POINT ( 'NONE',  ( 5.819126084642364916, -14.14507005385615201, 2.709888076677010371 ) ) ;
#17192 = CARTESIAN_POINT ( 'NONE',  ( -42.04985097881080236, 22.19100705996942935, 1.479702663569726573 ) ) ;
#17193 = CARTESIAN_POINT ( 'NONE',  ( -0.07396841670801596047, 117.3993836134566067, -1.494938445543764427 ) ) ;
#17194 = ORIENTED_EDGE ( 'NONE', *, *, #33957, .F. ) ;
#17195 = CARTESIAN_POINT ( 'NONE',  ( 12.32670121879455927, 122.4057692182592092, 1.805994760647165576 ) ) ;
#17196 = LINE ( 'NONE', #7837, #18913 ) ;
#17197 = ADVANCED_FACE ( 'NONE', ( #6367 ), #39544, .T. ) ;
#17198 = LINE ( 'NONE', #7839, #29343 ) ;
#17199 = AXIS2_PLACEMENT_3D ( 'NONE', #11234, #23586, #16993 ) ;
#17200 = CARTESIAN_POINT ( 'NONE',  ( -22.48855060683877838, 149.3130771379323392, 0.8549704587061034422 ) ) ;
#17201 = CARTESIAN_POINT ( 'NONE',  ( -7.252988161461171757, 9.422892264050933164, 4.294140714350721311 ) ) ;
#17202 = CARTESIAN_POINT ( 'NONE',  ( 5.176742542608628206, 120.9449653624321144, 0.6121131393098595552 ) ) ;
#17203 = DIRECTION ( 'NONE',  ( 0.01997839162482749689, 1.040247600000945640E-18, -0.9998004120163610509 ) ) ;
#17204 = EDGE_CURVE ( 'NONE', #29982, #2001, #35432, .T. ) ;
#17205 = CARTESIAN_POINT ( 'NONE',  ( 8.172070396905905199, 117.7057695168643932, -0.3161122371724935376 ) ) ;
#17206 = FACE_OUTER_BOUND ( 'NONE', #6286, .T. ) ;
#17207 = CARTESIAN_POINT ( 'NONE',  ( -53.65353144418239140, 9.505953006310818409, 3.603183245156613701 ) ) ;
#17208 = CARTESIAN_POINT ( 'NONE',  ( -50.64083583777225073, 22.17031204481727258, 0.3653657693499628989 ) ) ;
#17209 = CARTESIAN_POINT ( 'NONE',  ( 5.274109024393328404, 115.7029491485453150, -0.8140283081321303404 ) ) ;
#17210 = CARTESIAN_POINT ( 'NONE',  ( -55.41603145274652320, 6.826612083464994818, 3.210495615568572436 ) ) ;
#17211 = CARTESIAN_POINT ( 'NONE',  ( -58.62683610494525510, -0.2852240180758755517, 0.3850767576232742018 ) ) ;
#17212 = ADVANCED_FACE ( 'NONE', ( #15775 ), #22470, .T. ) ;
#17213 = CARTESIAN_POINT ( 'NONE',  ( -4.486895273669365025, 118.1299698726477914, 0.5326488260592314727 ) ) ;
#17214 = CARTESIAN_POINT ( 'NONE',  ( 2.918624193109982112, 107.9147049449184976, -4.333181634890918232 ) ) ;
#17215 = VERTEX_POINT ( 'NONE', #24262 ) ;
#17216 = CARTESIAN_POINT ( 'NONE',  ( -46.97515415817095175, 24.89137758704647396, 2.045406795549891577 ) ) ;
#17217 = CARTESIAN_POINT ( 'NONE',  ( -3.967643248668881295, 119.1178733970733958, -0.9224967296737327516 ) ) ;
#17218 = CARTESIAN_POINT ( 'NONE',  ( -5.345964095105384395, 116.9256180743815179, -0.9586058045032990194 ) ) ;
#17219 = STYLED_ITEM ( 'NONE', ( #4676 ), #24793 ) ;
#17220 = CARTESIAN_POINT ( 'NONE',  ( 4.585886860456856340, 118.0663496363380318, 0.7419266980658387745 ) ) ;
#17221 = CARTESIAN_POINT ( 'NONE',  ( -9.787166303541962264, 124.1138826855306831, -0.8907577946409741543 ) ) ;
#17222 = CARTESIAN_POINT ( 'NONE',  ( -0.1695618695486382776, 115.7029491485452866, -1.764636181574767537 ) ) ;
#17223 = CARTESIAN_POINT ( 'NONE',  ( 0.4467141430003514491, 117.3993820575490901, -1.478549762435686699 ) ) ;
#17224 = CARTESIAN_POINT ( 'NONE',  ( 5.302326897023531771, 116.4520502601644409, -0.8833424955642699139 ) ) ;
#17225 = CARTESIAN_POINT ( 'NONE',  ( -16.68619938060346541, 146.1290494286844819, -1.780952809221992172 ) ) ;
#17226 = ADVANCED_FACE ( 'NONE', ( #7473 ), #36444, .T. ) ;
#17227 = CARTESIAN_POINT ( 'NONE',  ( -28.69846420587789737, 77.20784726182124302, 1.523999999999991806 ) ) ;
#17228 = CARTESIAN_POINT ( 'NONE',  ( 8.131384943450600034, 121.0503350093198662, -0.9968526362123016904 ) ) ;
#17229 = CARTESIAN_POINT ( 'NONE',  ( -7.784012320790520967, 122.6313477007502115, -0.1555430920740401568 ) ) ;
#17230 = CARTESIAN_POINT ( 'NONE',  ( -17.14499999999999957, 71.11999999999999034, 5.714999999999999858 ) ) ;
#17231 = CARTESIAN_POINT ( 'NONE',  ( 0.9708930699731092018, 116.8374933757159795, 0.3283832199399772112 ) ) ;
#17232 = DIRECTION ( 'NONE',  ( 0.9998004120163609398, 0.000000000000000000, 0.01997839162482749689 ) ) ;
#17233 = CARTESIAN_POINT ( 'NONE',  ( 2.233744238265779281, -15.22787141332636374, 5.055619554762198931 ) ) ;
#17234 = CARTESIAN_POINT ( 'NONE',  ( -7.478391884465417583, 120.4750020944285609, 1.007254920367567808 ) ) ;
#17235 = CARTESIAN_POINT ( 'NONE',  ( -0.9396370176409497565, -11.09013235204027659, 0.2555656002325920051 ) ) ;
#17236 = CARTESIAN_POINT ( 'NONE',  ( 0.006534887713546001439, 159.5822087645323393, -0.3270325034788579277 ) ) ;
#17237 = CIRCLE ( 'NONE', #26082, 14.73199999999999577 ) ;
#17238 = CARTESIAN_POINT ( 'NONE',  ( -0.5432096421966324806, 25.39095905668347797, -0.8082079942862561150 ) ) ;
#17239 = ORIENTED_EDGE ( 'NONE', *, *, #20088, .F. ) ;
#17240 = CARTESIAN_POINT ( 'NONE',  ( -54.02436534585504546, 7.965282956745534548, 1.622780670314668994 ) ) ;
#17241 = CARTESIAN_POINT ( 'NONE',  ( 2.249496549248389154, 107.4436264546101967, 4.650814322000806911 ) ) ;
#17242 = ITEM_DEFINED_TRANSFORMATION ( 'NONE', 'NONE', #38658,  #3275 ) ;
#17243 = CARTESIAN_POINT ( 'NONE',  ( -9.732488649496342958, 124.0009531390599591, 0.4956537337270182642 ) ) ;
#17244 = EDGE_CURVE ( 'NONE', #28485, #2780, #36651, .T. ) ;
#17245 = CARTESIAN_POINT ( 'NONE',  ( 4.513689648792266418, -13.57929909251434708, 3.776549439516510898 ) ) ;
#17246 = CARTESIAN_POINT ( 'NONE',  ( 15.51360955034711253, 150.7699688800196611, -1.541415763164774466 ) ) ;
#17247 = EDGE_LOOP ( 'NONE', ( #36053, #8824, #13882, #7628 ) ) ;
#17248 = CARTESIAN_POINT ( 'NONE',  ( -9.741115574333473859, 120.9522862504114897, -1.586783935194494788 ) ) ;
#17249 = CARTESIAN_POINT ( 'NONE',  ( -3.571940676860559272, 104.6144662015457953, 3.260099875215366705 ) ) ;
#17250 = CARTESIAN_POINT ( 'NONE',  ( 3.149239739297259533, -13.85570235734440203, 1.885463239856044027 ) ) ;
#17251 = CARTESIAN_POINT ( 'NONE',  ( -4.773986132821358197, 117.6391641637075338, -1.128576530690340585 ) ) ;
#17252 = ADVANCED_FACE ( 'NONE', ( #17037 ), #10857, .T. ) ;
#17253 = CARTESIAN_POINT ( 'NONE',  ( 3.725873884401345926, 121.0563512343167645, -0.03194638937107874971 ) ) ;
#17254 = ORIENTED_EDGE ( 'NONE', *, *, #11201, .T. ) ;
#17255 = CARTESIAN_POINT ( 'NONE',  ( -2.730960582676723369, 107.1167599116663780, 4.574583874852882204 ) ) ;
#17256 = CARTESIAN_POINT ( 'NONE',  ( 2.864732365555376692, 107.5209036112635630, 4.491122542952314944 ) ) ;
#17257 = AXIS2_PLACEMENT_3D ( 'NONE', #19265, #38461, #12880 ) ;
#17258 = CARTESIAN_POINT ( 'NONE',  ( -3.148524768479886937, 30.89467502894792972, -0.4672404312464801812 ) ) ;
#17259 = ADVANCED_FACE ( 'NONE', ( #33878 ), #12962, .T. ) ;
#17260 = CARTESIAN_POINT ( 'NONE',  ( -18.32410244842765934, 0.6350000000000018963, 0.000000000000000000 ) ) ;
#17261 = CARTESIAN_POINT ( 'NONE',  ( 14.80501208800821011, 120.3086691715681695, 0.1403833142216709406 ) ) ;
#17262 = CARTESIAN_POINT ( 'NONE',  ( 1.650612623617701454E-15, 17.14499999999999957, 0.000000000000000000 ) ) ;
#17263 = CIRCLE ( 'NONE', #17924, 0.7620000000000000107 ) ;
#17264 = CARTESIAN_POINT ( 'NONE',  ( 1.758948546174424976, -15.24573455742719830, 5.911464237579555636 ) ) ;
#17265 = CARTESIAN_POINT ( 'NONE',  ( -17.14499999999999957, 71.11999999999999034, -5.016499999999999737 ) ) ;
#17266 = CARTESIAN_POINT ( 'NONE',  ( -3.409520279599585368, 31.22297404472999816, -0.3972485071703515946 ) ) ;
#17267 = CARTESIAN_POINT ( 'NONE',  ( 9.074718672963324906, 157.1510513929294177, 1.991881423077543012 ) ) ;
#17268 = VERTEX_POINT ( 'NONE', #41849 ) ;
#17269 = CARTESIAN_POINT ( 'NONE',  ( -4.930748812479134990, 13.88268055242722987, 6.853499169485068876 ) ) ;
#17270 = CARTESIAN_POINT ( 'NONE',  ( 2.394128288074550248, 117.2927635608798056, -0.5979285131003549969 ) ) ;
#17271 = CARTESIAN_POINT ( 'NONE',  ( -5.854120942168551167, 124.7508695889173111, -0.1197652058513695994 ) ) ;
#17272 = AXIS2_PLACEMENT_3D ( 'NONE', #12959, #19142, #25953 ) ;
#17274 = DIRECTION ( 'NONE',  ( 1.000000000000000000, -1.365923996832131856E-16, 0.000000000000000000 ) ) ;
#17273 = AXIS2_PLACEMENT_3D ( 'NONE', #19330, #25727, #3377 ) ;
#17275 = DIRECTION ( 'NONE',  ( -0.1906721105965031304, 0.9816537812491097359, -2.460754754889605160E-15 ) ) ;
#17276 = CARTESIAN_POINT ( 'NONE',  ( -7.772068811996249771, 69.25462295839062676, -1.269999999999995577 ) ) ;
#17277 = CARTESIAN_POINT ( 'NONE',  ( -1.576536484031922480, 10.66345178295009788, -4.350723848753511369 ) ) ;
#17278 = CARTESIAN_POINT ( 'NONE',  ( 1.589478822742971486E-15, 16.51000000000000156, 0.000000000000000000 ) ) ;
#17279 = CARTESIAN_POINT ( 'NONE',  ( -1.906939736952270925, 106.4592480297309436, -4.997920180712069893 ) ) ;
#17280 = CARTESIAN_POINT ( 'NONE',  ( 3.134184212546501591, -13.48855807073397273, 1.578073873303884156 ) ) ;
#17281 = CARTESIAN_POINT ( 'NONE',  ( 5.705706447001112736, 123.8402959710505087, 0.07212015369193675030 ) ) ;
#17282 = CARTESIAN_POINT ( 'NONE',  ( -15.41192216945103866, 121.3506620944898060, 0.4643526128083735327 ) ) ;
#17283 = CARTESIAN_POINT ( 'NONE',  ( 1.733480476724572616, 35.69352191795299234, 2.306000102516378547 ) ) ;
#17284 = CARTESIAN_POINT ( 'NONE',  ( -26.51793118801306548, 72.98537704160715123, -1.524000000000006017 ) ) ;
#17285 = ORIENTED_EDGE ( 'NONE', *, *, #1985, .T. ) ;
#17286 = CARTESIAN_POINT ( 'NONE',  ( -4.980122306282216194, 105.1217006149118163, -1.944304085884134503 ) ) ;
#17287 = CIRCLE ( 'NONE', #35001, 0.2540000000000006142 ) ;
#17288 = CARTESIAN_POINT ( 'NONE',  ( 4.642828252855901283, -15.60299999947604910, 2.403246459791627210 ) ) ;
#17289 = CARTESIAN_POINT ( 'NONE',  ( -14.15994444794836227, 154.3735777161816429, 1.715400944796409366 ) ) ;
#17290 = CARTESIAN_POINT ( 'NONE',  ( -0.5842699607273857954, -4.454521554441356557, 4.585487691134133570 ) ) ;
#17291 = ADVANCED_FACE ( 'NONE', ( #12646 ), #12286, .F. ) ;
#17292 = EDGE_LOOP ( 'NONE', ( #10646, #16662, #1556, #6374 ) ) ;
#17293 = DIRECTION ( 'NONE',  ( 0.9998004120163608288, -1.039227405372660929E-20, 0.01997839162482763914 ) ) ;
#17294 = CARTESIAN_POINT ( 'NONE',  ( 0.8775954529456102549, 122.2453746293775652, 0.2818696459738750382 ) ) ;
#17295 = CARTESIAN_POINT ( 'NONE',  ( -14.77909737591013695, 150.5114039713088516, 1.257293140667801179 ) ) ;
#17296 = CARTESIAN_POINT ( 'NONE',  ( -18.19824605342069290, 84.09650579081264254, -1.270000000000003570 ) ) ;
#17297 = CARTESIAN_POINT ( 'NONE',  ( 16.46509630982077255, 135.1966315799913900, -1.639354953089778633 ) ) ;
#17298 = CARTESIAN_POINT ( 'NONE',  ( -13.54337464129344504, 122.2126086331852974, -1.756000464972328867 ) ) ;
#17299 = DIRECTION ( 'NONE',  ( 0.7770581983690701966, -0.6294287539884197979, 8.537024980200731099E-16 ) ) ;
#17300 = CARTESIAN_POINT ( 'NONE',  ( 4.168088869111308270, 118.2394494485767780, -0.2219757712405359684 ) ) ;
#17301 = CARTESIAN_POINT ( 'NONE',  ( 9.597885446028643130, 124.1734284925964573, -0.3307417288639280528 ) ) ;
#17302 = EDGE_LOOP ( 'NONE', ( #32219, #36368, #12758, #25365 ) ) ;
#17303 = B_SPLINE_CURVE_WITH_KNOTS ( 'NONE', 3,
 ( #8240, #8036, #24843, #31230, #21211, #21009 ),
 .UNSPECIFIED., .F., .F.,
 ( 4, 2, 4 ),
 ( 0.0008205648557148674267, 0.001333860798246176271, 0.001847156740777485115 ),
 .UNSPECIFIED. ) ;
#17304 = CARTESIAN_POINT ( 'NONE',  ( 1.853042888461218007, -15.33088210119805339, 5.380378780177352382 ) ) ;
#17305 = EDGE_CURVE ( 'NONE', #37319, #18840, #32692, .T. ) ;
#17306 = CARTESIAN_POINT ( 'NONE',  ( 10.28897677580358128, 57.14999999999999858, -5.016500000000000625 ) ) ;
#17307 = EDGE_CURVE ( 'NONE', #26127, #38326, #16036, .T. ) ;
#17308 = CARTESIAN_POINT ( 'NONE',  ( -58.26714162322902979, -0.07371858623882177053, 0.4245910480440974188 ) ) ;
#17309 = CARTESIAN_POINT ( 'NONE',  ( 4.627658001546194555, 13.29687521248714610, 0.05192310334374634212 ) ) ;
#17310 = CARTESIAN_POINT ( 'NONE',  ( 5.844382469224909116, 120.7327493588883840, 0.8888191899821259456 ) ) ;
#17311 = CARTESIAN_POINT ( 'NONE',  ( -2.672954704825328598, 29.71133030240788386, 0.5376189070171468742 ) ) ;
#17312 = CARTESIAN_POINT ( 'NONE',  ( 4.523211737919912601, 7.414965188139293950, 0.9565071382433593117 ) ) ;
#17313 = CARTESIAN_POINT ( 'NONE',  ( 7.044165191775438650, 122.0728772437221323, 0.1705051815768212631 ) ) ;
#17314 = CARTESIAN_POINT ( 'NONE',  ( -5.212194349666299686, 114.7155706869413052, 1.248445758411629969 ) ) ;
#17315 = CARTESIAN_POINT ( 'NONE',  ( -56.40094345217906380, 3.567796355414390330, -1.062368598836910261 ) ) ;
#17316 = CARTESIAN_POINT ( 'NONE',  ( -2.168002701389783571, 116.2668357660312068, -0.2200461739608741141 ) ) ;
#17317 = DIRECTION ( 'NONE',  ( 5.188838149069472160E-16, -1.699382548006136559E-16, -1.000000000000000000 ) ) ;
#17318 = DIRECTION ( 'NONE',  ( -0.7071067811865467956, -0.7071067811865483499, 8.659560562354924230E-17 ) ) ;
#17319 = CARTESIAN_POINT ( 'NONE',  ( 1.868457900240731773, -15.55086107261450223, 5.421086310357070559 ) ) ;
#17320 = CARTESIAN_POINT ( 'NONE',  ( -29.81988630937914309, 58.80898419542295130, -1.270000000000005347 ) ) ;
#17321 = CARTESIAN_POINT ( 'NONE',  ( 3.617035938018385632, 9.361278981710560387, -7.607506385697127449 ) ) ;
#17322 = CARTESIAN_POINT ( 'NONE',  ( -46.91730334005650604, 25.06715201186495179, 1.923126375063701321 ) ) ;
#17323 = FACE_OUTER_BOUND ( 'NONE', #38297, .T. ) ;
#17324 = CARTESIAN_POINT ( 'NONE',  ( -58.57480556029605623, 0.6052348492003173375, 0.1017111358178618558 ) ) ;
#17325 = CARTESIAN_POINT ( 'NONE',  ( 0.01331772328568395919, 119.9741034315943864, -0.6664733318052135091 ) ) ;
#17326 = CARTESIAN_POINT ( 'NONE',  ( -23.08840689075984898, 149.5685596498530288, 0.1330139495868551958 ) ) ;
#17327 = ORIENTED_EDGE ( 'NONE', *, *, #4821, .F. ) ;
#17328 = CARTESIAN_POINT ( 'NONE',  ( -57.90853684698416259, 2.514838786807804816, -1.057718660164803538E-14 ) ) ;
#17329 = CARTESIAN_POINT ( 'NONE',  ( -6.986578011841114488, 121.9508038282781968, -0.1709446046045101919 ) ) ;
#17330 = ORIENTED_EDGE ( 'NONE', *, *, #27271, .T. ) ;
#17331 = DIRECTION ( 'NONE',  ( 6.353134868986659519E-16, -1.000000000000000000, 0.000000000000000000 ) ) ;
#17332 = CARTESIAN_POINT ( 'NONE',  ( -5.964965236245769908, 155.3820107761045790, -0.1591880423168908210 ) ) ;
#17333 = CARTESIAN_POINT ( 'NONE',  ( 2.110383923269381512, -15.54165552008020335, 5.912460941884730481 ) ) ;
#17334 = CARTESIAN_POINT ( 'NONE',  ( -14.20167894085462734, 122.0820592118662091, 1.087754808798858441 ) ) ;
#17335 = CARTESIAN_POINT ( 'NONE',  ( 20.19069946793830894, 128.9119615565081176, 0.7900021088785407208 ) ) ;
#17336 = CARTESIAN_POINT ( 'NONE',  ( 2.864695407350143164, 156.1076416471755977, 0.1877241569260537923 ) ) ;
#17337 = CARTESIAN_POINT ( 'NONE',  ( -31.49167364583235695, 53.84208496817151968, 1.269999999999994245 ) ) ;
#17338 = CARTESIAN_POINT ( 'NONE',  ( 0.9751244372034794106, -10.72340290332181567, 0.05698045496536860433 ) ) ;
#17339 = CARTESIAN_POINT ( 'NONE',  ( -23.37685013984168236, 146.7932648766621639, -0.8013420975766073484 ) ) ;
#17340 = CARTESIAN_POINT ( 'NONE',  ( -15.15189561879878433, 77.97492127061543954, -1.904999999999999583 ) ) ;
#17341 = CARTESIAN_POINT ( 'NONE',  ( 4.756814333351318425, 117.4032681585794791, 1.206529664789174339 ) ) ;
#17342 = VERTEX_POINT ( 'NONE', #18387 ) ;
#17343 = CARTESIAN_POINT ( 'NONE',  ( -5.553480690675685949, 116.8696988207415899, 0.2846251051479010696 ) ) ;
#17344 = CARTESIAN_POINT ( 'NONE',  ( -11.41761608106104475, 123.3954635094115702, 1.178011644471332442 ) ) ;
#17345 = CARTESIAN_POINT ( 'NONE',  ( -57.75430734548803002, 1.036090420344400798, -1.147874199045983312 ) ) ;
#17346 = CARTESIAN_POINT ( 'NONE',  ( 20.70190595857150129, 149.9184980045912425, 2.291194810033231111 ) ) ;
#17347 = CARTESIAN_POINT ( 'NONE',  ( 12.27894764211867695, 122.3148578561100948, -1.306772475271723799 ) ) ;
#17348 = CARTESIAN_POINT ( 'NONE',  ( -0.9608913863540493594, -11.74124177384809542, -0.1559992898937096195 ) ) ;
#17349 = CARTESIAN_POINT ( 'NONE',  ( -16.48954130525400075, 125.2933801378020888, -1.785035858276808884 ) ) ;
#17350 = CARTESIAN_POINT ( 'NONE',  ( -45.39816439898302036, 21.06106408185672763, -4.080402960186392036 ) ) ;
#17351 = CARTESIAN_POINT ( 'NONE',  ( -3.223859242259529356, 50.63946620154572997, 1.416295642791933984 ) ) ;
#17352 = CARTESIAN_POINT ( 'NONE',  ( 9.244484035386456355, 123.0263237342149978, -0.6646791600263457500 ) ) ;
#17353 = CARTESIAN_POINT ( 'NONE',  ( -4.911102353720303348, 117.7098496952192477, 0.7294018754363704726 ) ) ;
#17354 = AXIS2_PLACEMENT_3D ( 'NONE', #1164, #27129, #20509 ) ;
#17355 = ORIENTED_EDGE ( 'NONE', *, *, #21467, .F. ) ;
#17356 = CARTESIAN_POINT ( 'NONE',  ( -6.586386431196567415, 120.2999964176511014, -1.183541128842728662 ) ) ;
#17357 = CARTESIAN_POINT ( 'NONE',  ( 4.827739681024636909, -15.50696398224166117, 1.464145260785405522 ) ) ;
#17358 = DIRECTION ( 'NONE',  ( -0.8745520943968241312, 0.4849315768086548406, -5.691349986800536046E-16 ) ) ;
#17359 = CARTESIAN_POINT ( 'NONE',  ( -4.509696226152874132, 118.1210427847854163, -0.6597157338689267903 ) ) ;
#17360 = EDGE_CURVE ( 'NONE', #23764, #5065, #38800, .T. ) ;
#17361 = CARTESIAN_POINT ( 'NONE',  ( -56.65231406860745977, 4.194353530936431262, -2.518504496425251205 ) ) ;
#17362 = CARTESIAN_POINT ( 'NONE',  ( 4.113055949110636433, 118.2429491485453354, 0.3449990421833045162 ) ) ;
#17363 = CARTESIAN_POINT ( 'NONE',  ( 16.91058881216872223, 149.6223975874448229, 2.301385465272872910 ) ) ;
#17364 = CARTESIAN_POINT ( 'NONE',  ( -5.212520885064538589, 31.45212241211192605, -0.4657032193360505778 ) ) ;
#17365 = CARTESIAN_POINT ( 'NONE',  ( 8.078287538471617069, 158.6595088495342338, 0.1614234102745199240 ) ) ;
#17366 = CARTESIAN_POINT ( 'NONE',  ( -7.328769482851726025, 13.23335216599729947, 4.212906450523355772 ) ) ;
#17367 = CARTESIAN_POINT ( 'NONE',  ( 15.38106487260171562, 148.0444422243178337, 0.8962548396073237722 ) ) ;
#17368 = CARTESIAN_POINT ( 'NONE',  ( 16.34457059127843692, 122.7783120765077030, -0.5554794724330635036 ) ) ;
#17369 = DIRECTION ( 'NONE',  ( -0.8745520943968240202, 0.4849315768086551737, -5.361993529360572958E-16 ) ) ;
#17370 = DIRECTION ( 'NONE',  ( 1.011795553208986377E-16, 1.000000000000000000, -0.000000000000000000 ) ) ;
#17371 = CARTESIAN_POINT ( 'NONE',  ( -58.11144429832071268, 0.1746852717545849254, 0.04262357901407949623 ) ) ;
#17372 = CARTESIAN_POINT ( 'NONE',  ( -5.789608264049685538, 116.9447284183608389, -0.03249775470882597384 ) ) ;
#17373 = AXIS2_PLACEMENT_3D ( 'NONE', #2104, #21243, #14857 ) ;
#17374 = ORIENTED_EDGE ( 'NONE', *, *, #20419, .T. ) ;
#17375 = CARTESIAN_POINT ( 'NONE',  ( -47.08352113710599696, 24.38425570713750190, -2.219725161937593949 ) ) ;
#17376 = CARTESIAN_POINT ( 'NONE',  ( 6.649258020143044234, 120.6764540553069196, -0.8254125331649241337 ) ) ;
#17377 = CARTESIAN_POINT ( 'NONE',  ( -46.60530155212504866, 26.17382724835478314, -1.524000000000014454 ) ) ;
#17378 = ORIENTED_EDGE ( 'NONE', *, *, #86, .F. ) ;
#17379 = CARTESIAN_POINT ( 'NONE',  ( -5.332935397695337087, 104.6144662015457243, -0.1065647409268298818 ) ) ;
#17380 = CARTESIAN_POINT ( 'NONE',  ( -9.821648630411685232, 124.8790005272986861, -0.5336917924355369935 ) ) ;
#17381 = CARTESIAN_POINT ( 'NONE',  ( 5.004296470405577679, -11.88282826624689825, 0.9770688040177184508 ) ) ;
#17382 = CARTESIAN_POINT ( 'NONE',  ( -3.000642688540978487, 117.3922842568077698, 0.5420849065376541764 ) ) ;
#17383 = FACE_OUTER_BOUND ( 'NONE', #4370, .T. ) ;
#17384 = CARTESIAN_POINT ( 'NONE',  ( 22.83278390340148789, 150.4073064562084880, 0.5330863269314419783 ) ) ;
#17385 = EDGE_LOOP ( 'NONE', ( #19918, #6796 ) ) ;
#17386 = CARTESIAN_POINT ( 'NONE',  ( 3.895047602890354010, -2.730319773039217690, 2.488009491782988469 ) ) ;
#17387 = CARTESIAN_POINT ( 'NONE',  ( 0.0002511744760183973928, 116.4254662015457171, -0.01256979787922174636 ) ) ;
#17388 = CARTESIAN_POINT ( 'NONE',  ( 13.85159022459153988, 16.51000000000000156, 5.016499999999999737 ) ) ;
#17389 = DIRECTION ( 'NONE',  ( 1.000000000000000000, 0.000000000000000000, -0.000000000000000000 ) ) ;
#17390 = ORIENTED_EDGE ( 'NONE', *, *, #14746, .F. ) ;
#17391 = CARTESIAN_POINT ( 'NONE',  ( -8.137098263763151706, 121.0228228821670911, 1.007425014759447013 ) ) ;
#17392 = CARTESIAN_POINT ( 'NONE',  ( 1.861163356255745915, -7.643417679262992870, 4.233688895527200735 ) ) ;
#17393 = CARTESIAN_POINT ( 'NONE',  ( 1.049200951577147878, 117.3444111807523882, 0.5008604537731423667 ) ) ;
#17394 = CARTESIAN_POINT ( 'NONE',  ( -47.84756666395259117, 19.38928433903615911, -5.209054514891951371 ) ) ;
#17395 = CARTESIAN_POINT ( 'NONE',  ( 3.150705211532580652, 118.1710492231644736, -0.7255832847742738068 ) ) ;
#17396 = CARTESIAN_POINT ( 'NONE',  ( 4.406646451516359697, -6.344046434980911364, 1.391598188203984288 ) ) ;
#17397 = CARTESIAN_POINT ( 'NONE',  ( -17.90421410101181721, 154.0540368679750998, -1.594113676345344732 ) ) ;
#17398 = ORIENTED_EDGE ( 'NONE', *, *, #32894, .T. ) ;
#17399 = CARTESIAN_POINT ( 'NONE',  ( -9.115521395012626371, 123.9337093609977529, 0.04715588286475777546 ) ) ;
#17400 = CARTESIAN_POINT ( 'NONE',  ( 3.037190435423921642, -15.45437603076259236, 5.639675387367293347 ) ) ;
#17401 = CARTESIAN_POINT ( 'NONE',  ( -46.33290834485666920, 20.59977736898131440, 4.631597800898110684 ) ) ;
#17402 = CARTESIAN_POINT ( 'NONE',  ( -0.3314327031344502239, 118.1651004622152783, -0.8947675711121312325 ) ) ;
#17404 = VERTEX_POINT ( 'NONE', #23046 ) ;
#17403 = VECTOR ( 'NONE', #41857, 1000.000000000000227 ) ;
#17405 = CARTESIAN_POINT ( 'NONE',  ( 12.24350972434449147, 123.0735437985678971, 1.806721486477698591 ) ) ;
#17406 = DIRECTION ( 'NONE',  ( 0.9998004120163609398, 0.000000000000000000, 0.01997839162482749689 ) ) ;
#17407 = CARTESIAN_POINT ( 'NONE',  ( -6.515206564940426254E-14, 69.43546620154573645, -8.744632320494937509E-18 ) ) ;
#17408 = CARTESIAN_POINT ( 'NONE',  ( -8.102197167285096313, 117.9965348323767671, 0.5618759090088268904 ) ) ;
#17409 = CARTESIAN_POINT ( 'NONE',  ( -6.209159877377784298, 7.473591768893033560, -5.687189600455027971 ) ) ;
#17410 = CARTESIAN_POINT ( 'NONE',  ( 15.67318563778015061, 143.6801599334541208, 1.294273616026768492 ) ) ;
#17411 = CARTESIAN_POINT ( 'NONE',  ( -25.97603047661466036, 74.27059221564131519, -1.270000000000005791 ) ) ;
#17412 = CARTESIAN_POINT ( 'NONE',  ( 22.94521658075144188, 142.4877946823990271, -0.4044642804735132380 ) ) ;
#17413 = CARTESIAN_POINT ( 'NONE',  ( -29.82321757229076908, 71.17901112636586447, 1.269999999999991802 ) ) ;
#17414 = CARTESIAN_POINT ( 'NONE',  ( -57.16753566998470859, 2.297090730223299904, 1.678507472752695184 ) ) ;
#17415 = FILL_AREA_STYLE ('',( #34459 ) ) ;
#17416 = CARTESIAN_POINT ( 'NONE',  ( -58.09657527255103560, 0.9821181129459344294, 1.359330230256424521 ) ) ;
#17417 = CARTESIAN_POINT ( 'NONE',  ( -58.59008072161548597, -0.2123309539291723391, 0.4862672643680832629 ) ) ;
#17418 = CARTESIAN_POINT ( 'NONE',  ( -4.514281675679005623, 118.1172348940403367, 0.5455092187523593594 ) ) ;
#17419 = CARTESIAN_POINT ( 'NONE',  ( 2.730790556997842788, 107.1172351171862118, -4.574511410390974753 ) ) ;
#17420 = VERTEX_POINT ( 'NONE', #29246 ) ;
#17421 = CARTESIAN_POINT ( 'NONE',  ( -47.16890147375937659, 22.20336809214646578, 4.187060126831876339 ) ) ;
#17422 = CARTESIAN_POINT ( 'NONE',  ( 6.160900166467479622, 119.5651146182915738, -1.008937348957311242 ) ) ;
#17423 = CARTESIAN_POINT ( 'NONE',  ( -5.229314312453288593, 116.0897965414613964, -1.239798673375258842 ) ) ;
#17424 = CARTESIAN_POINT ( 'NONE',  ( 4.638744064954714474, 118.0266105220047024, 0.7608683655302644899 ) ) ;
#17425 = CARTESIAN_POINT ( 'NONE',  ( -10.86813797462349740, 153.1125297277760069, -1.236783938685797279 ) ) ;
#17426 = CARTESIAN_POINT ( 'NONE',  ( -0.6181410509038570700, 115.7031374082930455, -1.759523019197690274 ) ) ;
#17427 = CARTESIAN_POINT ( 'NONE',  ( 0.5464446624898103844, 117.9496048909628456, -1.385902395265538267 ) ) ;
#17428 = VECTOR ( 'NONE', #1485, 1000.000000000000000 ) ;
#17429 = CARTESIAN_POINT ( 'NONE',  ( -3.685501180670149424, 30.72893705507438611, -2.802369389919810772 ) ) ;
#17430 = CARTESIAN_POINT ( 'NONE',  ( -5.849275934571582347, 120.8872308857076519, -0.8185814695607154245 ) ) ;
#17431 = CARTESIAN_POINT ( 'NONE',  ( 4.678875543802746506, 116.0444662015457737, -3.608683038041131663 ) ) ;
#17432 = CARTESIAN_POINT ( 'NONE',  ( -47.72737885966184024, 19.53144537861849273, 5.204668046378070123 ) ) ;
#17433 = CARTESIAN_POINT ( 'NONE',  ( 8.764399874728660222, 117.8902759020840563, -0.3181776094565843538 ) ) ;
#17434 = CARTESIAN_POINT ( 'NONE',  ( -4.633229131069707130, 121.2001890545385976, 0.01432855803707623957 ) ) ;
#17435 = TOROIDAL_SURFACE ( 'NONE', #41263, 14.09699999999999420, 0.6350000000000000089 ) ;
#17436 = DIRECTION ( 'NONE',  ( 0.4849315768086535638, 0.8745520943968251304, 1.030032898892975065E-16 ) ) ;
#17437 = CARTESIAN_POINT ( 'NONE',  ( 19.64956762203114593, 128.7577553591919752, 1.229466013835583738 ) ) ;
#17438 = CARTESIAN_POINT ( 'NONE',  ( 11.65115770210962687, 16.51000000000000156, 4.908176479697702099 ) ) ;
#17439 = CARTESIAN_POINT ( 'NONE',  ( 3.263309282894114371, -14.66069363451780205, 2.445366243406764006 ) ) ;
#17440 = CARTESIAN_POINT ( 'NONE',  ( -16.81178602683906220, 135.2943057719725459, 1.678525023343173661 ) ) ;
#17441 = CARTESIAN_POINT ( 'NONE',  ( -0.3089908097382615959, -9.589635095254870123, 0.9269408180416041088 ) ) ;
#17442 = CARTESIAN_POINT ( 'NONE',  ( 0.009748065369120871224, 159.5507987164374981, -0.4878330526048096361 ) ) ;
#17443 = CARTESIAN_POINT ( 'NONE',  ( -0.8611515851325071136, 16.54815110656625166, -0.4551624184793268135 ) ) ;
#17444 = VERTEX_POINT ( 'NONE', #13274 ) ;
#17445 = CARTESIAN_POINT ( 'NONE',  ( -49.74050263075070433, 15.22813595918496432, 2.996737790144726965 ) ) ;
#17446 = CARTESIAN_POINT ( 'NONE',  ( 5.733418603097385713, 118.4539739381501988, 0.6622650514401648980 ) ) ;
#17447 = CARTESIAN_POINT ( 'NONE',  ( -14.68012063964734004, 139.2174805014774392, 0.5696158742132094721 ) ) ;
#17448 = CARTESIAN_POINT ( 'NONE',  ( 2.226119369219526689, -15.10343733042141068, 5.886803469647748699 ) ) ;
#17449 = CARTESIAN_POINT ( 'NONE',  ( 17.30559516374531626, 146.8699245690979751, -1.364999074652126110 ) ) ;
#17450 = ORIENTED_EDGE ( 'NONE', *, *, #3677, .T. ) ;
#17451 = CARTESIAN_POINT ( 'NONE',  ( -10.57181108402536829, 155.7851685111067184, -2.170362527570921962 ) ) ;
#17452 = CARTESIAN_POINT ( 'NONE',  ( 2.500242650891530971, 104.6144662015457527, 4.137678032133335293 ) ) ;
#17453 = ADVANCED_FACE ( 'NONE', ( #29675 ), #6843, .F. ) ;
#17454 = CARTESIAN_POINT ( 'NONE',  ( 3.134184212546501591, -13.48855807073397273, 1.578073873303884156 ) ) ;
#17455 = CARTESIAN_POINT ( 'NONE',  ( -4.942124793971827579, 117.4083539704047183, -1.067544502694063979 ) ) ;
#17456 = ADVANCED_FACE ( 'NONE', ( #19445 ), #29276, .T. ) ;
#17457 = CARTESIAN_POINT ( 'NONE',  ( 9.007539097974285980, 123.9742709865185191, 0.1460878630902627262 ) ) ;
#17458 = ORIENTED_EDGE ( 'NONE', *, *, #10202, .F. ) ;
#17459 = CARTESIAN_POINT ( 'NONE',  ( 13.40750253236522127, 122.4565580348552913, 1.800089891214285531 ) ) ;
#17460 = CARTESIAN_POINT ( 'NONE',  ( 2.321315766260381608, 107.3040393085556445, 4.704548974857680754 ) ) ;
#17461 =( BOUNDED_CURVE ( )  B_SPLINE_CURVE ( 1, ( #18474, #5733 ),
 .UNSPECIFIED., .F., .T. ) 
 B_SPLINE_CURVE_WITH_KNOTS ( ( 2, 2 ),
 ( 0.04437134223310085224, 0.9700710138315444819 ),
 .UNSPECIFIED. ) 
 CURVE ( )  GEOMETRIC_REPRESENTATION_ITEM ( )  RATIONAL_B_SPLINE_CURVE ( ( 0.9983552002448072837, 0.9999484871150284837 ) ) 
 REPRESENTATION_ITEM ( '' )  );
#17462 = AXIS2_PLACEMENT_3D ( 'NONE', #24629, #8040, #21013 ) ;
#17463 = LINE ( 'NONE', #33884, #24550 ) ;
#17464 = DIRECTION ( 'NONE',  ( 0.9998501190848635423, 0.01731298258487451447, 5.158639060800523934E-16 ) ) ;
#17465 = CARTESIAN_POINT ( 'NONE',  ( 8.048392397359023676, 158.6767594643193604, -0.003330354478298842586 ) ) ;
#17466 = DIRECTION ( 'NONE',  ( -1.000000000000000000, 1.893378931774809890E-16, 0.000000000000000000 ) ) ;
#17467 = CARTESIAN_POINT ( 'NONE',  ( 1.667695940653114883, -15.52399890817349259, 5.699764172519937055 ) ) ;
#17468 = CARTESIAN_POINT ( 'NONE',  ( 18.35410564743290607, 77.35382415001784295, 5.016499999999999737 ) ) ;
#17469 = CARTESIAN_POINT ( 'NONE',  ( 2.912792906754999134, 38.59631781016217644, -1.173005823891349220 ) ) ;
#17470 = CARTESIAN_POINT ( 'NONE',  ( 1.154696340448265524, 118.0995038195805904, 0.6495305470935905934 ) ) ;
#17471 = VERTEX_POINT ( 'NONE', #10497 ) ;
#17472 = CARTESIAN_POINT ( 'NONE',  ( 8.403146708066456583, 17.13307930518084632, 0.5673920214783956251 ) ) ;
#17473 = CARTESIAN_POINT ( 'NONE',  ( -2.367130307693360081, 117.2935156952702016, -0.6933524696228330342 ) ) ;
#17474 = CARTESIAN_POINT ( 'NONE',  ( -3.776803835208340843, 121.1194860566822626, -0.3725146398702259276 ) ) ;
#17475 = LINE ( 'NONE', #688, #12814 ) ;
#17476 = CARTESIAN_POINT ( 'NONE',  ( -4.703828842912097130, 114.7515309228077030, -1.852197097316329311 ) ) ;
#17477 = CARTESIAN_POINT ( 'NONE',  ( -0.005880675322317568607, 122.2435587914035295, 0.2942930402745070340 ) ) ;
#17478 = CIRCLE ( 'NONE', #31753, 0.3810000000000000053 ) ;
#17479 = CARTESIAN_POINT ( 'NONE',  ( 2.801506786573456420, 9.139157206818806500, -3.684590140147142368 ) ) ;
#17480 = DIRECTION ( 'NONE',  ( 5.188838149069472160E-16, -1.699382548006136559E-16, -1.000000000000000000 ) ) ;
#17481 = CARTESIAN_POINT ( 'NONE',  ( -5.177913976931285411, 57.14999999999999858, -5.372100000000001430 ) ) ;
#17482 = CARTESIAN_POINT ( 'NONE',  ( 3.334874478900925254, -13.11215654211414439, 1.739483084651320066 ) ) ;
#17483 = EDGE_CURVE ( 'NONE', #35734, #14389, #22264, .T. ) ;
#17484 = CARTESIAN_POINT ( 'NONE',  ( 4.141015252736647057, 122.5143120247930142, -0.07252455213604046269 ) ) ;
#17485 = CARTESIAN_POINT ( 'NONE',  ( 0.6408964823745235684, 37.72669835237458358, 1.782185992127281793 ) ) ;
#17486 = DIRECTION ( 'NONE',  ( -0.6559537821943239866, 0.7548010569845283735, -4.686333752532408853E-16 ) ) ;
#17487 = CIRCLE ( 'NONE', #22908, 7.461249999999999716 ) ;
#17488 = VERTEX_POINT ( 'NONE', #6682 ) ;
#17489 = CARTESIAN_POINT ( 'NONE',  ( -4.831300404072987220, 104.6144662015457811, -0.2179056330698100619 ) ) ;
#17490 = CARTESIAN_POINT ( 'NONE',  ( 1.930844028328122519, -15.65960119559217745, 5.531553210582124791 ) ) ;
#17491 = CARTESIAN_POINT ( 'NONE',  ( -19.68629672748976489, 145.2539617268756729, 1.742627101631720077 ) ) ;
#17492 = CARTESIAN_POINT ( 'NONE',  ( 0.6989348986720191892, -4.029744825116962303, 4.573446973323917142 ) ) ;
#17493 = VERTEX_POINT ( 'NONE', #3710 ) ;
#17494 = ORIENTED_EDGE ( 'NONE', *, *, #37363, .T. ) ;
#17495 = CYLINDRICAL_SURFACE ( 'NONE', #1509, 13.46199999999999619 ) ;
#17496 = CARTESIAN_POINT ( 'NONE',  ( 0.3557171951617904004, 107.2171362991012842, 4.792661424475801901 ) ) ;
#17497 = CARTESIAN_POINT ( 'NONE',  ( -9.956456675072866247, 154.0333045108203009, 1.106646445589350325 ) ) ;
#17498 = CARTESIAN_POINT ( 'NONE',  ( -45.22172581742046304, 21.28617977371392200, 3.835562958556399504 ) ) ;
#17499 = CARTESIAN_POINT ( 'NONE',  ( 15.87040186760622262, 150.9007765090757971, -1.629155861667390681 ) ) ;
#17500 = CARTESIAN_POINT ( 'NONE',  ( -20.64857576366725667, 148.2641884961211076, -2.442776014760721370 ) ) ;
#17501 = DIRECTION ( 'NONE',  ( -0.8745520943968235761, 0.4849315768086558953, -5.361993529360570985E-16 ) ) ;
#17502 = ADVANCED_FACE ( 'NONE', ( #19648 ), #26259, .T. ) ;
#17503 = CARTESIAN_POINT ( 'NONE',  ( 4.280713456108180992, 118.2124846597233869, -0.3641107394327984803 ) ) ;
#17504 = CARTESIAN_POINT ( 'NONE',  ( 0.6165924928997299492, 120.7136710450757988, -0.2143668442300579458 ) ) ;
#17505 = EDGE_LOOP ( 'NONE', ( #22181, #33300, #21912, #8337, #3161, #36174, #35558, #7535 ) ) ;
#17506 = CARTESIAN_POINT ( 'NONE',  ( 3.392805262616394035, -14.86080682751021698, 1.607197643132475040 ) ) ;
#17507 = DIRECTION ( 'NONE',  ( 0.7770581983690896255, -0.6294287539883961502, 6.584108293994711875E-16 ) ) ;
#17508 = AXIS2_PLACEMENT_3D ( 'NONE', #8601, #21564, #34592 ) ;
#17509 = CARTESIAN_POINT ( 'NONE',  ( -58.22800107110067103, 0.01111325675227925469, 0.5047451677687325722 ) ) ;
#17510 = ADVANCED_FACE ( 'NONE', ( #39268 ), #13490, .F. ) ;
#17511 = CARTESIAN_POINT ( 'NONE',  ( 4.099978103716023448, 4.450953565018914482, -2.131961072590273343 ) ) ;
#17512 = CARTESIAN_POINT ( 'NONE',  ( 10.56433624517442738, 123.7931190674884050, 1.348085882050163553 ) ) ;
#17513 = CARTESIAN_POINT ( 'NONE',  ( -1.879194370357706756, 31.42354579518680424, 3.981814511614890417 ) ) ;
#17514 = CARTESIAN_POINT ( 'NONE',  ( -6.279970060868473425, 120.0898888515776264, 0.2014705954985339942 ) ) ;
#17515 = CARTESIAN_POINT ( 'NONE',  ( 2.801506786573456420, 9.139157206818806500, -3.684590140147142368 ) ) ;
#17516 = CARTESIAN_POINT ( 'NONE',  ( 11.84172335778361251, 151.9972573545839225, 0.3576891575424543945 ) ) ;
#17517 = DIRECTION ( 'NONE',  ( -0.8745520943968241312, 0.4849315768086548406, -5.691349986800536046E-16 ) ) ;
#17518 = CARTESIAN_POINT ( 'NONE',  ( -50.60903162571948855, 13.45680032611325849, -2.107060282091948622 ) ) ;
#17519 = CARTESIAN_POINT ( 'NONE',  ( 2.168201787175106698, 116.3152343823800265, -0.1794994579355096709 ) ) ;
#17520 = CARTESIAN_POINT ( 'NONE',  ( 0.002462548249238089102, 123.7646714092002611, -0.1232359841710924941 ) ) ;
#17521 = CARTESIAN_POINT ( 'NONE',  ( -46.90670141593995623, 25.33105981158402642, -1.751001814892826580 ) ) ;
#17522 = CARTESIAN_POINT ( 'NONE',  ( -2.005270804404902574, 106.7492432543866130, 4.871661368785221491 ) ) ;
#17523 = CARTESIAN_POINT ( 'NONE',  ( -29.02482657614628536, 65.73348897311412031, -1.524000000000005350 ) ) ;
#17524 = CARTESIAN_POINT ( 'NONE',  ( -6.252972126910993467, 3.963778981710710969, 5.644239715445565686 ) ) ;
#17525 = CARTESIAN_POINT ( 'NONE',  ( -17.14500000000466784, 71.11999999999886768, -1.270000000000000684 ) ) ;
#17526 = DIRECTION ( 'NONE',  ( -0.5810519254489896479, -0.8138664877804110409, 0.000000000000000000 ) ) ;
#17527 = CARTESIAN_POINT ( 'NONE',  ( -58.49256177947683000, 0.7572623586737103896, 0.8868308481463905713 ) ) ;
#17528 = CARTESIAN_POINT ( 'NONE',  ( 0.0002200197269684159480, 124.8375573595198063, -0.01101068683960094302 ) ) ;
#17529 = CARTESIAN_POINT ( 'NONE',  ( -0.3220477894875805047, 116.6413645472259617, 0.1880332438949533225 ) ) ;
#17530 = ORIENTED_EDGE ( 'NONE', *, *, #16245, .T. ) ;
#17531 = CARTESIAN_POINT ( 'NONE',  ( -56.90441949580814196, 4.712873715160811550, -1.842411344577102206 ) ) ;
#17532 = CARTESIAN_POINT ( 'NONE',  ( -7.784332312133520837, 122.6279626997426533, -0.1742668636873402899 ) ) ;
#17533 = EDGE_CURVE ( 'NONE', #32851, #10071, #38134, .T. ) ;
#17534 = ORIENTED_EDGE ( 'NONE', *, *, #32590, .F. ) ;
#17535 = CARTESIAN_POINT ( 'NONE',  ( -46.96000079187034970, 20.35382130790375044, -5.064780906956246831 ) ) ;
#17536 = CARTESIAN_POINT ( 'NONE',  ( -9.501049366036612653, 124.7903798759050460, -0.1436111869418686404 ) ) ;
#17537 = CARTESIAN_POINT ( 'NONE',  ( 5.253367374056280070, -14.88852847978991356, 3.689182801501961428 ) ) ;
#17538 = CARTESIAN_POINT ( 'NONE',  ( -20.86711222142712074, 145.7124547906547889, 1.576573076165909360 ) ) ;
#17539 = CARTESIAN_POINT ( 'NONE',  ( -0.004355829920669731722, 116.7171338949676738, 0.2179835409713598571 ) ) ;
#17540 = EDGE_CURVE ( 'NONE', #35348, #16752, #36701, .T. ) ;
#17541 = CARTESIAN_POINT ( 'NONE',  ( 20.00278215841951379, 152.4248492066682559, -0.8711105393690438126 ) ) ;
#17542 = CARTESIAN_POINT ( 'NONE',  ( 14.73199999999999754, 61.59499999999999886, 5.016499999999999737 ) ) ;
#17543 = CARTESIAN_POINT ( 'NONE',  ( -23.30140632484793528, 142.7201128741078833, -0.7978754358820899784 ) ) ;
#17544 = CARTESIAN_POINT ( 'NONE',  ( -49.66173528812303317, 16.83021509124200676, -4.995230413551627002 ) ) ;
#17545 = CARTESIAN_POINT ( 'NONE',  ( -30.75918919842648336, 69.77432548395512413, -1.270000000000007567 ) ) ;
#17546 = ORIENTED_EDGE ( 'NONE', *, *, #33664, .T. ) ;
#17547 = CARTESIAN_POINT ( 'NONE',  ( -5.556907610490653404, 116.8023684160186519, 0.1994680161719879219 ) ) ;
#17548 = CARTESIAN_POINT ( 'NONE',  ( -11.30191013352091467, 123.2561760277034324, 1.170227508207775324 ) ) ;
#17549 = CARTESIAN_POINT ( 'NONE',  ( -57.76679705834290246, 1.009099809236461587, -1.134662844628306910 ) ) ;
#17550 = CARTESIAN_POINT ( 'NONE',  ( 11.12579521122935944, 121.4866960210745503, -1.254162869557706061 ) ) ;
#17551 = CARTESIAN_POINT ( 'NONE',  ( 0.7724745873405186591, -15.29971413243098688, -0.5873327843062005060 ) ) ;
#17552 = CARTESIAN_POINT ( 'NONE',  ( -6.794677088231817486, 118.4250403807481575, -1.128628347181275693 ) ) ;
#17553 = CARTESIAN_POINT ( 'NONE',  ( -48.16508968810062896, 19.01313136326716347, -5.219744232931991412 ) ) ;
#17554 = CARTESIAN_POINT ( 'NONE',  ( 14.29925251870365699, 150.3563008155378213, -0.9573768768026650333 ) ) ;
#17555 = ADVANCED_FACE ( 'NONE', ( #11332 ), #16839, .T. ) ;
#17556 = CARTESIAN_POINT ( 'NONE',  ( -11.83539255247756117, 152.0195595274622349, -0.2364993098673504601 ) ) ;
#17557 = ORIENTED_EDGE ( 'NONE', *, *, #931, .F. ) ;
#17558 = CARTESIAN_POINT ( 'NONE',  ( -13.11083847086530874, 125.9194590699508893, -1.866409529942264944 ) ) ;
#17559 = CARTESIAN_POINT ( 'NONE',  ( 2.110750219194173827, -15.67940412490098723, 5.433654451060461632 ) ) ;
#17560 = DIRECTION ( 'NONE',  ( 4.017660918040594346E-17, -1.000000000000000000, -2.376309959284834438E-19 ) ) ;
#17561 = CARTESIAN_POINT ( 'NONE',  ( -4.299846727470445273, 118.2124326582062963, -0.4976427630063417484 ) ) ;
#17562 = CARTESIAN_POINT ( 'NONE',  ( -54.47970570282438274, 8.083255770631444292, -3.476097746275910172 ) ) ;
#17563 = DIRECTION ( 'NONE',  ( -0.5149185422762211362, 0.8572391118119444542, 0.000000000000000000 ) ) ;
#17564 = CARTESIAN_POINT ( 'NONE',  ( 10.84669103489406972, 122.6724665872831679, 1.607685377936340032 ) ) ;
#17565 = DIRECTION ( 'NONE',  ( -0.9998004120163609398, 0.000000000000000000, -0.01997839162482749689 ) ) ;
#17566 = CARTESIAN_POINT ( 'NONE',  ( 4.713631738767327661, 116.7564862437112794, 0.09418957996065577265 ) ) ;
#17567 = CARTESIAN_POINT ( 'NONE',  ( -2.166771814436331045, 10.43868160547798674, -8.139002505017437272 ) ) ;
#17568 = CARTESIAN_POINT ( 'NONE',  ( 5.248704524870055010, 121.2670714900434206, 0.3264022214948026912 ) ) ;
#17569 = EDGE_CURVE ( 'NONE', #1073, #16433, #18719, .T. ) ;
#17570 = CARTESIAN_POINT ( 'NONE',  ( 19.39512251848550761, 128.7092500879292345, -0.6293422422100684033 ) ) ;
#17571 = CARTESIAN_POINT ( 'NONE',  ( -44.77556674759998856, 21.10465188057014174, -3.405155276520980934 ) ) ;
#17572 = CARTESIAN_POINT ( 'NONE',  ( 2.791705395246603327, 115.6909491485452577, 1.685629878066634113 ) ) ;
#17573 = CARTESIAN_POINT ( 'NONE',  ( -57.72731561024291125, 0.8685078910842247701, 0.07340608407945603542 ) ) ;
#17574 = CARTESIAN_POINT ( 'NONE',  ( -22.83585328881722276, 150.4073064562084880, -0.3794817294851793865 ) ) ;
#17575 = ORIENTED_EDGE ( 'NONE', *, *, #18882, .F. ) ;
#17576 = CARTESIAN_POINT ( 'NONE',  ( -47.05348687143031583, 24.98710001375500056, -1.566218509541823956 ) ) ;
#17577 = CARTESIAN_POINT ( 'NONE',  ( -5.923576811503439288, 121.3842984696033653, -0.3127082814038080194 ) ) ;
#17578 = FACE_OUTER_BOUND ( 'NONE', #27858, .T. ) ;
#17579 = ORIENTED_EDGE ( 'NONE', *, *, #17307, .F. ) ;
#17580 = CARTESIAN_POINT ( 'NONE',  ( 0.2889217817199783434, 115.7029882075844540, -1.754376360704741122 ) ) ;
#17581 = CARTESIAN_POINT ( 'NONE',  ( -8.575029486087489161, 123.3373102669514765, -0.3234659723512184337 ) ) ;
#17582 = CARTESIAN_POINT ( 'NONE',  ( 4.994336218630399671, -12.17445384341683834, 1.469335147697719890 ) ) ;
#17583 = CARTESIAN_POINT ( 'NONE',  ( -21.43028413922730024, 149.8571540977637255, 1.275288106631634832 ) ) ;
#17584 = CARTESIAN_POINT ( 'NONE',  ( 10.92199999999999704, 57.78500000000000369, 5.016499999999999737 ) ) ;
#17585 = CARTESIAN_POINT ( 'NONE',  ( 23.34655412193302837, 148.8653451956335516, 0.6207958181910346873 ) ) ;
#17586 = EDGE_CURVE ( 'NONE', #5717, #30054, #32021, .T. ) ;
#17587 = ORIENTED_EDGE ( 'NONE', *, *, #35079, .T. ) ;
#17588 = CARTESIAN_POINT ( 'NONE',  ( 4.349802767100347189, -10.92635770930747796, -1.576909098649299512 ) ) ;
#17589 = CARTESIAN_POINT ( 'NONE',  ( -3.302029177305334073, 159.4671159221996959, -0.06598240135525369754 ) ) ;
#17590 = CARTESIAN_POINT ( 'NONE',  ( -6.707568152035292797E-14, 117.3144662015457271, 2.632902133564923224E-18 ) ) ;
#17591 = DIRECTION ( 'NONE',  ( -0.7308269722843310223, 0.6825627711659330021, -4.952078135395968077E-16 ) ) ;
#17592 = ADVANCED_FACE ( 'NONE', ( #14304 ), #23140, .T. ) ;
#17593 = ORIENTED_EDGE ( 'NONE', *, *, #2212, .F. ) ;
#17594 = CARTESIAN_POINT ( 'NONE',  ( 8.208067840267224469, 120.4389322928407324, 1.432930303473133993 ) ) ;
#17595 = CARTESIAN_POINT ( 'NONE',  ( -4.434453077421578904, -10.21728329253013179, 1.368390957472948921 ) ) ;
#17596 = CARTESIAN_POINT ( 'NONE',  ( 21.87689675406251411, 150.0588410196355937, 1.874897916013938737 ) ) ;
#17597 = CARTESIAN_POINT ( 'NONE',  ( -52.86182053368817435, 11.13604294809218587, -4.079049242077941173 ) ) ;
#17598 = CARTESIAN_POINT ( 'NONE',  ( 20.72967856921734864, 148.2641884961211076, -1.615940018417327373 ) ) ;
#17599 = CARTESIAN_POINT ( 'NONE',  ( -4.598078022480850180, -10.86695742004451404, -0.5832510952623800593 ) ) ;
#17600 = CARTESIAN_POINT ( 'NONE',  ( -14.71083544318262071, 121.0688405154646858, -1.213083844406487977 ) ) ;
#17601 = ORIENTED_EDGE ( 'NONE', *, *, #41067, .F. ) ;
#17602 = ORIENTED_EDGE ( 'NONE', *, *, #38480, .T. ) ;
#17603 = CARTESIAN_POINT ( 'NONE',  ( -11.97065782033005554, 130.4318746828361100, -0.03484989721007628743 ) ) ;
#17605 = CARTESIAN_POINT ( 'NONE',  ( 4.211475536325941071, -15.04083557003654903, 4.983330352733777779 ) ) ;
#17604 = VECTOR ( 'NONE', #4419, 1000.000000000000000 ) ;
#17606 = AXIS2_PLACEMENT_3D ( 'NONE', #41027, #5460, #18420 ) ;
#17607 = FACE_OUTER_BOUND ( 'NONE', #19375, .T. ) ;
#17608 = CARTESIAN_POINT ( 'NONE',  ( -0.4814620969468332845, 118.1651003975972998, -0.8929907497847521247 ) ) ;
#17609 = ORIENTED_EDGE ( 'NONE', *, *, #21467, .T. ) ;
#17610 = CARTESIAN_POINT ( 'NONE',  ( 9.741115574333344185, 120.9522862504114897, 1.586783935194494788 ) ) ;
#17611 = DIRECTION ( 'NONE',  ( 6.146657985744592735E-16, 3.905054717696927382E-31, 1.000000000000000000 ) ) ;
#17612 = DIRECTION ( 'NONE',  ( 0.9998004120163608288, 0.000000000000000000, 0.01997839162482749342 ) ) ;
#17613 = CARTESIAN_POINT ( 'NONE',  ( -14.55782549726419894, 156.0472725025049954, 0.8788902920476678871 ) ) ;
#17614 = CARTESIAN_POINT ( 'NONE',  ( -4.386519595447357922, 0.5779702600499575516, 7.231359419481246498 ) ) ;
#17615 = CARTESIAN_POINT ( 'NONE',  ( 12.64766777886143068, 130.7634385742845780, 1.140803344710751510 ) ) ;
#17616 = DIRECTION ( 'NONE',  ( -0.1715592850456333085, 0.1224830539174543292, 0.9775302108976914317 ) ) ;
#17617 = CARTESIAN_POINT ( 'NONE',  ( 13.30049347609353561, 119.7426348059052685, -0.3046699512218788430 ) ) ;
#17618 = FACE_OUTER_BOUND ( 'NONE', #31755, .T. ) ;
#17619 = CARTESIAN_POINT ( 'NONE',  ( -53.64375852056468830, 9.525086444836489363, 3.607221310910125656 ) ) ;
#17620 = CARTESIAN_POINT ( 'NONE',  ( -6.484670282503085616E-14, 71.97546620154574271, 3.533028205012241021E-29 ) ) ;
#17622 = CARTESIAN_POINT ( 'NONE',  ( -58.07447437077728125, 1.735896131820596766, 1.499107834811089113 ) ) ;
#17621 = B_SPLINE_CURVE_WITH_KNOTS ( 'NONE', 3,
 ( #31038, #37650, #8475, #34666 ),
 .UNSPECIFIED., .F., .F.,
 ( 4, 4 ),
 ( 0.02831029896240370991, 1.000000000000000000 ),
 .UNSPECIFIED. ) ;
#17623 = CARTESIAN_POINT ( 'NONE',  ( -58.65177056075324202, -0.3162497232223037136, 0.3274186093513313800 ) ) ;
#17624 = CARTESIAN_POINT ( 'NONE',  ( -4.158059140961544387, 118.2391353841180432, 0.2335865895784110802 ) ) ;
#17625 = LINE ( 'NONE', #40649, #3660 ) ;
#17626 = EDGE_LOOP ( 'NONE', ( #12875, #40411, #28350, #12941 ) ) ;
#17627 = CARTESIAN_POINT ( 'NONE',  ( -47.35944255389382818, 21.37623662739424191, 4.722871667523163453 ) ) ;
#17628 = AXIS2_PLACEMENT_3D ( 'NONE', #34637, #25038, #38041 ) ;
#17629 = CARTESIAN_POINT ( 'NONE',  ( -8.253346482873464396, 120.2166765077018340, -1.447820397028310779 ) ) ;
#17630 = AXIS2_PLACEMENT_3D ( 'NONE', #5561, #31738, #41552 ) ;
#17631 = CARTESIAN_POINT ( 'NONE',  ( -4.762298162519812195, 112.7561542417671916, -2.571201254457596175 ) ) ;
#17632 = CARTESIAN_POINT ( 'NONE',  ( 4.233096343644137782, 118.2249610142085032, 0.4811101450830501669 ) ) ;
#17633 = CARTESIAN_POINT ( 'NONE',  ( -15.67318563778028206, 143.6801599334541208, -1.294273616026768270 ) ) ;
#17634 = CARTESIAN_POINT ( 'NONE',  ( 0.6048459695572244721, 117.3993834314627236, -1.469644289381657254 ) ) ;
#17635 = ORIENTED_EDGE ( 'NONE', *, *, #40447, .T. ) ;
#17636 = CARTESIAN_POINT ( 'NONE',  ( 0.1065646865914872399, 105.8844662015456777, -5.332932678536313809 ) ) ;
#17637 = CARTESIAN_POINT ( 'NONE',  ( -3.381852828898228136, 156.3978305292817481, -1.289121224278521938 ) ) ;
#17638 = CARTESIAN_POINT ( 'NONE',  ( -0.1561264326628848120, 116.0444662015457027, 6.158975241439932802 ) ) ;
#17639 = CARTESIAN_POINT ( 'NONE',  ( -47.85244527695894590, 19.39403540832958583, 5.219971639306684175 ) ) ;
#17640 = CARTESIAN_POINT ( 'NONE',  ( 13.46199999999999619, 17.14499999999999957, 1.648619521012166171E-15 ) ) ;
#17641 = CARTESIAN_POINT ( 'NONE',  ( -15.76305951754530099, 145.8995318477080332, -0.1132554252373959985 ) ) ;
#17642 = DIRECTION ( 'NONE',  ( 0.000000000000000000, 0.000000000000000000, -1.000000000000000000 ) ) ;
#17643 = CARTESIAN_POINT ( 'NONE',  ( 11.33669861507955190, 118.9804978796424706, 0.9069902030348427902 ) ) ;
#17644 = DIRECTION ( 'NONE',  ( -0.4849315768086480127, -0.8745520943968279060, -1.030032898892941415E-16 ) ) ;
#17646 = CARTESIAN_POINT ( 'NONE',  ( 21.43028413922716879, 149.8571540977637255, -1.275288106631634610 ) ) ;
#17645 = CARTESIAN_POINT ( 'NONE',  ( 2.667920334613889555, -13.82128762729334426, -0.01087480101406306660 ) ) ;
#17647 = CARTESIAN_POINT ( 'NONE',  ( -0.9814465556261140478, 157.4778559999684830, 1.561959177316862180 ) ) ;
#17648 = CARTESIAN_POINT ( 'NONE',  ( -0.9543378889979354796, -1.596235181177088291, 0.1924800533990675688 ) ) ;
#17649 = CARTESIAN_POINT ( 'NONE',  ( 0.005431400947611031600, 116.8580640273661118, -0.2718095133625907933 ) ) ;
#17650 = CARTESIAN_POINT ( 'NONE',  ( 0.9751022921854990422, 22.16746322748675624, -0.05045228706074462999 ) ) ;
#17651 = ORIENTED_EDGE ( 'NONE', *, *, #5123, .T. ) ;
#17652 = CARTESIAN_POINT ( 'NONE',  ( -49.01239152747368166, 15.29178156536908872, 1.600675721865261858 ) ) ;
#17653 = ITEM_DEFINED_TRANSFORMATION ( 'NONE', 'NONE', #12108,  #3275 ) ;
#17654 = CARTESIAN_POINT ( 'NONE',  ( -11.75634259954081529, 128.3321206738457647, 0.5010001888332091813 ) ) ;
#17655 = CARTESIAN_POINT ( 'NONE',  ( 2.069070256058832324, -15.20480250118845511, 5.930115229603830862 ) ) ;
#17656 = CARTESIAN_POINT ( 'NONE',  ( 0.5698427240850039155, 120.0661220204379305, -0.4260729765348976184 ) ) ;
#17657 = ORIENTED_EDGE ( 'NONE', *, *, #9963, .T. ) ;
#17658 = DIRECTION ( 'NONE',  ( -4.017660918040594346E-17, 1.000000000000000000, 2.376309959284834438E-19 ) ) ;
#17659 = CARTESIAN_POINT ( 'NONE',  ( 3.394644278243977187, -13.41358914320520057, 2.304069835958892032 ) ) ;
#17660 = CARTESIAN_POINT ( 'NONE',  ( -5.176850267262477878, 31.60528704468920580, -0.07969122161898611889 ) ) ;
#17661 = CARTESIAN_POINT ( 'NONE',  ( 0.6477285649443610405, 156.3042436901572216, -0.05974520555407228373 ) ) ;
#17662 = CIRCLE ( 'NONE', #31965, 5.588000000000006295 ) ;
#17663 = ORIENTED_EDGE ( 'NONE', *, *, #4277, .T. ) ;
#17664 = CARTESIAN_POINT ( 'NONE',  ( 19.98568676637946950, 149.3093937917295762, 2.465107550769984890 ) ) ;
#17665 = CARTESIAN_POINT ( 'NONE',  ( 4.943369476187105427, 113.9634657096399053, 2.116106984914523093 ) ) ;
#17666 = AXIS2_PLACEMENT_3D ( 'NONE', #17800, #4217, #17178 ) ;
#17667 = LINE ( 'NONE', #24269, #27939 ) ;
#17668 = CARTESIAN_POINT ( 'NONE',  ( 0.02768730785345232051, 158.9256195073445213, -1.385586103196075447 ) ) ;
#17669 = CARTESIAN_POINT ( 'NONE',  ( 15.79392588796402208, 121.0087326939336378, 0.08323308591264581835 ) ) ;
#17670 = DIRECTION ( 'NONE',  ( 5.188838149069472160E-16, -1.699382548006136559E-16, -1.000000000000000000 ) ) ;
#17671 = CARTESIAN_POINT ( 'NONE',  ( 1.848236747766272892, -15.62973196022113243, 5.883794544018126516 ) ) ;
#17672 = DIRECTION ( 'NONE',  ( 4.017660918040594346E-17, -1.000000000000000000, -2.376309959284834438E-19 ) ) ;
#17673 = CARTESIAN_POINT ( 'NONE',  ( 1.122158211225881885, 34.81801111161350804, -0.09678150280622686841 ) ) ;
#17674 = CARTESIAN_POINT ( 'NONE',  ( 0.4162271216348931713, 118.1045761740670201, 0.5784513839558712567 ) ) ;
#17675 = ORIENTED_EDGE ( 'NONE', *, *, #40687, .T. ) ;
#17676 = CARTESIAN_POINT ( 'NONE',  ( -8.291425676780491472, 12.16085651096402032, -1.523321141447528948 ) ) ;
#17677 = CARTESIAN_POINT ( 'NONE',  ( -8.672386296370172332, 118.2230072205180420, -0.9366548366208437004 ) ) ;
#17678 = CARTESIAN_POINT ( 'NONE',  ( -3.448667622495882323, 119.7720183225874138, -0.5479595714127596384 ) ) ;
#17679 = CARTESIAN_POINT ( 'NONE',  ( 4.825270798805025407, 117.7346728073316626, 1.017784339641811808 ) ) ;
#17680 = CARTESIAN_POINT ( 'NONE',  ( -13.73816324777078890, 59.55066437026322745, 5.662797264199856073 ) ) ;
#17681 = CARTESIAN_POINT ( 'NONE',  ( -4.423373769213096551, 104.6144662015457243, 1.938597605103610011 ) ) ;
#17682 = CARTESIAN_POINT ( 'NONE',  ( -1.544744425833544099, 4.816215111148435923, 4.377641278133862279 ) ) ;
#17683 = DIRECTION ( 'NONE',  ( -0.8745520943968240202, 0.4849315768086553402, -5.361993529360572958E-16 ) ) ;
#17684 = CARTESIAN_POINT ( 'NONE',  ( -2.780279277094420021, 107.4064198780910431, -4.544082669632513394 ) ) ;
#17685 = CARTESIAN_POINT ( 'NONE',  ( 3.815374714676033729, -13.42234902974577615, 3.291045305163978085 ) ) ;
#17686 = CARTESIAN_POINT ( 'NONE',  ( 0.2613516939665402328, 106.0087397856094356, -5.279363957283110587 ) ) ;
#17687 = AXIS2_PLACEMENT_3D ( 'NONE', #33253, #20436, #10862 ) ;
#17688 = CARTESIAN_POINT ( 'NONE',  ( 2.461214384022098134, 39.20946620154573026, 1.319434448097693169 ) ) ;
#17689 = CARTESIAN_POINT ( 'NONE',  ( -2.055040306894160729, 115.7029326251217185, 1.635618938382796816 ) ) ;
#17690 = EDGE_LOOP ( 'NONE', ( #12683, #18050, #7715, #36547, #26073 ) ) ;
#17691 = CARTESIAN_POINT ( 'NONE',  ( -5.255091509764169722, 104.6144662015501012, -0.9306984194723886272 ) ) ;
#17692 = CARTESIAN_POINT ( 'NONE',  ( 5.310739065812000170, -15.29705283487872691, 0.1354967992945097788 ) ) ;
#17693 = CARTESIAN_POINT ( 'NONE',  ( -13.71253074539983530, 123.6869008171703541, 1.368039988124472695 ) ) ;
#17694 = CARTESIAN_POINT ( 'NONE',  ( -0.5268263777171366957, 24.48095756788062261, 0.8226642508852344271 ) ) ;
#17695 = ORIENTED_EDGE ( 'NONE', *, *, #29205, .F. ) ;
#17696 = ORIENTED_EDGE ( 'NONE', *, *, #25329, .T. ) ;
#17697 = CARTESIAN_POINT ( 'NONE',  ( 1.734723475976807094E-15, 17.14499999999999957, 0.000000000000000000 ) ) ;
#17698 = CARTESIAN_POINT ( 'NONE',  ( 2.486440349385794502, 120.2382744777187611, 0.5044468955786926001 ) ) ;
#17699 =( NAMED_UNIT ( * ) PLANE_ANGLE_UNIT ( ) SI_UNIT ( $, .RADIAN. ) );
#17700 = CARTESIAN_POINT ( 'NONE',  ( -5.181828529333126099, 120.8264575521020987, 0.4749581527667977032 ) ) ;
#17701 = CYLINDRICAL_SURFACE ( 'NONE', #23195, 2.539999999999999591 ) ;
#17702 =( BOUNDED_CURVE ( )  B_SPLINE_CURVE ( 3, ( #12867, #6910, #33107, #7330 ),
 .UNSPECIFIED., .F., .T. ) 
 B_SPLINE_CURVE_WITH_KNOTS ( ( 4, 4 ),
 ( 1.570796326794896558, 3.141592653589793116 ),
 .UNSPECIFIED. ) 
 CURVE ( )  GEOMETRIC_REPRESENTATION_ITEM ( )  RATIONAL_B_SPLINE_CURVE ( ( 1.000000000000000000, 0.8047378541243649375, 0.8047378541243649375, 1.000000000000000000 ) ) 
 REPRESENTATION_ITEM ( '' )  );
#17703 = CARTESIAN_POINT ( 'NONE',  ( 4.550223619785835005, 118.0718490517250814, -0.6268591698733608775 ) ) ;
#17704 = CARTESIAN_POINT ( 'NONE',  ( 17.87798177106712672, 144.5560955566678558, -1.636306359874433847 ) ) ;
#17705 = CARTESIAN_POINT ( 'NONE',  ( -17.00694855514576886, 128.5677977248401476, -2.111551361116177361 ) ) ;
#17706 = DIRECTION ( 'NONE',  ( 1.011795553208986377E-16, 1.000000000000000000, -0.000000000000000000 ) ) ;
#17707 = CIRCLE ( 'NONE', #5480, 5.588000000000006295 ) ;
#17708 = CARTESIAN_POINT ( 'NONE',  ( 4.242333036053028472, 118.2242299894752335, -0.3186625456669344159 ) ) ;
#17709 = CARTESIAN_POINT ( 'NONE',  ( 15.66930740726043148, 147.5723176251010784, -0.2779681209298466293 ) ) ;
#17710 = ORIENTED_EDGE ( 'NONE', *, *, #2757, .T. ) ;
#17711 = CARTESIAN_POINT ( 'NONE',  ( 1.850858793973401584, -15.28950465061244834, 5.390636727418374186 ) ) ;
#17712 = AXIS2_PLACEMENT_3D ( 'NONE', #9448, #32247, #3077 ) ;
#17713 = CARTESIAN_POINT ( 'NONE',  ( 11.42297701379735742, 55.88459609804034756, -4.463034230327253660 ) ) ;
#17714 = CARTESIAN_POINT ( 'NONE',  ( -58.16644339752579640, 0.1874380212899332265, 0.9010643025995082045 ) ) ;
#17715 = CARTESIAN_POINT ( 'NONE',  ( 4.628409624684510781, -5.919234854628785847, 0.1277143096542201761 ) ) ;
#17716 = CARTESIAN_POINT ( 'NONE',  ( 0.5523667267584208007, 120.0661220204379305, 0.4484973920728143049 ) ) ;
#17717 = CARTESIAN_POINT ( 'NONE',  ( -2.190789743540378698, 30.46265602596804811, 2.500874623987990208 ) ) ;
#17718 = CARTESIAN_POINT ( 'NONE',  ( -4.093446853122649109, 111.5999093057820772, 2.867423493935855827 ) ) ;
#17719 = CARTESIAN_POINT ( 'NONE',  ( -1.861891798414337940, 1.167894131763866250, -4.247245584637167504 ) ) ;
#17720 = CARTESIAN_POINT ( 'NONE',  ( 1.611903344789260117, 120.9971453638330985, 0.05790686387416384834 ) ) ;
#17721 = DIRECTION ( 'NONE',  ( 5.188838149069472160E-16, -1.699382548006136559E-16, -1.000000000000000000 ) ) ;
#17722 = CARTESIAN_POINT ( 'NONE',  ( -57.74348367832291018, 0.8661236967133778553, -0.1780388485286305555 ) ) ;
#17723 = CARTESIAN_POINT ( 'NONE',  ( -2.156330945748770045, 116.3329555247961480, -0.2805685296613497637 ) ) ;
#17724 = DIRECTION ( 'NONE',  ( 0.9998004120163608288, 0.000000000000000000, 0.01997839162482736852 ) ) ;
#17725 = CARTESIAN_POINT ( 'NONE',  ( -46.84474875364813329, 25.59693625086653412, -1.568125628604711608 ) ) ;
#17726 = CARTESIAN_POINT ( 'NONE',  ( 1.842426711869075362, -15.45708672024492003, 5.391926158250407219 ) ) ;
#17727 = CARTESIAN_POINT ( 'NONE',  ( -0.01632536679074437017, 38.84944212800221663, 1.323018725044087018 ) ) ;
#17728 = CIRCLE ( 'NONE', #28627, 0.2539999999999992264 ) ;
#17729 = CARTESIAN_POINT ( 'NONE',  ( 6.435022864794023079, 6.566661361801033436, 5.478585407919045025 ) ) ;
#17730 = CARTESIAN_POINT ( 'NONE',  ( -4.825814575782359839, 56.51500000000000767, 4.829586058641171853 ) ) ;
#17731 = CARTESIAN_POINT ( 'NONE',  ( -0.09641566778521773462, 105.7853610664052866, 4.825034276358891816 ) ) ;
#17732 = CARTESIAN_POINT ( 'NONE',  ( -58.08922378330620973, 1.909136410080003454, 0.4248916911265161467 ) ) ;
#17733 = ADVANCED_FACE ( 'NONE', ( #20909 ), #7401, .T. ) ;
#17734 = CARTESIAN_POINT ( 'NONE',  ( -58.87911280034276018, -0.2081424763510641984, -1.061797465414398100E-14 ) ) ;
#17735 = CARTESIAN_POINT ( 'NONE',  ( -23.14523085694538196, 149.5941399179437781, -0.009123583346247826631 ) ) ;
#17736 = ORIENTED_EDGE ( 'NONE', *, *, #37350, .F. ) ;
#17737 = CARTESIAN_POINT ( 'NONE',  ( -57.71825614945207406, 2.868614883688350048, -0.7691332274306353911 ) ) ;
#17738 = ORIENTED_EDGE ( 'NONE', *, *, #21226, .T. ) ;
#17739 = CARTESIAN_POINT ( 'NONE',  ( -44.18728704178806765, 21.36917510655693420, -3.097942224162511415 ) ) ;
#17741 = CARTESIAN_POINT ( 'NONE',  ( -5.959810334499720419, 155.3892724211786742, -0.1190911940436165245 ) ) ;
#17740 = AXIS2_PLACEMENT_3D ( 'NONE', #8783, #34986, #18554 ) ;
#17742 = CARTESIAN_POINT ( 'NONE',  ( 4.034131674322845029, -15.09852482505488780, 5.122685350376444902 ) ) ;
#17743 = CARTESIAN_POINT ( 'NONE',  ( -20.98992760039535099, 147.8517002469272370, 1.565498118541299277 ) ) ;
#17744 = CARTESIAN_POINT ( 'NONE',  ( 22.35542929045582383, 148.9358926463403918, -0.9984386947210761587 ) ) ;
#17745 = CARTESIAN_POINT ( 'NONE',  ( -2.923568588381722844, 13.88697512809157786, 3.594856661414283394 ) ) ;
#17746 = CARTESIAN_POINT ( 'NONE',  ( -6.905720769004730641, 117.2044255678715814, -0.3198409844323960027 ) ) ;
#17747 = CARTESIAN_POINT ( 'NONE',  ( -50.68868110200592980, 15.17409885929999902, -4.768265622168934570 ) ) ;
#17748 = ADVANCED_FACE ( 'NONE', ( #18977 ), #9199, .T. ) ;
#17749 = CARTESIAN_POINT ( 'NONE',  ( 8.796266902338841120, 117.6874721126187779, 0.2328958698391284388 ) ) ;
#17750 = CARTESIAN_POINT ( 'NONE',  ( -10.06933303711913474, 122.3915136462027817, 1.070338282017660791 ) ) ;
#17751 = CARTESIAN_POINT ( 'NONE',  ( -54.28365971233007059, 8.261047645289938401, -3.332732081090967746 ) ) ;
#17752 = CARTESIAN_POINT ( 'NONE',  ( 10.95471005835502609, 121.6366708983051836, -1.250572042008267326 ) ) ;
#17753 = CARTESIAN_POINT ( 'NONE',  ( -7.089439975188652099, 158.1912585135832785, -1.657816039754273163 ) ) ;
#17754 = CARTESIAN_POINT ( 'NONE',  ( -44.66298991629287940, 23.47648082339880915, -1.964675176939946644 ) ) ;
#17755 = PRODUCT_RELATED_PRODUCT_CATEGORY ( 'part', '', ( #4534 ) ) ;
#17756 = CARTESIAN_POINT ( 'NONE',  ( 9.647033449255031812, 123.8920215319950842, -0.4922632944252960385 ) ) ;
#17757 = EDGE_CURVE ( 'NONE', #16319, #18538, #8202, .T. ) ;
#17758 = ORIENTED_EDGE ( 'NONE', *, *, #19283, .F. ) ;
#17759 = CARTESIAN_POINT ( 'NONE',  ( -16.10024230344514962, 135.1141785778430346, -2.240991319914668711 ) ) ;
#17760 = CARTESIAN_POINT ( 'NONE',  ( 4.504576368470070591, -15.30243295294880745, -0.5136648547128764841 ) ) ;
#17761 = CARTESIAN_POINT ( 'NONE',  ( -4.531929919898019854, 118.1072688352402338, -0.6771984859318007643 ) ) ;
#17762 = AXIS2_PLACEMENT_3D ( 'NONE', #9030, #21995, #15609 ) ;
#17763 = ADVANCED_FACE ( 'NONE', ( #12180 ), #28785, .F. ) ;
#17764 = CARTESIAN_POINT ( 'NONE',  ( -56.22331024217277928, 5.808995339285999648, -2.850545730341259798 ) ) ;
#17765 = CARTESIAN_POINT ( 'NONE',  ( -4.866602953137410204, 117.4089747018453238, 0.9905608030323003188 ) ) ;
#17766 = CARTESIAN_POINT ( 'NONE',  ( 7.368974454111232752, 120.7277362223577768, 1.240556355415273870 ) ) ;
#17767 = CARTESIAN_POINT ( 'NONE',  ( -5.332935381406168851, 115.7029491485442634, -0.1065653510733624160 ) ) ;
#17768 = EDGE_CURVE ( 'NONE', #28485, #19344, #19085, .T. ) ;
#17769 = CIRCLE ( 'NONE', #812, 0.3810000000000015041 ) ;
#17770 = CARTESIAN_POINT ( 'NONE',  ( 23.21412382727100976, 149.6303025714371131, 0.4381719528662393337 ) ) ;
#17771 = ADVANCED_FACE ( 'NONE', ( #41798 ), #12596, .T. ) ;
#17772 = CARTESIAN_POINT ( 'NONE',  ( 0.7039615705130309875, 19.50765702457006157, -8.391957350905826729 ) ) ;
#17773 = CARTESIAN_POINT ( 'NONE',  ( 15.70678031088808879, 147.2451778420852406, 0.7656494529899997570 ) ) ;
#17774 = CARTESIAN_POINT ( 'NONE',  ( -8.336765840796966032, 73.19241104973453105, 1.270000000000001572 ) ) ;
#17775 = CARTESIAN_POINT ( 'NONE',  ( -42.01646181069634878, 22.10209156318453694, -0.7046475714187767636 ) ) ;
#17776 = VECTOR ( 'NONE', #29430, 1000.000000000000227 ) ;
#17777 = CARTESIAN_POINT ( 'NONE',  ( 2.186287969701115497, 115.6909491485452577, 1.711441318780086540 ) ) ;
#17778 = CARTESIAN_POINT ( 'NONE',  ( -58.33591949829837375, -0.2304704932390572170, 0.1444701089452633536 ) ) ;
#17779 = CARTESIAN_POINT ( 'NONE',  ( -3.297133786507796760, 159.4684106755469202, -0.01890815954691990250 ) ) ;
#17780 = VERTEX_POINT ( 'NONE', #15779 ) ;
#17781 = CARTESIAN_POINT ( 'NONE',  ( -47.14788814370446346, 23.76379789425250166, -2.690610990139723491 ) ) ;
#17782 = CARTESIAN_POINT ( 'NONE',  ( -7.874818391576265064, 122.1194222050971518, -0.8646837367724872214 ) ) ;
#17783 = DIRECTION ( 'NONE',  ( 0.000000000000000000, -0.000000000000000000, 1.000000000000000000 ) ) ;
#17784 = ORIENTED_EDGE ( 'NONE', *, *, #33678, .T. ) ;
#17785 = CARTESIAN_POINT ( 'NONE',  ( -4.757314290308038984, 117.4006805855117364, -1.206872172350066164 ) ) ;
#17786 = CARTESIAN_POINT ( 'NONE',  ( -2.787004648571314025, 120.9517662584847102, -0.1965090384792944900 ) ) ;
#17787 = CARTESIAN_POINT ( 'NONE',  ( 4.523112235310252416, -13.07411707498565256, 2.966381825927230764 ) ) ;
#17788 = TOROIDAL_SURFACE ( 'NONE', #5575, 5.080000000000005400, 0.5080000000000000071 ) ;
#17789 = CARTESIAN_POINT ( 'NONE',  ( -1.091392056213116746, 117.4935207075373569, 0.4954137919519209232 ) ) ;
#17790 = DIRECTION ( 'NONE',  ( 0.9998004120163609398, 0.000000000000000000, 0.01997839162482749689 ) ) ;
#17791 = AXIS2_PLACEMENT_3D ( 'NONE', #29901, #36509, #3298 ) ;
#17792 = CARTESIAN_POINT ( 'NONE',  ( 6.903663268456370794, 117.1865127098105575, 0.2656477445430290296 ) ) ;
#17793 = CARTESIAN_POINT ( 'NONE',  ( 10.99029326479648461, 127.9870517001798760, 0.2725059437867732859 ) ) ;
#17794 = ORIENTED_EDGE ( 'NONE', *, *, #10577, .T. ) ;
#17795 = CARTESIAN_POINT ( 'NONE',  ( 0.4606059098249736805, 26.09511874640634943, 0.8667040019166204479 ) ) ;
#17796 = CARTESIAN_POINT ( 'NONE',  ( -22.98488057257204886, 150.1591296352320910, -0.4592926148156235011 ) ) ;
#17797 = VECTOR ( 'NONE', #1699, 1000.000000000000114 ) ;
#17798 = CARTESIAN_POINT ( 'NONE',  ( -43.55282861522693594, 21.75186539808470698, -2.470256665153925724 ) ) ;
#17799 = EDGE_LOOP ( 'NONE', ( #5645, #35695, #18483, #33085 ) ) ;
#17800 = CARTESIAN_POINT ( 'NONE',  ( 10.39494437172059094, 55.24500000000000455, 5.094799277214218769 ) ) ;
#17801 = ORIENTED_EDGE ( 'NONE', *, *, #6848, .F. ) ;
#17802 = CARTESIAN_POINT ( 'NONE',  ( -8.499151694004579483, 119.2578417338014702, 1.013587109124426178 ) ) ;
#17803 = CARTESIAN_POINT ( 'NONE',  ( -3.254339884055971854, 0.1279812147911008058, 3.287934741457726684 ) ) ;
#17804 = CARTESIAN_POINT ( 'NONE',  ( 14.46681479972615136, 121.7426775721902175, 1.517288920005034791 ) ) ;
#17805 = CARTESIAN_POINT ( 'NONE',  ( -58.63158931450414002, -0.2944865825844911189, -0.3706283016938188846 ) ) ;
#17806 = CARTESIAN_POINT ( 'NONE',  ( 0.03153870137008670665, 158.4432089348667319, -1.578325583784928154 ) ) ;
#17807 = CARTESIAN_POINT ( 'NONE',  ( -1.011143250135940530, 20.41458852336931074, 8.389224627043086358 ) ) ;
#17808 = CARTESIAN_POINT ( 'NONE',  ( -14.51109376910522286, 156.0472725025049954, -1.459756479172738874 ) ) ;
#17809 = CARTESIAN_POINT ( 'NONE',  ( 4.772939762337750302, 117.6315509942823923, -0.9548895502630124765 ) ) ;
#17810 = ORIENTED_EDGE ( 'NONE', *, *, #34479, .F. ) ;
#17811 = EDGE_CURVE ( 'NONE', #31901, #32861, #25900, .T. ) ;
#17812 = CARTESIAN_POINT ( 'NONE',  ( -15.81858318527965324, 146.5893318786020814, 0.01456738144011954575 ) ) ;
#17813 = CARTESIAN_POINT ( 'NONE',  ( 4.034131674322845029, -15.09852482505488780, 5.122685350376444902 ) ) ;
#17814 = EDGE_CURVE ( 'NONE', #7084, #18074, #10061, .T. ) ;
#17815 = DIRECTION ( 'NONE',  ( 5.188838149069472160E-16, -1.699382548006136559E-16, -1.000000000000000000 ) ) ;
#17816 = CARTESIAN_POINT ( 'NONE',  ( -3.099633551182617186, 108.5668320698263898, -4.179674138198564926 ) ) ;
#17817 = EDGE_LOOP ( 'NONE', ( #38199, #36391, #16454, #11750 ) ) ;
#17818 = CARTESIAN_POINT ( 'NONE',  ( 4.182621382391884524, 157.4559852174668322, 1.843664507743932424 ) ) ;
#17819 = CARTESIAN_POINT ( 'NONE',  ( -30.75918919842648336, 69.77432548395512413, -1.270000000000007567 ) ) ;
#17820 = EDGE_CURVE ( 'NONE', #3641, #18200, #5599, .T. ) ;
#17821 = CARTESIAN_POINT ( 'NONE',  ( -29.24376532021898356, 65.27002024517358336, -1.270000000000005791 ) ) ;
#17822 = AXIS2_PLACEMENT_3D ( 'NONE', #26657, #10468, #19207 ) ;
#17823 = CARTESIAN_POINT ( 'NONE',  ( -0.5256976547266306588, 110.0486234891351245, 3.677594289785357518 ) ) ;
#17824 = ADVANCED_FACE ( 'NONE', ( #1976 ), #15000, .T. ) ;
#17825 = CARTESIAN_POINT ( 'NONE',  ( -2.748994976520039213, 10.49642266832308124, 7.958378898918418543 ) ) ;
#17826 = CARTESIAN_POINT ( 'NONE',  ( 14.94238115049589588, 139.3652335140928074, 1.424457715676853642 ) ) ;
#17827 = CARTESIAN_POINT ( 'NONE',  ( -5.486567272856878414E-14, 86.35999999999998522, 0.000000000000000000 ) ) ;
#17828 = CARTESIAN_POINT ( 'NONE',  ( 2.863213894092299316, 116.8186761214209213, -0.2817159656421848180 ) ) ;
#17829 = DIRECTION ( 'NONE',  ( -1.011795553208986377E-16, -1.000000000000000000, 0.000000000000000000 ) ) ;
#17830 = ADVANCED_FACE ( 'NONE', ( #37957 ), #15361, .F. ) ;
#17831 = CARTESIAN_POINT ( 'NONE',  ( -56.09991784293080030, 4.552033362070804223, 2.401778663949239778 ) ) ;
#17832 = CARTESIAN_POINT ( 'NONE',  ( -48.75791856165849936, 18.18949858612532466, 5.155209323065509608 ) ) ;
#17833 = LINE ( 'NONE', #6281, #7603 ) ;
#17834 = CARTESIAN_POINT ( 'NONE',  ( -4.257826819935623064, 118.2250077456210846, 0.3017621733391205874 ) ) ;
#17835 = DIRECTION ( 'NONE',  ( -6.353134868986659519E-16, 1.000000000000000000, 0.000000000000000000 ) ) ;
#17836 = ORIENTED_EDGE ( 'NONE', *, *, #11013, .T. ) ;
#17837 = CARTESIAN_POINT ( 'NONE',  ( -51.34009458250667279, 14.66650723912346699, 4.800162786360129274 ) ) ;
#17838 = CARTESIAN_POINT ( 'NONE',  ( 8.312601280572751605, 120.1777224443565615, -1.117780186305196821 ) ) ;
#17839 = CARTESIAN_POINT ( 'NONE',  ( -7.326027964658058167, 123.0350022594044219, -0.2150643116641766939 ) ) ;
#17840 = CARTESIAN_POINT ( 'NONE',  ( 4.296427252414747322, 118.2130177109110321, 0.5011668729022451529 ) ) ;
#17841 = CARTESIAN_POINT ( 'NONE',  ( -0.6009856513686788748, 120.6441756478195089, -0.2688776736664573175 ) ) ;
#17842 = CARTESIAN_POINT ( 'NONE',  ( -29.57045817531687959, 58.76046099849394011, 1.523999999999993138 ) ) ;
#17843 = FACE_BOUND ( 'NONE', #31275, .T. ) ;
#17844 = EDGE_LOOP ( 'NONE', ( #955, #21299 ) ) ;
#17845 = CARTESIAN_POINT ( 'NONE',  ( -0.9950013725589796909, 29.65466048987409309, -4.513790593961638287 ) ) ;
#17846 = CARTESIAN_POINT ( 'NONE',  ( -13.40915985073344352, 130.9706359334022920, -1.586196205478585197 ) ) ;
#17847 = DIRECTION ( 'NONE',  ( 0.8745520943968240202, -0.4849315768086553402, 6.829619984160650158E-16 ) ) ;
#17848 = CARTESIAN_POINT ( 'NONE',  ( -47.59852559863926302, 19.66225068540052945, 5.176489187661841740 ) ) ;
#17849 = LINE ( 'NONE', #24242, #40587 ) ;
#17850 = CARTESIAN_POINT ( 'NONE',  ( -15.64684598352423350, 147.2230049032471868, -0.1119480208309122649 ) ) ;
#17851 = CARTESIAN_POINT ( 'NONE',  ( 4.636249899789679496, -11.37698174978397958, -0.2454043791197063895 ) ) ;
#17852 = CARTESIAN_POINT ( 'NONE',  ( 22.71262516694549660, 146.4845460041848355, 1.645735859231715725 ) ) ;
#17853 = CARTESIAN_POINT ( 'NONE',  ( 5.475330206976777525, 77.01756249999996840, -5.107412922131463695 ) ) ;
#17855 = CARTESIAN_POINT ( 'NONE',  ( 0.009513433763446757160, 117.6614778598761291, -0.4760911276077179899 ) ) ;
#17854 = CARTESIAN_POINT ( 'NONE',  ( 3.221735024265227398, -14.36526069886394730, 2.718910799868354378 ) ) ;
#17856 = CARTESIAN_POINT ( 'NONE',  ( -11.27019207447484384, 122.4230570912197038, 1.244363564371071540 ) ) ;
#17857 = CARTESIAN_POINT ( 'NONE',  ( -0.8659212883131867100, -1.167510040683709560, 0.4517697218592801600 ) ) ;
#17858 = CARTESIAN_POINT ( 'NONE',  ( -15.17352684164009524, 120.8830733721255370, -0.9063557954379339865 ) ) ;
#17859 = CIRCLE ( 'NONE', #25346, 8.794750000000000512 ) ;
#17860 = CARTESIAN_POINT ( 'NONE',  ( 0.4978855121113271442, 23.66801414613304289, -0.8366695591092367934 ) ) ;
#17861 = ORIENTED_EDGE ( 'NONE', *, *, #1224, .T. ) ;
#17862 = CARTESIAN_POINT ( 'NONE',  ( -48.90916507497669841, 16.41193755240580288, 3.099911505780750254 ) ) ;
#17863 = CARTESIAN_POINT ( 'NONE',  ( -9.542276680740393147, 123.9284174147966269, 0.4124357159827420349 ) ) ;
#17864 = CARTESIAN_POINT ( 'NONE',  ( 4.564001774108119136, -12.95384785397724059, 2.770574723176509657 ) ) ;
#17865 = CARTESIAN_POINT ( 'NONE',  ( 5.875224328284113895, 120.7327493588883840, -0.6546335550538250336 ) ) ;
#17866 = VERTEX_POINT ( 'NONE', #6837 ) ;
#17867 = CARTESIAN_POINT ( 'NONE',  ( 0.5746707734919784816, 115.7029522474750820, 1.760669174839533557 ) ) ;
#17868 = CIRCLE ( 'NONE', #22624, 0.6350000000000001199 ) ;
#17869 = CARTESIAN_POINT ( 'NONE',  ( 3.398501971686946010, -13.69110397484313246, 2.823423868610629217 ) ) ;
#17870 = CARTESIAN_POINT ( 'NONE',  ( -4.707310151561321376, 117.7551317797143469, -1.085303849379790186 ) ) ;
#17871 = CARTESIAN_POINT ( 'NONE',  ( 9.119960873764027198, 153.9201329141909866, 0.06997149051007753306 ) ) ;
#17872 = ORIENTED_EDGE ( 'NONE', *, *, #12340, .F. ) ;
#17873 = CARTESIAN_POINT ( 'NONE',  ( 13.15656197906093894, 122.1656469061080514, 1.777190774585285071 ) ) ;
#17874 = FACE_OUTER_BOUND ( 'NONE', #25745, .T. ) ;
#17875 = CARTESIAN_POINT ( 'NONE',  ( -18.58115504727956591, 80.30342350548193053, 1.523999999999996247 ) ) ;
#17876 = EDGE_CURVE ( 'NONE', #40376, #37721, #34097, .T. ) ;
#17877 = CARTESIAN_POINT ( 'NONE',  ( 0.02615319344467511437, 156.8698190429800832, -1.308812744920978322 ) ) ;
#17878 = CARTESIAN_POINT ( 'NONE',  ( 9.784355093145334692, 118.0142902678875885, -0.004515160920743642621 ) ) ;
#17879 = CARTESIAN_POINT ( 'NONE',  ( -29.89586364642803318, 71.55302121702176521, 1.269999999999991802 ) ) ;
#17880 = AXIS2_PLACEMENT_3D ( 'NONE', #12717, #38712, #6339 ) ;
#17881 = AXIS2_PLACEMENT_3D ( 'NONE', #39837, #33442, #17232 ) ;
#17882 = CARTESIAN_POINT ( 'NONE',  ( 1.931858869400174150, -15.61904180168537160, 5.924774731895777080 ) ) ;
#17883 = CARTESIAN_POINT ( 'NONE',  ( -24.26619908708081041, 81.70586579672512073, 1.523999999999993138 ) ) ;
#17884 = CARTESIAN_POINT ( 'NONE',  ( -1.912856793975784786, 32.45769749710033381, 0.9767251062931671113 ) ) ;
#17885 = CARTESIAN_POINT ( 'NONE',  ( -4.753021167359183785, 117.9428942815730466, 0.6272315166840956024 ) ) ;
#17886 = ORIENTED_EDGE ( 'NONE', *, *, #17099, .T. ) ;
#17887 = ORIENTED_EDGE ( 'NONE', *, *, #10758, .T. ) ;
#17888 = CARTESIAN_POINT ( 'NONE',  ( -23.49500000000000455, 71.11999999999999034, 5.016499999999999737 ) ) ;
#17889 = CARTESIAN_POINT ( 'NONE',  ( -8.482050796837413031, 119.1145137661371933, -1.313062426393583060 ) ) ;
#17890 = CARTESIAN_POINT ( 'NONE',  ( -5.854942301702540597, 124.9344662015456890, -0.1169956811762812854 ) ) ;
#17891 = CARTESIAN_POINT ( 'NONE',  ( 4.883721824859848404, 117.6381041156431024, 1.023514187599162906 ) ) ;
#17892 = DIRECTION ( 'NONE',  ( 1.011795553208986377E-16, 1.000000000000000000, -0.000000000000000000 ) ) ;
#17893 = CARTESIAN_POINT ( 'NONE',  ( -0.9884870862450249041, 123.5966405200008325, 0.1018174175105951568 ) ) ;
#17894 = VECTOR ( 'NONE', #4615, 1000.000000000000227 ) ;
#17895 = CARTESIAN_POINT ( 'NONE',  ( 1.961646697876492373, -0.1315482170498871728, -4.191205975169975950 ) ) ;
#17896 = CARTESIAN_POINT ( 'NONE',  ( 5.002599301907898699, 117.4023545182666055, -0.8031422281648238348 ) ) ;
#17897 = CARTESIAN_POINT ( 'NONE',  ( -3.332395206781303187, 108.2587724951642087, -4.156421558053723153 ) ) ;
#17898 = CARTESIAN_POINT ( 'NONE',  ( 3.350179296191433398, -14.02378440268806159, 3.677192885962260682 ) ) ;
#17899 = CARTESIAN_POINT ( 'NONE',  ( 0.1065646865914872121, 105.8844662015457061, -5.332932678536314697 ) ) ;
#17900 = CARTESIAN_POINT ( 'NONE',  ( -4.338858593134309771, 28.47720539748115698, 2.044640056223529179 ) ) ;
#17901 = CARTESIAN_POINT ( 'NONE',  ( -2.051726258433167693, 115.7029491863252133, 1.635864041877385100 ) ) ;
#17902 = CARTESIAN_POINT ( 'NONE',  ( 0.9564925537785137211, 29.00497265395555857, -4.523030980006896407 ) ) ;
#17903 = VERTEX_POINT ( 'NONE', #33042 ) ;
#17904 = CARTESIAN_POINT ( 'NONE',  ( -5.344509134975541365, 104.6144662015523750, 0.1077285959981589963 ) ) ;
#17905 = CARTESIAN_POINT ( 'NONE',  ( 4.028426573186930426, -15.65323953938244017, 3.316845843096514201 ) ) ;
#17906 = CARTESIAN_POINT ( 'NONE',  ( -7.699499347746557198, 119.6133147451300971, 1.075113282820071570 ) ) ;
#17907 = CARTESIAN_POINT ( 'NONE',  ( 0.2459283266301676152, 20.16186220226971315, -0.9436028068393225166 ) ) ;
#17908 = ORIENTED_EDGE ( 'NONE', *, *, #23999, .T. ) ;
#17909 = ORIENTED_EDGE ( 'NONE', *, *, #35198, .F. ) ;
#17910 = DIRECTION ( 'NONE',  ( -0.9998004120163608288, 0.000000000000000000, -0.01997839162482749342 ) ) ;
#17911 = CARTESIAN_POINT ( 'NONE',  ( 1.040151681621031221, 108.5039085404744981, 4.268591994808179635 ) ) ;
#17912 = CARTESIAN_POINT ( 'NONE',  ( -12.75300196040212874, 152.1353413313561305, 1.119124812251137691 ) ) ;
#17913 = DIRECTION ( 'NONE',  ( 0.1715592850456333085, 0.1224830539174543292, -0.9775302108976914317 ) ) ;
#17914 = CARTESIAN_POINT ( 'NONE',  ( 4.531563741779123689, 118.0870819156608320, -0.6068543356175654102 ) ) ;
#17915 = CARTESIAN_POINT ( 'NONE',  ( 5.873949295438634977, 120.1673030736515955, -0.8402073876045390577 ) ) ;
#17916 = AXIS2_PLACEMENT_3D ( 'NONE', #15014, #21391, #30998 ) ;
#17917 = CARTESIAN_POINT ( 'NONE',  ( 0.01133701039331720326, 118.4098733054621277, -0.5673503590873751889 ) ) ;
#17918 = CARTESIAN_POINT ( 'NONE',  ( -6.639407854763120941E-14, 101.6934662015457320, 3.307182826377456566E-30 ) ) ;
#17919 = CARTESIAN_POINT ( 'NONE',  ( 4.270423886376517153, 118.2236112661795175, -0.2874234743081488519 ) ) ;
#17920 = AXIS2_PLACEMENT_3D ( 'NONE', #23786, #4231, #7833 ) ;
#17921 = CARTESIAN_POINT ( 'NONE',  ( 7.650102001921197825, 122.3449549946481056, -0.2051776793030276602 ) ) ;
#17922 = ORIENTED_EDGE ( 'NONE', *, *, #10763, .T. ) ;
#17923 = CARTESIAN_POINT ( 'NONE',  ( 2.233078627056604759, -15.14192004606506536, 5.083345892419886880 ) ) ;
#17924 = AXIS2_PLACEMENT_3D ( 'NONE', #18501, #2770, #2565 ) ;
#17925 = CARTESIAN_POINT ( 'NONE',  ( -58.40429423216560423, -0.3346038877926625354, 0.4235997928849980498 ) ) ;
#17926 = CARTESIAN_POINT ( 'NONE',  ( 0.6256056815405413030, -8.068247431453825058, 4.577905309659676014 ) ) ;
#17927 = CARTESIAN_POINT ( 'NONE',  ( 16.96873827569982041, 146.4457527449227143, 1.929048950080526126 ) ) ;
#17928 = CARTESIAN_POINT ( 'NONE',  ( -2.804869963407872202, 28.95498092762696984, 0.1876698244966022444 ) ) ;
#17929 = CARTESIAN_POINT ( 'NONE',  ( -7.256067632580425197, 123.0461458356614628, -0.07605313119184028969 ) ) ;
#17930 = VECTOR ( 'NONE', #30107, 1000.000000000000000 ) ;
#17931 = EDGE_CURVE ( 'NONE', #5200, #24894, #16407, .T. ) ;
#17932 = CARTESIAN_POINT ( 'NONE',  ( -3.416230376366909294, -5.529048218071860532, 3.121479803864907865 ) ) ;
#17933 = CARTESIAN_POINT ( 'NONE',  ( 15.77055413937410222, 146.5697412905949477, 0.3665361178749760307 ) ) ;
#17934 = CARTESIAN_POINT ( 'NONE',  ( 8.237246883283409815, -6.118032110028554627, 1.824569540066587114 ) ) ;
#17935 = CARTESIAN_POINT ( 'NONE',  ( -58.24002838079472610, 0.001074765447070524793, -0.6562585879479864159 ) ) ;
#17936 = CARTESIAN_POINT ( 'NONE',  ( -8.777543396403881815, 117.7565081666817832, -0.4614390791137490955 ) ) ;
#17937 = CARTESIAN_POINT ( 'NONE',  ( 0.009645608633017716330, 120.9711055683165597, -0.4827056984855355171 ) ) ;
#17938 = TOROIDAL_SURFACE ( 'NONE', #41788, 0.8889999999999989022, 0.2540000000000000036 ) ;
#17939 = CYLINDRICAL_SURFACE ( 'NONE', #28036, 0.2539999999999937863 ) ;
#17940 = CARTESIAN_POINT ( 'NONE',  ( 2.058067359092983661, -15.63668844659656187, 5.842422791592847275 ) ) ;
#17941 = DIRECTION ( 'NONE',  ( -5.188838149069472160E-16, 1.699382548006136559E-16, 1.000000000000000000 ) ) ;
#17942 = CARTESIAN_POINT ( 'NONE',  ( 4.223004820120735303, -0.3563183945215069870, -7.287282906663286930 ) ) ;
#17943 = CYLINDRICAL_SURFACE ( 'NONE', #13010, 3.175000000000001155 ) ;
#17944 = CARTESIAN_POINT ( 'NONE',  ( 1.650612623617701651E-15, 17.14499999999999957, 0.000000000000000000 ) ) ;
#17945 = CARTESIAN_POINT ( 'NONE',  ( 2.350639260211558668, -15.10312717587823705, 4.966175652281853203 ) ) ;
#17946 = CARTESIAN_POINT ( 'NONE',  ( -58.37241122568488549, -0.2962816677227753104, -1.034007718770489626E-14 ) ) ;
#17947 = CARTESIAN_POINT ( 'NONE',  ( -15.06072413439841817, 156.1474796653986630, 0.2161187639505617319 ) ) ;
#17948 = ORIENTED_EDGE ( 'NONE', *, *, #31348, .F. ) ;
#17949 = CARTESIAN_POINT ( 'NONE',  ( -58.83227707057486811, -0.08366279997995551554, -5.952756869281050995E-15 ) ) ;
#17950 =( BOUNDED_SURFACE ( )  B_SPLINE_SURFACE ( 3, 2, ( 
 ( #25380, #9197, #38385 ),
 ( #13587, #29571, #16562 ),
 ( #407, #21953, #15359 ),
 ( #3811, #16775, #28366 ),
 ( #10389, #12176, #36179 ),
 ( #16346, #29351, #35186 ),
 ( #13165, #23361, #25172 ),
 ( #5805, #26576, #18760 ),
 ( #22154, #31771, #13375 ),
 ( #18973, #22934, #26155 ),
 ( #39156, #9962, #35963 ),
 ( #26362, #39371, #10173 ),
 ( #39584, #36395, #17816 ),
 ( #24415, #4861, #1451 ),
 ( #39803, #1033, #26793 ),
 ( #30609, #23575, #30192 ),
 ( #20171, #36598, #4232 ),
 ( #13997, #33614, #30816 ),
 ( #4651, #33822, #7834 ),
 ( #37420, #33197, #37218 ) ),
 .UNSPECIFIED., .F., .F., .F. ) 
 B_SPLINE_SURFACE_WITH_KNOTS ( ( 4, 2, 2, 2, 2, 2, 2, 2, 2, 4 ),
 ( 3, 3 ),
 ( -3.009270892369297901E-16, 0.0008043714308976721581, 0.001608742861795645291, 0.002413114292693618532, 0.003217485723591591556, 0.004021857154489564580, 0.004826228585387538038, 0.006434971447183484086, 0.009652457170775376183, 0.01286994289436726828 ),
 ( 0.000000000000000000, 1.000000000000000000 ),
 .UNSPECIFIED. ) 
 GEOMETRIC_REPRESENTATION_ITEM ( )  RATIONAL_B_SPLINE_SURFACE ( (
 ( 1.000000000000000000, 0.9815197824473285149, 1.000000000000000000),
 ( 1.000000000000000000, 0.9811723635258926546, 1.000000000000000000),
 ( 1.000000000000000000, 0.9803956462538041539, 1.000000000000000000),
 ( 1.000000000000000000, 0.9775604298907969447, 1.000000000000000000),
 ( 1.000000000000000000, 0.9755054586208901091, 1.000000000000000000),
 ( 1.000000000000000000, 0.9704993482238920555, 1.000000000000000000),
 ( 1.000000000000000000, 0.9675447666335766916, 1.000000000000000000),
 ( 1.000000000000000000, 0.9610561756468071204, 1.000000000000000000),
 ( 1.000000000000000000, 0.9575813355064265453, 1.000000000000000000),
 ( 1.000000000000000000, 0.9503236772837940771, 1.000000000000000000),
 ( 1.000000000000000000, 0.9465499958478611475, 1.000000000000000000),
 ( 1.000000000000000000, 0.9387344193221167643, 1.000000000000000000),
 ( 1.000000000000000000, 0.9346745718259914515, 1.000000000000000000),
 ( 1.000000000000000000, 0.9222609948196353047, 1.000000000000000000),
 ( 1.000000000000000000, 0.9134583146165992096, 1.000000000000000000),
 ( 1.000000000000000000, 0.8860507374761776855, 1.000000000000000000),
 ( 1.000000000000000000, 0.8669451626876586436, 1.000000000000000000),
 ( 1.000000000000000000, 0.8330907799448757922, 1.000000000000000000),
 ( 1.000000000000000000, 0.8189901318540898645, 1.000000000000000000),
 ( 1.000000000000000000, 0.8121911378916643054, 1.000000000000000000) ) ) 
 REPRESENTATION_ITEM ( '' )  SURFACE ( )  );
#17951 = ORIENTED_EDGE ( 'NONE', *, *, #458, .F. ) ;
#17952 = CARTESIAN_POINT ( 'NONE',  ( -46.53702275532300092, 20.69065974945478104, -4.840627275220472647 ) ) ;
#17953 = CARTESIAN_POINT ( 'NONE',  ( -9.118174893680297544, 124.1671967267183589, -0.1822028344259498389 ) ) ;
#17954 = CARTESIAN_POINT ( 'NONE',  ( 4.666472529085985421, -15.22678077218547799, 4.383143511210439769 ) ) ;
#17955 = CARTESIAN_POINT ( 'NONE',  ( -3.126689565637764456, 118.0390668470448929, 0.7034308075613268096 ) ) ;
#17956 = CIRCLE ( 'NONE', #10453, 0.6349999999999984546 ) ;
#17957 = CARTESIAN_POINT ( 'NONE',  ( 22.59368173950831604, 146.4122051224262577, -0.8656317577275308706 ) ) ;
#17958 = CARTESIAN_POINT ( 'NONE',  ( -2.755274729907521980, 20.69627551736597226, -3.746277899328600558 ) ) ;
#17959 = CARTESIAN_POINT ( 'NONE',  ( -15.20946960781377832, 120.7148350616293300, -0.7222319099908601769 ) ) ;
#17960 = CARTESIAN_POINT ( 'NONE',  ( -48.62040608122599394, 18.38533207009528070, -5.173709449133584215 ) ) ;
#17961 = EDGE_LOOP ( 'NONE', ( #7678, #15551, #33368, #17801 ) ) ;
#17962 = CARTESIAN_POINT ( 'NONE',  ( 5.561693798059717864, 116.7001734479162138, 0.1683348082849521199 ) ) ;
#17963 = CARTESIAN_POINT ( 'NONE',  ( -20.21600168833980149, 80.16988503754176065, -1.270000000000003793 ) ) ;
#17964 = CARTESIAN_POINT ( 'NONE',  ( -1.391675519083843460, 119.6596719632383383, 0.5469696729655013634 ) ) ;
#17965 = CARTESIAN_POINT ( 'NONE',  ( -48.83525966142772745, 18.03881763506669955, -5.101163988045986031 ) ) ;
#17966 = ADVANCED_FACE ( 'NONE', ( #35605 ), #37481, .T. ) ;
#17967 = CARTESIAN_POINT ( 'NONE',  ( 1.284628845569729894, 118.8689652838214244, -0.6394392525890019163 ) ) ;
#17968 = CIRCLE ( 'NONE', #41807, 0.2539999999999942859 ) ;
#17969 = CARTESIAN_POINT ( 'NONE',  ( -15.17292428814161553, 123.1171956318823533, -1.668999667383225471 ) ) ;
#17970 = CARTESIAN_POINT ( 'NONE',  ( -48.53848336910535011, 19.22582880449973075, -5.323527254358048744 ) ) ;
#17971 = CARTESIAN_POINT ( 'NONE',  ( 7.796255004792614685, 122.1031240515655298, -0.5053261734565677177 ) ) ;
#17972 = ORIENTED_EDGE ( 'NONE', *, *, #6532, .T. ) ;
#17973 = CARTESIAN_POINT ( 'NONE',  ( -17.13831219182137033, 149.7102054596878702, -2.353104315458284468 ) ) ;
#17974 = CARTESIAN_POINT ( 'NONE',  ( 4.184971198371238543, -15.30562903706386635, -0.2021278847381603183 ) ) ;
#17975 = AXIS2_PLACEMENT_3D ( 'NONE', #32151, #25958, #12964 ) ;
#17976 = CARTESIAN_POINT ( 'NONE',  ( -4.468857898947769414, 118.1303058819741381, -0.7050480387964153106 ) ) ;
#17977 = EDGE_CURVE ( 'NONE', #35748, #33508, #1449, .T. ) ;
#17978 = CARTESIAN_POINT ( 'NONE',  ( -57.36719850051837000, 1.975114663830185302, -1.756955940785672077 ) ) ;
#17979 = CARTESIAN_POINT ( 'NONE',  ( -4.888083438996877916, 117.4785984266663803, 0.9708402414164146732 ) ) ;
#17980 = CARTESIAN_POINT ( 'NONE',  ( 6.574985064279017521, 120.4115791468657903, 1.154926965394999394 ) ) ;
#17981 = CARTESIAN_POINT ( 'NONE',  ( -6.566230858599542383E-14, 82.13546620154573930, -5.726718672203201028E-18 ) ) ;
#17982 = CARTESIAN_POINT ( 'NONE',  ( -8.022552064266685434, 3.315157024569945765, 2.561087356634513590 ) ) ;
#17983 = CARTESIAN_POINT ( 'NONE',  ( 15.76219760562750771, 147.2673792861271522, 0.9072345144146886087 ) ) ;
#17984 = CARTESIAN_POINT ( 'NONE',  ( -58.50860430493789721, 0.7049166599848305514, -0.9756837515128595761 ) ) ;
#17985 = CARTESIAN_POINT ( 'NONE',  ( -43.98989719630797168, 21.38545485255711398, -2.905481552205971596 ) ) ;
#17986 = CARTESIAN_POINT ( 'NONE',  ( -2.558524215040917316, 118.1588900017448509, 0.7376291965803625228 ) ) ;
#17987 = CARTESIAN_POINT ( 'NONE',  ( 2.765784402779746465, 118.7629491485453883, 1.199736011334208818 ) ) ;
#17988 = B_SPLINE_CURVE_WITH_KNOTS ( 'NONE', 3,
 ( #32555, #6371, #38747, #9972, #29789, #416, #23372, #26373, #19341, #32347, #41951, #39381, #26587, #3608, #10184, #39165, #16355, #29142, #23153, #42159, #3824, #36190, #13598, #12954, #9554, #35762, #3390, #22526, #29362, #36405, #19138, #32142, #2974, #36820, #4245, #4872, #37230, #7639, #14009, #10818, #7430, #4033, #17619, #27633, #17207, #30411, #11031, #8048, #20598, #4663, #833, #1259, #21021, #17831, #34044, #33629, #36611, #26806, #40236, #30828, #30621, #4457, #23801, #13808, #17414, #14213, #27223, #11235, #27430, #1676, #39814, #7848, #1045, #27016, #24012, #37032, #20809, #33835, #30205, #10607, #40024, #33208, #14631, #1464, #20388, #23588, #14422, #40644, #33413, #40443, #11438, #24219, #24426, #7222, #20183, #16994, #29993, #5713, #15683, #34458, #18454, #15049, #28051, #18669, #11653, #35096, #14839, #21224, #5493, #28267, #31459, #8887, #25068, #24638, #24860, #2303, #2516, #31676, #15263, #37856, #37649, #12079, #38071, #34880, #15480, #2725, #8679, #28481, #9105, #41274, #21641, #41060, #1877, #11870, #41486, #12506, #34665, #12293, #28687, #8474, #25281, #21852, #38285, #21430, #22069, #5084, #5291, #31889, #18036, #18240, #5918, #18880, #41695, #37431, #8252, #31242, #34255, #2086, #31037, #27844, #40851, #38913, #374, #19936, #22275, #6330, #16741, #15893 ),
 .UNSPECIFIED., .F., .F.,
 ( 4, 2, 2, 2, 2, 1, 1, 1, 2, 2, 2, 1, 1, 1, 1, 2, 2, 2, 1, 2, 2, 1, 1, 1, 1, 1, 1, 1, 1, 2, 2, 2, 2, 2, 1, 1, 1, 1, 1, 2, 2, 2, 2, 2, 2, 2, 2, 2, 2, 2, 1, 2, 2, 2, 2, 2, 1, 1, 1, 2, 2, 2, 2, 2, 2, 2, 2, 1, 2, 2, 2, 2, 1, 2, 2, 2, 2, 1, 1, 1, 2, 2, 2, 1, 1, 1, 2, 2, 2, 2, 1, 2, 2, 2, 1, 2, 2, 2, 1, 2, 2, 4 ),
 ( 0.000000000000000000, 0.03124999999999582972, 0.06249999999999165945, 0.07031249999999060474, 0.07226562499999056310, 0.07421874999999052147, 0.07812499999999043820, 0.09374999999998993860, 0.1249999999999889533, 0.1874999999999869826, 0.2187499999999860112, 0.2343749999999854006, 0.2421874999999849842, 0.2460937499999849842, 0.2480468749999849565, 0.2490234374999850675, 0.2499999999999851230, 0.3749999999999627520, 0.3906249999999598654, 0.3925781249999596989, 0.3945312499999595879, 0.3984374999999594769, 0.4062499999999596434, 0.4374999999999604761, 0.4687499999999613087, 0.4843749999999614753, 0.4921874999999617528, 0.4960937499999616418, 0.4980468749999616418, 0.4990234374999615863, 0.4999999999999615863, 0.6249999999999517053, 0.6874999999999467093, 0.7187499999999442668, 0.7343749999999431566, 0.7421874999999427125, 0.7460937499999424904, 0.7480468749999424904, 0.7490234374999424904, 0.7495117187499424904, 0.7499999999999424904, 0.8124999999999656941, 0.8437499999999771294, 0.8593749999999827915, 0.8671874999999856781, 0.8710937499999867883, 0.8749999999999878986, 0.8906249999999940048, 0.8984374999999971134, 0.9003906249999981126, 0.9023437499999990008, 0.9062500000000008882, 0.9140625000000045519, 0.9179687500000063283, 0.9218750000000079936, 0.9296875000000117684, 0.9335937500000134337, 0.9355468750000140998, 0.9365234375000144329, 0.9370117187500146549, 0.9375000000000147660, 0.9414062500000129896, 0.9433593750000121014, 0.9443359375000116573, 0.9453125000000112133, 0.9492187500000097700, 0.9511718750000092149, 0.9521484375000092149, 0.9526367187500092149, 0.9531250000000092149, 0.9609375000000078826, 0.9648437500000073275, 0.9667968750000069944, 0.9677734375000067724, 0.9687500000000065503, 0.9765625000000043299, 0.9804687500000031086, 0.9824218750000025535, 0.9833984375000022204, 0.9838867187500022204, 0.9841308593750023315, 0.9843750000000024425, 0.9882812500000022204, 0.9902343750000021094, 0.9912109375000021094, 0.9916992187500019984, 0.9919433593750019984, 0.9921875000000018874, 0.9941406250000014433, 0.9951171875000012212, 0.9956054687500011102, 0.9958496093750011102, 0.9960937500000011102, 0.9970703125000007772, 0.9975585937500005551, 0.9978027343750005551, 0.9980468750000004441, 0.9985351562500003331, 0.9987792968750002220, 0.9989013671875002220, 0.9990234375000002220, 1.000000000000000000 ),
 .UNSPECIFIED. ) ;
#17989 = CARTESIAN_POINT ( 'NONE',  ( -57.57967628038989005, 1.451576601202167360, 1.494865757154131947 ) ) ;
#17990 = CARTESIAN_POINT ( 'NONE',  ( -52.06588384925056801, 19.72955628943436679, -1.003574140810235308E-14 ) ) ;
#17991 = CARTESIAN_POINT ( 'NONE',  ( -0.9075203043614510356, 116.4850453793277865, 0.07935580435194651561 ) ) ;
#17992 = ORIENTED_EDGE ( 'NONE', *, *, #32093, .F. ) ;
#17993 = CARTESIAN_POINT ( 'NONE',  ( -49.37240900658670739, 23.24656341648388036, -0.6295958749597222459 ) ) ;
#17994 = CARTESIAN_POINT ( 'NONE',  ( 5.869729252252017915, 121.2845232542697573, -0.2003997253776844401 ) ) ;
#17995 = CARTESIAN_POINT ( 'NONE',  ( -8.020178813430042908, 121.5755450013093224, 0.8283951592328122615 ) ) ;
#17996 = CARTESIAN_POINT ( 'NONE',  ( 1.144851334150850164, 115.6909491485452719, -1.703252225057385161 ) ) ;
#17997 = CARTESIAN_POINT ( 'NONE',  ( -15.76594527475419483, 145.7191243368997675, -0.6468106390071731715 ) ) ;
#17998 = CARTESIAN_POINT ( 'NONE',  ( 4.475827780916731946, -13.19141740729908108, 3.156716699630707890 ) ) ;
#17999 = CARTESIAN_POINT ( 'NONE',  ( -3.032027503100559240, 117.5448765310053005, 0.5892388327060571473 ) ) ;
#18000 = CARTESIAN_POINT ( 'NONE',  ( 3.682264917456193221, 75.78546620154573077, 0.07358041635423968885 ) ) ;
#18001 = CARTESIAN_POINT ( 'NONE',  ( 8.213135470206557542, 117.5064756823292385, 0.2531991783344220703 ) ) ;
#18002 = CARTESIAN_POINT ( 'NONE',  ( 0.6405796906021217207, 156.3034662015458593, 0.04853048433328251837 ) ) ;
#18003 = LINE ( 'NONE', #5887, #21669 ) ;
#18004 = CARTESIAN_POINT ( 'NONE',  ( 0.1338929724787690234, 25.55936205620983515, 0.9658879472844225100 ) ) ;
#18005 = EDGE_CURVE ( 'NONE', #25703, #1559, #32140, .T. ) ;
#18006 = CARTESIAN_POINT ( 'NONE',  ( -5.774842806153472452, 116.9337168780244696, -0.1296094601971083948 ) ) ;
#18007 = CARTESIAN_POINT ( 'NONE',  ( -45.22172561961857440, 21.28617983374608613, -3.835562791334466315 ) ) ;
#18008 = ORIENTED_EDGE ( 'NONE', *, *, #11000, .F. ) ;
#18009 = DIRECTION ( 'NONE',  ( -0.01997839162482737546, -1.040247600000940825E-18, 0.9998004120163610509 ) ) ;
#18010 = ORIENTED_EDGE ( 'NONE', *, *, #38619, .T. ) ;
#18011 = CARTESIAN_POINT ( 'NONE',  ( 3.713122095021297753, 118.0206735692917022, 0.9242336517888254388 ) ) ;
#18012 = DIRECTION ( 'NONE',  ( -0.8745520943968053684, 0.4849315768086885359, -5.691349986800504491E-16 ) ) ;
#18013 = CARTESIAN_POINT ( 'NONE',  ( 20.44519586420840440, 150.9797539340098069, 2.100688152434085243 ) ) ;
#18014 = CARTESIAN_POINT ( 'NONE',  ( -52.79140191242705527, 11.19429870261168958, -3.959798436811984512 ) ) ;
#18015 = CARTESIAN_POINT ( 'NONE',  ( 18.27466214341546191, 151.8090458617612057, -1.628071726616033388 ) ) ;
#18016 = CARTESIAN_POINT ( 'NONE',  ( 4.581850893073086795, -15.30275035579069254, -0.5110622633019785699 ) ) ;
#18017 = CARTESIAN_POINT ( 'NONE',  ( -22.07768208608597504, 150.1365687424457178, -1.739787554465966668 ) ) ;
#18018 = CARTESIAN_POINT ( 'NONE',  ( 4.900207408254827257, 117.6430132448414270, -0.8582711705238391664 ) ) ;
#18019 = VERTEX_POINT ( 'NONE', #22996 ) ;
#18020 = CARTESIAN_POINT ( 'NONE',  ( -5.925782188533705863, 121.5237468798633955, 0.003878672073842466105 ) ) ;
#18021 = CARTESIAN_POINT ( 'NONE',  ( 3.194259428633707376, -15.59200274161393018, 5.439406988142795107 ) ) ;
#18022 = DIRECTION ( 'NONE',  ( -0.8745520943968250194, 0.4849315768086532863, -5.361993529360574930E-16 ) ) ;
#18023 = CARTESIAN_POINT ( 'NONE',  ( 5.153327614265654333, 56.51694913689138389, 4.640534983550359094 ) ) ;
#18024 = ORIENTED_EDGE ( 'NONE', *, *, #16216, .T. ) ;
#18025 = CARTESIAN_POINT ( 'NONE',  ( 5.835242038117685048, 119.5807162246413498, 1.179424802705185238 ) ) ;
#18026 = DIRECTION ( 'NONE',  ( -5.188838149069472160E-16, 1.699382548006136559E-16, 1.000000000000000000 ) ) ;
#18027 = CARTESIAN_POINT ( 'NONE',  ( -0.7550517280344761772, 118.1535578050699087, -0.9127457894755339751 ) ) ;
#18028 = CARTESIAN_POINT ( 'NONE',  ( -2.352838477949809270, 119.2037781873646622, 0.5921520780602628209 ) ) ;
#18029 = CARTESIAN_POINT ( 'NONE',  ( -7.647780498939813931, -9.906183224868927439, 3.644365410659974991 ) ) ;
#18030 = CARTESIAN_POINT ( 'NONE',  ( 16.01418025823780766, 147.7157881801689427, 1.429122529412921061 ) ) ;
#18031 = DIRECTION ( 'NONE',  ( -0.9998004120163609398, 0.000000000000000000, -0.01997839162482749689 ) ) ;
#18032 = ADVANCED_FACE ( 'NONE', ( #29628 ), #26601, .T. ) ;
#18033 = CIRCLE ( 'NONE', #18704, 0.5080000000000016724 ) ;
#18034 = CARTESIAN_POINT ( 'NONE',  ( 16.59152294496558966, 155.2525159475892167, -0.4418349252515506587 ) ) ;
#18035 = CARTESIAN_POINT ( 'NONE',  ( -24.26619908708080686, 81.70586579672512073, -1.270000000000006235 ) ) ;
#18036 = CARTESIAN_POINT ( 'NONE',  ( -58.36351474529333672, -0.2784124508822488631, 0.09868539478380247698 ) ) ;
#18037 = CARTESIAN_POINT ( 'NONE',  ( -6.057513928997652286, 83.56599999999998829, 1.904999999999996030 ) ) ;
#18038 = CARTESIAN_POINT ( 'NONE',  ( -51.05013135955051951, 14.56862583435632530, 4.678276857666586075 ) ) ;
#18039 = CARTESIAN_POINT ( 'NONE',  ( -3.630816577625875226E-14, 57.14999999999999147, 0.000000000000000000 ) ) ;
#18040 = CARTESIAN_POINT ( 'NONE',  ( -4.157387891345566189, 118.2390912615641838, 0.2342884288663792947 ) ) ;
#18041 = CARTESIAN_POINT ( 'NONE',  ( 3.563983649201253989, 108.3861600575944379, -3.960794436007483821 ) ) ;
#18042 = ORIENTED_EDGE ( 'NONE', *, *, #16476, .T. ) ;
#18043 = EDGE_CURVE ( 'NONE', #39961, #8736, #36449, .T. ) ;
#18044 = CARTESIAN_POINT ( 'NONE',  ( -49.39021242113546606, 17.77731941784099234, 5.290631085210035778 ) ) ;
#18045 = CARTESIAN_POINT ( 'NONE',  ( 6.279405009837805807, 119.8162689779731949, -0.9809252895020896812 ) ) ;
#18046 = DIRECTION ( 'NONE',  ( -0.000000000000000000, -0.000000000000000000, -1.000000000000000000 ) ) ;
#18047 = CARTESIAN_POINT ( 'NONE',  ( 4.279885407778224682, 118.2143666532004715, 0.5181637047333805812 ) ) ;
#18048 = CARTESIAN_POINT ( 'NONE',  ( -9.600854460372945098, 124.0356975489027036, -0.7994020406953789015 ) ) ;
#18049 = CARTESIAN_POINT ( 'NONE',  ( 16.31694223957253698, 121.4173703750124531, 0.3260513381110077824 ) ) ;
#18050 = ORIENTED_EDGE ( 'NONE', *, *, #1565, .T. ) ;
#18051 = CARTESIAN_POINT ( 'NONE',  ( 2.332027132427558769, 25.33165720878049498, 3.998286310156994983 ) ) ;
#18052 = CARTESIAN_POINT ( 'NONE',  ( -5.158718007120306481, 120.8264575521020987, -0.6815868816981844880 ) ) ;
#18053 = CARTESIAN_POINT ( 'NONE',  ( -17.64290547347870941, 83.78857423953914463, 1.269999999999996021 ) ) ;
#18054 = CARTESIAN_POINT ( 'NONE',  ( -46.78765925928225755, 20.34570826442007174, 4.900687844021624606 ) ) ;
#18055 = DIRECTION ( 'NONE',  ( 5.188838149069472160E-16, -1.699382548006136559E-16, -1.000000000000000000 ) ) ;
#18056 = CARTESIAN_POINT ( 'NONE',  ( -6.062687220451711489, 121.4407148395792007, -0.04901857013319344675 ) ) ;
#18057 = EDGE_CURVE ( 'NONE', #10259, #3896, #3231, .T. ) ;
#18058 = CARTESIAN_POINT ( 'NONE',  ( -4.621355134897683570, 27.56591289442953041, -0.4301045952606497025 ) ) ;
#18059 = CARTESIAN_POINT ( 'NONE',  ( 22.82453445504499356, 148.6346580502994073, 1.538154475459325043 ) ) ;
#18060 = FACE_OUTER_BOUND ( 'NONE', #12350, .T. ) ;
#18062 = CARTESIAN_POINT ( 'NONE',  ( 21.16640241758159036, 149.7512365312068709, -1.384406599442889130 ) ) ;
#18061 = CARTESIAN_POINT ( 'NONE',  ( 2.993548201347409510, -14.88003303992029025, 3.932447912750371977 ) ) ;
#18063 = CARTESIAN_POINT ( 'NONE',  ( -2.279834263381315562, 157.4004113605966211, 1.585270110160261758 ) ) ;
#18064 = CARTESIAN_POINT ( 'NONE',  ( -3.632229383214316876, 17.08265688572556584, -2.901706292871565562 ) ) ;
#18065 = CARTESIAN_POINT ( 'NONE',  ( -9.660431270553321070, 118.1749183431956425, -0.7024802509354080016 ) ) ;
#18066 = EDGE_CURVE ( 'NONE', #29132, #5595, #22574, .T. ) ;
#18067 = CARTESIAN_POINT ( 'NONE',  ( 0.9269407327955943021, 12.00036500698010578, 0.3089908296573128932 ) ) ;
#18068 = VERTEX_POINT ( 'NONE', #3655 ) ;
#18069 = CARTESIAN_POINT ( 'NONE',  ( -52.82621711067185544, 9.762356329794503296, 1.302233150175811094 ) ) ;
#18070 = AXIS2_PLACEMENT_3D ( 'NONE', #4216, #33381, #6979 ) ;
#18071 = CARTESIAN_POINT ( 'NONE',  ( -8.072651008563880737, 154.6119571123129788, 0.5584669891872423575 ) ) ;
#18072 = CARTESIAN_POINT ( 'NONE',  ( 5.898638393742167807, -12.20234047945549527, 0.6047796074133310329 ) ) ;
#18073 = CARTESIAN_POINT ( 'NONE',  ( 8.983288137945146801, 154.9128698100208794, -1.355969927742461723 ) ) ;
#18074 = VERTEX_POINT ( 'NONE', #32194 ) ;
#18075 = CARTESIAN_POINT ( 'NONE',  ( 1.357034515785712880, 115.7027987071164574, 1.737102370113531746 ) ) ;
#18076 = CARTESIAN_POINT ( 'NONE',  ( 1.848046085800040483, -15.12359198595263088, 5.521975501593071378 ) ) ;
#18077 = CARTESIAN_POINT ( 'NONE',  ( -4.742396055309614056, 117.8491596531413563, -0.9896183798233539886 ) ) ;
#18078 = CARTESIAN_POINT ( 'NONE',  ( 15.77879114986260589, 146.5725700477668170, 0.1868612039608988085 ) ) ;
#18079 = EDGE_CURVE ( 'NONE', #24559, #11189, #26212, .T. ) ;
#18080 = EDGE_LOOP ( 'NONE', ( #29438, #37809, #29408, #3559 ) ) ;
#18081 = CARTESIAN_POINT ( 'NONE',  ( 7.694773992301578325, 119.4405053107883958, 1.366649582720010025 ) ) ;
#18082 = CARTESIAN_POINT ( 'NONE',  ( -35.99603394726484851, 64.04701136959550922, -1.270000000000009344 ) ) ;
#18083 = DIRECTION ( 'NONE',  ( 6.146657985744592735E-16, 3.905054717696927382E-31, 1.000000000000000000 ) ) ;
#18084 = LINE ( 'NONE', #40490, #7522 ) ;
#18085 = CARTESIAN_POINT ( 'NONE',  ( 13.57554913733958557, 119.6371495169912436, 0.05144635950012921982 ) ) ;
#18086 = CARTESIAN_POINT ( 'NONE',  ( -4.737240446979687825, 56.51500000000003610, -4.914900000000006486 ) ) ;
#18087 = CARTESIAN_POINT ( 'NONE',  ( 1.683587623118159682, -15.20357760260822388, 5.672209996086073680 ) ) ;
#18088 = CARTESIAN_POINT ( 'NONE',  ( -43.82859865241511699, 24.63416949198730421, 1.523999999999993138 ) ) ;
#18089 = CARTESIAN_POINT ( 'NONE',  ( -5.274544067074300457, 115.7029491485454002, 0.8135768287290441325 ) ) ;
#18090 = VECTOR ( 'NONE', #37917, 1000.000000000000114 ) ;
#18091 = EDGE_CURVE ( 'NONE', #4125, #32297, #39216, .T. ) ;
#18092 = CARTESIAN_POINT ( 'NONE',  ( -4.640960256449444543, 117.9807172536480238, 0.7263108157050279790 ) ) ;
#18093 = VECTOR ( 'NONE', #5863, 1000.000000000000114 ) ;
#18094 = VERTEX_POINT ( 'NONE', #465 ) ;
#18095 = EDGE_LOOP ( 'NONE', ( #23085, #23569, #21695, #2803 ) ) ;
#18096 = CARTESIAN_POINT ( 'NONE',  ( -4.974399692199978240, 117.4065978902591354, 0.8873519537265817103 ) ) ;
#18097 = CARTESIAN_POINT ( 'NONE',  ( -5.764161295553385855, 118.7617298297994637, -1.235935067645903329 ) ) ;
#18098 = CARTESIAN_POINT ( 'NONE',  ( 0.1065646865915093611, 105.8844662015456777, -5.332932678536313809 ) ) ;
#18099 = CARTESIAN_POINT ( 'NONE',  ( 4.752655214354502888, 117.6359145343736117, 1.138150416757013339 ) ) ;
#18100 = CARTESIAN_POINT ( 'NONE',  ( -11.97180806971932299, 56.20439414705996484, -5.016499999999999737 ) ) ;
#18101 = CARTESIAN_POINT ( 'NONE',  ( -0.4103500344927140664, 124.0591982226670211, 0.08506156519360540125 ) ) ;
#18102 = CARTESIAN_POINT ( 'NONE',  ( 0.09481320634720795393, -4.229605868409334057, 4.636458411128852930 ) ) ;
#18103 = CARTESIAN_POINT ( 'NONE',  ( 4.889703507614793665, 117.4101837603834468, -0.9754936775373431734 ) ) ;
#18104 = CARTESIAN_POINT ( 'NONE',  ( -17.64290547347870941, 83.78857423953914463, -1.524000000000003130 ) ) ;
#18105 = CARTESIAN_POINT ( 'NONE',  ( 3.377503200524144322, -12.59127376242380514, 1.184662976626496000 ) ) ;
#18106 = CARTESIAN_POINT ( 'NONE',  ( 5.249845242698079062, 116.4925209815607730, -0.8804580864248582328 ) ) ;
#18107 = CARTESIAN_POINT ( 'NONE',  ( -4.445868218450056197, 29.55296359113615523, 3.403299529360248599 ) ) ;
#18108 = CARTESIAN_POINT ( 'NONE',  ( -0.7131320481206968598, 115.7031549148529734, 1.731730113216342071 ) ) ;
#18109 = CARTESIAN_POINT ( 'NONE',  ( 1.790774717077139089, 25.13178105314743860, 4.274281468382033822 ) ) ;
#18110 = ORIENTED_EDGE ( 'NONE', *, *, #41205, .T. ) ;
#18111 = CARTESIAN_POINT ( 'NONE',  ( -4.808149584360944750, 104.6144662015457527, 0.4147572885131461939 ) ) ;
#18112 = CARTESIAN_POINT ( 'NONE',  ( 3.591698533489739553, -15.62560650602327961, 3.738647084555763112 ) ) ;
#18113 = CARTESIAN_POINT ( 'NONE',  ( -5.881924083617415810, 119.0696708348911699, 0.9594134845634217923 ) ) ;
#18114 = CARTESIAN_POINT ( 'NONE',  ( -0.7486558104752240039, 25.82057725623272759, -0.6268360674696834556 ) ) ;
#18115 = EDGE_CURVE ( 'NONE', #31840, #37188, #13439, .T. ) ;
#18116 = CARTESIAN_POINT ( 'NONE',  ( -0.4721710868402241301, 14.98625149489145159, 0.8573358612705738180 ) ) ;
#18117 = ORIENTED_EDGE ( 'NONE', *, *, #2385, .T. ) ;
#18118 = VERTEX_POINT ( 'NONE', #26425 ) ;
#18119 = PLANE ( 'NONE',  #9113 ) ;
#18120 = CARTESIAN_POINT ( 'NONE',  ( 1.600579373209928269, 119.3928400758114918, 0.6828601607076615343 ) ) ;
#18121 = CARTESIAN_POINT ( 'NONE',  ( -8.566376370482908342, 122.4751019636825049, 0.6322842599711311351 ) ) ;
#18122 = DIRECTION ( 'NONE',  ( -1.000000000000000000, 0.000000000000000000, 0.000000000000000000 ) ) ;
#18123 = CARTESIAN_POINT ( 'NONE',  ( 3.247910276010201880, -14.18928037215049009, 3.960261243354706640 ) ) ;
#18124 = CARTESIAN_POINT ( 'NONE',  ( 18.19397457907784599, 146.9188445454784357, -1.620492285849223224 ) ) ;
#18125 = CARTESIAN_POINT ( 'NONE',  ( 0.03153870137009017610, 158.4432089348667319, -1.578325583784927932 ) ) ;
#18126 = DIRECTION ( 'NONE',  ( 5.188838149069472160E-16, -1.699382548006136559E-16, -1.000000000000000000 ) ) ;
#18127 = CARTESIAN_POINT ( 'NONE',  ( 4.119003220443754110, 118.2429491485453354, -0.1854851255534567256 ) ) ;
#18128 = CARTESIAN_POINT ( 'NONE',  ( 0.003052472355804966304, 120.8426702770480148, -0.1527581987772200500 ) ) ;
#18129 = CIRCLE ( 'NONE', #21525, 0.2540000000000006142 ) ;
#18130 = VERTEX_POINT ( 'NONE', #25998 ) ;
#18131 = CARTESIAN_POINT ( 'NONE',  ( 2.930607426163104545, -14.92094031927118714, 4.083576684136651203 ) ) ;
#18132 = CARTESIAN_POINT ( 'NONE',  ( 10.63219908769121247, 56.50600268266116188, -5.016500000000110759 ) ) ;
#18133 = CARTESIAN_POINT ( 'NONE',  ( -57.50985127144491571, 1.621858126761932084, 1.632528232186438721 ) ) ;
#18134 = CARTESIAN_POINT ( 'NONE',  ( -0.05192310401019068627, -8.293124787585329116, 4.627658001227512585 ) ) ;
#18135 = CARTESIAN_POINT ( 'NONE',  ( 0.7424407951589586663, 156.5584078035761593, 0.9879031837870264621 ) ) ;
#18136 = CARTESIAN_POINT ( 'NONE',  ( 0.06674422508556764055, 33.39646256408616409, 3.182828529663568773 ) ) ;
#18137 = CARTESIAN_POINT ( 'NONE',  ( -2.817215192601065787, 108.0685014782224442, 4.280041469292686251 ) ) ;
#18138 = AXIS2_PLACEMENT_3D ( 'NONE', #34977, #11747, #5379 ) ;
#18139 = CARTESIAN_POINT ( 'NONE',  ( -4.627450822138572839, 2.892058097378844117, -0.1328416527703782657 ) ) ;
#18140 = CARTESIAN_POINT ( 'NONE',  ( 14.16569067496505774, 138.8670163227233161, 0.2830642121559648339 ) ) ;
#18141 = CARTESIAN_POINT ( 'NONE',  ( -2.830841276205400270, 0.8888151952923978305, 7.984752373722160179 ) ) ;
#18142 = CARTESIAN_POINT ( 'NONE',  ( -57.61542428582638564, 1.103772655929896596, -0.1998674755708677864 ) ) ;
#18143 = CARTESIAN_POINT ( 'NONE',  ( 5.522311800473831411, 117.0453351255057726, -0.4840448646347706441 ) ) ;
#18144 = CIRCLE ( 'NONE', #35178, 0.6350000000000001199 ) ;
#18145 = DIRECTION ( 'NONE',  ( 5.188838149069472160E-16, -1.699382548006136559E-16, -1.000000000000000000 ) ) ;
#18146 = DIRECTION ( 'NONE',  ( -0.9998501190848635423, -0.01731298258487451447, -5.158639060800523934E-16 ) ) ;
#18147 = CARTESIAN_POINT ( 'NONE',  ( -5.495523183683927115, 31.57050297546189199, 3.325088329614593885 ) ) ;
#18148 = CARTESIAN_POINT ( 'NONE',  ( 4.037907715354051241, 27.70556447992504445, -2.267523456217593214 ) ) ;
#18149 = DIRECTION ( 'NONE',  ( 9.627370216492862708E-17, 1.000000000000000000, -0.000000000000000000 ) ) ;
#18150 = CARTESIAN_POINT ( 'NONE',  ( -5.078986093043186045, 98.39146620154573952, -0.1014902294541237954 ) ) ;
#18151 = CARTESIAN_POINT ( 'NONE',  ( -58.83227707057488232, -0.08366279997998327111, -1.543674587295873857E-14 ) ) ;
#18152 = CARTESIAN_POINT ( 'NONE',  ( 0.2204105866771658151, 106.6745790697264056, -5.009819746185714351 ) ) ;
#18153 = CARTESIAN_POINT ( 'NONE',  ( -15.73021646601979384, 121.2535323456646523, 0.2080526303901672758 ) ) ;
#18154 = VECTOR ( 'NONE', #5615, 1000.000000000000000 ) ;
#18155 = ORIENTED_EDGE ( 'NONE', *, *, #38651, .T. ) ;
#18156 = CARTESIAN_POINT ( 'NONE',  ( -58.60381103753274346, 0.5214191424347813797, -0.2072982876684605347 ) ) ;
#18157 = ORIENTED_EDGE ( 'NONE', *, *, #18596, .F. ) ;
#18158 = FACE_OUTER_BOUND ( 'NONE', #11905, .T. ) ;
#18159 = CARTESIAN_POINT ( 'NONE',  ( -10.18105065676974519, 125.9743313966586129, -0.2034416216762104657 ) ) ;
#18160 = CARTESIAN_POINT ( 'NONE',  ( 6.376069600431401696, -13.97715805579494130, 0.6469259796868158663 ) ) ;
#18161 = CARTESIAN_POINT ( 'NONE',  ( -17.34031924846188133, 128.5728276651957742, 1.378292450406111147 ) ) ;
#18162 = CARTESIAN_POINT ( 'NONE',  ( 21.01108318401065134, 151.1643092826112138, -1.006483555388256068 ) ) ;
#18163 = CARTESIAN_POINT ( 'NONE',  ( 4.636458409304901274, 17.36039413176390411, -0.09481320587925551324 ) ) ;
#18164 = CARTESIAN_POINT ( 'NONE',  ( -17.01700507317055511, 122.6950552906510694, -0.6769824155666206433 ) ) ;
#18165 = CARTESIAN_POINT ( 'NONE',  ( -50.50202955377455538, 15.48282070406618338, -4.812845866082358981 ) ) ;
#18166 = VERTEX_POINT ( 'NONE', #39007 ) ;
#18167 = CARTESIAN_POINT ( 'NONE',  ( 5.562220668319040939, 116.6985801738751292, 0.1494643777500437865 ) ) ;
#18168 = DIRECTION ( 'NONE',  ( 0.7548010569845216011, 0.6559537821943317581, 2.801824109679580762E-16 ) ) ;
#18169 = CARTESIAN_POINT ( 'NONE',  ( -15.51360955034724043, 150.7699688800196611, 1.541415763164774466 ) ) ;
#18170 = CARTESIAN_POINT ( 'NONE',  ( -54.85593356636119466, 7.111675983978352100, -3.067722010356754403 ) ) ;
#18171 = CARTESIAN_POINT ( 'NONE',  ( 14.27152401005723448, 125.7140216354555804, -1.459898031787023376 ) ) ;
#18172 = CARTESIAN_POINT ( 'NONE',  ( -12.00897459848981796, 120.6765805525287334, -1.550193712165490956 ) ) ;
#18173 = CARTESIAN_POINT ( 'NONE',  ( -55.11216289415786207, 6.786895728730008237, -3.177266426849177705 ) ) ;
#18174 = AXIS2_PLACEMENT_3D ( 'NONE', #6579, #38748, #15527 ) ;
#18175 = CARTESIAN_POINT ( 'NONE',  ( 10.46017523140576344, 124.8149993102252182, -0.6249645713522342660 ) ) ;
#18176 = ORIENTED_EDGE ( 'NONE', *, *, #36658, .T. ) ;
#18177 = CARTESIAN_POINT ( 'NONE',  ( -11.01279815837321863, 154.4909003399924643, -2.068435761307119147 ) ) ;
#18178 = CARTESIAN_POINT ( 'NONE',  ( 3.827285340041869155, -15.59443631323044421, 3.224486442507772388 ) ) ;
#18179 = CARTESIAN_POINT ( 'NONE',  ( -4.455953229021707429, 118.1125578900950757, -0.7543243153411564039 ) ) ;
#18180 = CARTESIAN_POINT ( 'NONE',  ( -57.43854689232674815, 1.757847328446624058, -1.624773336220253217 ) ) ;
#18181 = TOROIDAL_SURFACE ( 'NONE', #36488, 3.683000000000000718, 0.5080000000000000071 ) ;
#18182 = DIRECTION ( 'NONE',  ( -0.8745520943968241312, 0.4849315768086548406, -5.691349986800536046E-16 ) ) ;
#18183 = CARTESIAN_POINT ( 'NONE',  ( 15.43964774321182354, 150.7699688800196611, 2.159935508548367356 ) ) ;
#18184 = CARTESIAN_POINT ( 'NONE',  ( 0.02537255736346701387, 39.20946620154573736, -1.269746523260778970 ) ) ;
#18185 = CARTESIAN_POINT ( 'NONE',  ( -5.045332104996713696, -5.333490553104357268, 6.775881858851239947 ) ) ;
#18186 = CARTESIAN_POINT ( 'NONE',  ( 14.74011517316798248, 148.8440819608433969, 0.7404754567584960201 ) ) ;
#18187 = CARTESIAN_POINT ( 'NONE',  ( 4.801216665947148243, 117.4032681888235459, -1.015537427445656782 ) ) ;
#18188 =( BOUNDED_CURVE ( )  B_SPLINE_CURVE ( 3, ( #28805, #22383, #36043, #38812 ),
 .UNSPECIFIED., .F., .T. ) 
 B_SPLINE_CURVE_WITH_KNOTS ( ( 4, 4 ),
 ( 0.000000000000000000, 1.570796326794895226 ),
 .UNSPECIFIED. ) 
 CURVE ( )  GEOMETRIC_REPRESENTATION_ITEM ( )  RATIONAL_B_SPLINE_CURVE ( ( 1.000000000000000000, 0.8047378541243652705, 0.8047378541243652705, 1.000000000000000000 ) ) 
 REPRESENTATION_ITEM ( '' )  );
#18189 = DIRECTION ( 'NONE',  ( -0.5149185422762213582, 0.8572391118119444542, 6.416759367969739335E-15 ) ) ;
#18190 = CARTESIAN_POINT ( 'NONE',  ( -3.931412874456751361, 118.1588900401562938, 0.5787760988833658971 ) ) ;
#18191 = CARTESIAN_POINT ( 'NONE',  ( -6.559134203278485842, 78.24119908707510263, 1.270000000000002682 ) ) ;
#18192 = CIRCLE ( 'NONE', #42048, 16.60960244842765832 ) ;
#18193 = CARTESIAN_POINT ( 'NONE',  ( -57.80191396384030611, 0.8575073823135492823, 0.7186190270693690874 ) ) ;
#18194 = CARTESIAN_POINT ( 'NONE',  ( -49.65119436432973998, 19.91503915004672720, 3.137105223390890263 ) ) ;
#18195 = CARTESIAN_POINT ( 'NONE',  ( -23.09707919911562612, 149.8924475812327159, -0.2317116236470734003 ) ) ;
#18196 = ORIENTED_EDGE ( 'NONE', *, *, #15927, .T. ) ;
#18197 = CARTESIAN_POINT ( 'NONE',  ( -51.02231935970569054, 20.76374992004582154, -0.7877321375940368187 ) ) ;
#18198 = CARTESIAN_POINT ( 'NONE',  ( 7.924075518182773337, 122.0230495997628140, -0.6113557723677206512 ) ) ;
#18199 = CARTESIAN_POINT ( 'NONE',  ( -8.072253591115543969, 121.3304565451442727, 0.9161511751190034580 ) ) ;
#18200 = VERTEX_POINT ( 'NONE', #9817 ) ;
#18201 = CARTESIAN_POINT ( 'NONE',  ( 1.648710697724705687, 115.6909491485466646, -1.667653344520376724 ) ) ;
#18202 = CARTESIAN_POINT ( 'NONE',  ( -15.27538331669057570, 143.4753230507764670, -0.6393389556987904010 ) ) ;
#18203 = CARTESIAN_POINT ( 'NONE',  ( 5.309946395046844181, -12.59883844183437596, 1.960244440597288529 ) ) ;
#18204 = CARTESIAN_POINT ( 'NONE',  ( -21.68724320794237670, 149.9601031839316079, 1.147785971009648298 ) ) ;
#18205 = CARTESIAN_POINT ( 'NONE',  ( -8.216341275949833545, 69.50096819940942794, 1.270000000000003348 ) ) ;
#18206 = CARTESIAN_POINT ( 'NONE',  ( 20.41771265994151463, 129.0384130229076334, 0.5332683426449600361 ) ) ;
#18207 = CARTESIAN_POINT ( 'NONE',  ( 3.768629899957671281, 121.0935559710094509, 0.1102337842458726014 ) ) ;
#18208 = FACE_OUTER_BOUND ( 'NONE', #27155, .T. ) ;
#18209 = CARTESIAN_POINT ( 'NONE',  ( 0.03997419820544263758, 30.08235846857972007, -0.9743396344490610206 ) ) ;
#18210 = CARTESIAN_POINT ( 'NONE',  ( 0.0002734175338603746100, 159.6054662015457382, -0.01368293144939978188 ) ) ;
#18211 = CARTESIAN_POINT ( 'NONE',  ( -42.24009380985435058, 22.39526060921979678, -1.717801299055324415 ) ) ;
#18212 = DIRECTION ( 'NONE',  ( -0.8572391118119510045, -0.5149185422762100339, -3.573031421855330583E-16 ) ) ;
#18213 = EDGE_LOOP ( 'NONE', ( #14513, #20784, #19171, #8721, #17575 ) ) ;
#18214 = CARTESIAN_POINT ( 'NONE',  ( 6.037009026191382688, 118.8442016224334594, 1.226040081825612527 ) ) ;
#18215 = DIRECTION ( 'NONE',  ( 0.6594218222380271444, 0.7517731442105921591, -2.068700233264622195E-15 ) ) ;
#18216 = CARTESIAN_POINT ( 'NONE',  ( 21.32959265000921434, 150.3702682424204511, 2.003547396033109607 ) ) ;
#18217 = CARTESIAN_POINT ( 'NONE',  ( -58.41956937744169664, -0.3672969284050977001, -0.3776070891688105280 ) ) ;
#18218 = CARTESIAN_POINT ( 'NONE',  ( 20.44439181834784236, 148.1475078817917961, -1.665223645801947594 ) ) ;
#18219 = CARTESIAN_POINT ( 'NONE',  ( 7.630415381941168640, 23.66608445915806058, -3.560124470299026900 ) ) ;
#18220 = CARTESIAN_POINT ( 'NONE',  ( -2.036215858770317855, 117.3535355059730705, -0.5825239229278258435 ) ) ;
#18221 = CARTESIAN_POINT ( 'NONE',  ( 4.833494790946907038, 117.7366326795467586, -0.8572946300570807310 ) ) ;
#18222 = CARTESIAN_POINT ( 'NONE',  ( 7.089375086749911681, 122.4291926079955317, 0.2513136963589434059 ) ) ;
#18223 = EDGE_LOOP ( 'NONE', ( #2862, #28831, #17254, #22493, #30912, #31809, #26320, #36234, #16240, #13002, #34580, #24504 ) ) ;
#18224 = CARTESIAN_POINT ( 'NONE',  ( -15.79579396213704001, 146.5797798787131399, -0.08547097745249035428 ) ) ;
#18225 = CARTESIAN_POINT ( 'NONE',  ( -15.41952259888553911, 128.5596447653542498, -2.179146846741407906 ) ) ;
#18226 = CARTESIAN_POINT ( 'NONE',  ( 2.659284927817582744, -15.52939239755456136, 5.761088356787748666 ) ) ;
#18227 = DIRECTION ( 'NONE',  ( -0.8745520943968240202, 0.4849315768086551737, -5.361993529360572958E-16 ) ) ;
#18228 =( GEOMETRIC_REPRESENTATION_CONTEXT ( 3 ) GLOBAL_UNCERTAINTY_ASSIGNED_CONTEXT ( ( #29540 ) ) GLOBAL_UNIT_ASSIGNED_CONTEXT ( ( #10690, #14923, #5583 ) ) REPRESENTATION_CONTEXT ( 'NONE', 'WORKASPACE' ) );
#18229 = CARTESIAN_POINT ( 'NONE',  ( -4.367291737180500455, 117.9496054766628674, -1.181649046108978585 ) ) ;
#18230 = ORIENTED_EDGE ( 'NONE', *, *, #12927, .T. ) ;
#18231 = CARTESIAN_POINT ( 'NONE',  ( -0.01133701094408546065, 119.0130636887059410, 0.5673503866435171128 ) ) ;
#18232 = CARTESIAN_POINT ( 'NONE',  ( -5.332935397695336199, 105.1224662015457199, -0.1065647409268299373 ) ) ;
#18233 = CARTESIAN_POINT ( 'NONE',  ( -5.328528283132492938, 115.6909491485453003, -0.4166226019199130159 ) ) ;
#18234 = CARTESIAN_POINT ( 'NONE',  ( -1.600813358578796031, 118.7759820277219944, 0.7642889039740425883 ) ) ;
#18235 = CARTESIAN_POINT ( 'NONE',  ( -7.266063235143556120, -1.810023253287891487, -4.326994388187479501 ) ) ;
#18236 = CARTESIAN_POINT ( 'NONE',  ( 5.869717882709199586, 121.2452591720019370, 0.5958057796325609834 ) ) ;
#18237 = CARTESIAN_POINT ( 'NONE',  ( -4.787624606785451320, 118.5930653697794384, -0.9408880203060064895 ) ) ;
#18238 = CARTESIAN_POINT ( 'NONE',  ( 6.914686169612705768, 117.4533518774869947, -0.3713220847589204787 ) ) ;
#18239 = VECTOR ( 'NONE', #36039, 1000.000000000000000 ) ;
#18240 = CARTESIAN_POINT ( 'NONE',  ( -58.36378379890241774, -0.2789760973723339754, 0.09651987913409887376 ) ) ;
#18241 = CARTESIAN_POINT ( 'NONE',  ( -30.30981065340567682, 56.20484928103341815, -1.524000000000004462 ) ) ;
#18242 = CARTESIAN_POINT ( 'NONE',  ( 2.081461833008364515, -15.42522581128936210, 5.972092850182500356 ) ) ;
#18243 = CARTESIAN_POINT ( 'NONE',  ( -4.171376165246405421, 118.2392936340378498, 0.2183368768271861937 ) ) ;
#18244 = CARTESIAN_POINT ( 'NONE',  ( -18.86374853661781970, 125.3403196291361610, -0.3769425889880997360 ) ) ;
#18245 = ORIENTED_EDGE ( 'NONE', *, *, #6574, .F. ) ;
#18246 = CARTESIAN_POINT ( 'NONE',  ( -48.56815661899837977, 19.24492339269602681, 5.224590812749973168 ) ) ;
#18247 = CARTESIAN_POINT ( 'NONE',  ( 4.336810308868679797, 119.4260466530178348, -0.7558801875816598681 ) ) ;
#18248 = CARTESIAN_POINT ( 'NONE',  ( -6.589702033682734540E-14, 87.97746620154572383, -4.338478393988997516E-18 ) ) ;
#18249 = CARTESIAN_POINT ( 'NONE',  ( 4.426091836488892817, 118.1635172220246517, 0.6237344508278885868 ) ) ;
#18250 = CARTESIAN_POINT ( 'NONE',  ( -4.418888662852294757, 155.8637389808261275, -0.7167756870077639508 ) ) ;
#18251 = PRODUCT_DEFINITION_FORMATION_WITH_SPECIFIED_SOURCE ( 'ANY', '', #20129, .NOT_KNOWN. ) ;
#18252 = LINE ( 'NONE', #40657, #26754 ) ;
#18253 = CARTESIAN_POINT ( 'NONE',  ( 6.894732321505262718, 117.1676844715483270, 0.1377731603346603051 ) ) ;
#18254 = EDGE_CURVE ( 'NONE', #926, #15317, #6632, .T. ) ;
#18255 = ORIENTED_EDGE ( 'NONE', *, *, #25087, .T. ) ;
#18256 = CARTESIAN_POINT ( 'NONE',  ( -2.755274729907521980, 20.69627551736597226, -3.746277899328600558 ) ) ;
#18257 = CARTESIAN_POINT ( 'NONE',  ( -17.14500000000466784, 71.11999999999886768, -1.270000000000000684 ) ) ;
#18258 = DIRECTION ( 'NONE',  ( 5.188838149069472160E-16, -1.699382548006136559E-16, -1.000000000000000000 ) ) ;
#18259 = CYLINDRICAL_SURFACE ( 'NONE', #4749, 9.048749999999998295 ) ;
#18260 = CARTESIAN_POINT ( 'NONE',  ( 7.788361015690092870, 122.6175610730192176, 0.07939682999910972760 ) ) ;
#18261 = CARTESIAN_POINT ( 'NONE',  ( 6.070467230626295674, 121.4441374072678883, 0.2166268477916202806 ) ) ;
#18262 = CIRCLE ( 'NONE', #22324, 0.3810000000000015041 ) ;
#18263 = CARTESIAN_POINT ( 'NONE',  ( -2.133573495637306916, 19.78131850274109382, 4.120466288703205748 ) ) ;
#18264 = CARTESIAN_POINT ( 'NONE',  ( 22.70157303802166737, 149.4207734315791072, 1.531927632650241788 ) ) ;
#18265 = CARTESIAN_POINT ( 'NONE',  ( -4.502681726546150287, 104.6144662015457811, -1.767325709528040134 ) ) ;
#18267 = CARTESIAN_POINT ( 'NONE',  ( 20.87437586479479634, 150.1670661137953289, -1.386469220648549383 ) ) ;
#18266 = CARTESIAN_POINT ( 'NONE',  ( 3.178324225997528618, -14.33742748831649827, 1.935164598152447679 ) ) ;
#18268 = CARTESIAN_POINT ( 'NONE',  ( -10.29797255167336978, 122.2012759285571946, 1.140151759267314269 ) ) ;
#18269 = AXIS2_PLACEMENT_3D ( 'NONE', #20518, #11157, #36329 ) ;
#18270 = CARTESIAN_POINT ( 'NONE',  ( 2.838909340336904563, 21.51804255560577772, 3.663749385350952181 ) ) ;
#18271 = CARTESIAN_POINT ( 'NONE',  ( -22.90231444567494989, 149.5023856264156450, -1.310353656364537045 ) ) ;
#18272 = CARTESIAN_POINT ( 'NONE',  ( -0.9107729336552147226, 17.84451472381387305, 0.3451692354151053577 ) ) ;
#18273 = EDGE_LOOP ( 'NONE', ( #12593, #672, #8893, #20684 ) ) ;
#18274 = EDGE_CURVE ( 'NONE', #32282, #19659, #23203, .T. ) ;
#18275 = CARTESIAN_POINT ( 'NONE',  ( -56.88731995051697510, 2.378615435641926013, -9.753004163756391309E-15 ) ) ;
#18276 = CARTESIAN_POINT ( 'NONE',  ( -9.401300499464442240, 153.8930958044198576, 0.5598851911991608032 ) ) ;
#18277 = CARTESIAN_POINT ( 'NONE',  ( 3.566861488287894844, -14.88765406650577283, 5.398167181214303945 ) ) ;
#18278 = CARTESIAN_POINT ( 'NONE',  ( 7.304865317682085468, 121.1388872696715282, -0.8066302172824779682 ) ) ;
#18279 = EDGE_LOOP ( 'NONE', ( #32284, #1371 ) ) ;
#18280 = CARTESIAN_POINT ( 'NONE',  ( 1.556864280699287395, 115.7027529739286535, 1.730863229191432318 ) ) ;
#18281 = ORIENTED_EDGE ( 'NONE', *, *, #9754, .F. ) ;
#18282 = CARTESIAN_POINT ( 'NONE',  ( -4.649178111515271716, 117.8875442298166831, -1.000802408407167166 ) ) ;
#18283 = CARTESIAN_POINT ( 'NONE',  ( 15.77201034003348745, 145.9134097338176730, 0.1865891569459579291 ) ) ;
#18284 = EDGE_LOOP ( 'NONE', ( #37784, #7194 ) ) ;
#18285 = CARTESIAN_POINT ( 'NONE',  ( 8.897726962874816792, 119.7003323559047061, 1.444919796022273273 ) ) ;
#18286 = DIRECTION ( 'NONE',  ( -4.017660918040594346E-17, 1.000000000000000000, 2.376309959284834438E-19 ) ) ;
#18287 = DIRECTION ( 'NONE',  ( -0.000000000000000000, -0.000000000000000000, -1.000000000000000000 ) ) ;
#18288 = ADVANCED_FACE ( 'NONE', ( #35814 ), #17083, .T. ) ;
#18289 = CARTESIAN_POINT ( 'NONE',  ( 0.02969003158472036108, 157.1787724364823760, -1.485810588193620552 ) ) ;
#18290 = CARTESIAN_POINT ( 'NONE',  ( 22.50450395291942129, 150.7830971219523519, 0.1219060866366472456 ) ) ;
#18291 = EDGE_CURVE ( 'NONE', #22322, #9160, #32610, .T. ) ;
#18292 = CIRCLE ( 'NONE', #17630, 0.5080000000000002292 ) ;
#18293 = CARTESIAN_POINT ( 'NONE',  ( 0.09909826073474366226, 106.8097931225389488, -4.959282197179095242 ) ) ;
#18294 = EDGE_CURVE ( 'NONE', #8452, #5595, #41586, .T. ) ;
#18295 = CARTESIAN_POINT ( 'NONE',  ( 1.881137653242185959, -15.44088361928680442, 5.378024698638343537 ) ) ;
#18296 = CARTESIAN_POINT ( 'NONE',  ( 10.79307885933830136, 57.10041794475090171, 5.016499999999999737 ) ) ;
#18297 = LINE ( 'NONE', #31296, #36862 ) ;
#18298 = CARTESIAN_POINT ( 'NONE',  ( -4.757343136932370875, 117.8474671740875550, 0.8187060929519298647 ) ) ;
#18299 = EDGE_LOOP ( 'NONE', ( #28599, #12539, #10799, #24463 ) ) ;
#18300 = DIRECTION ( 'NONE',  ( 0.8745520943968235761, -0.4849315768086558398, 4.268512490100410909E-16 ) ) ;
#18301 = CARTESIAN_POINT ( 'NONE',  ( -3.208471139890875179, 118.3820369523956941, -0.9069343936787985783 ) ) ;
#18302 = CARTESIAN_POINT ( 'NONE',  ( -4.850755190081010859, 117.2937442104795593, -0.9187341308512858573 ) ) ;
#18303 = CARTESIAN_POINT ( 'NONE',  ( 4.744653392920721302, 117.6672350140714229, 1.125260125251866583 ) ) ;
#18304 = CARTESIAN_POINT ( 'NONE',  ( -11.62920297224728827, 55.59919541886078065, -5.016500000000107207 ) ) ;
#18305 = CARTESIAN_POINT ( 'NONE',  ( -0.7705677718992680614, 119.3684187487962305, 0.7342037314787066560 ) ) ;
#18306 = CYLINDRICAL_SURFACE ( 'NONE', #9089, 9.048749999999998295 ) ;
#18307 = CARTESIAN_POINT ( 'NONE',  ( -52.32205026661357294, 13.67230311332622072, 4.407798173677520914 ) ) ;
#18308 = DIRECTION ( 'NONE',  ( -4.017660918040594346E-17, 1.000000000000000000, 2.376309959284834438E-19 ) ) ;
#18309 = CARTESIAN_POINT ( 'NONE',  ( 2.845270837621566518, -14.55731563485390723, 4.954299782322259205 ) ) ;
#18310 = CARTESIAN_POINT ( 'NONE',  ( 0.3027292972882736910, 105.9597790263619146, -5.298406829468305546 ) ) ;
#18311 = CARTESIAN_POINT ( 'NONE',  ( -5.087176912069907075, 120.2090573957402455, -0.9271508619376559457 ) ) ;
#18312 = B_SPLINE_CURVE_WITH_KNOTS ( 'NONE', 3,
 ( #33405, #30195, #14206, #822, #7421, #24002, #1036, #36812 ),
 .UNSPECIFIED., .F., .F.,
 ( 4, 2, 2, 4 ),
 ( 0.000000000000000000, 0.1320084156803643383, 0.1980126235205464935, 0.2567263020195166834 ),
 .UNSPECIFIED. ) ;
#18313 = CARTESIAN_POINT ( 'NONE',  ( -17.64950171984354199, 84.16951713491046405, -1.270000000000003126 ) ) ;
#18314 = LINE ( 'NONE', #31954, #32608 ) ;
#18315 = CARTESIAN_POINT ( 'NONE',  ( -0.5072216500879573875, 115.7034658939820417, 1.744308663346807897 ) ) ;
#18316 = CARTESIAN_POINT ( 'NONE',  ( 4.585487687326599726, 17.13547844546973309, 0.5842699607688729424 ) ) ;
#18318 = ORIENTED_EDGE ( 'NONE', *, *, #564, .F. ) ;
#18317 = CARTESIAN_POINT ( 'NONE',  ( 23.20005416489656724, 148.7951734159264561, 1.060305963766563053 ) ) ;
#18319 = CARTESIAN_POINT ( 'NONE',  ( 2.418018609469429148, 104.6144662015533555, -4.757618545730919024 ) ) ;
#18320 = CARTESIAN_POINT ( 'NONE',  ( 2.046246934637348858, -15.60107924929197942, 5.318501171315276999 ) ) ;
#18321 = CARTESIAN_POINT ( 'NONE',  ( -4.191956958763880969, 119.0775769483117870, 0.8365378509937178020 ) ) ;
#18322 = CARTESIAN_POINT ( 'NONE',  ( 0.8739363859948088287, 22.79536383596403226, -0.4369566804381688208 ) ) ;
#18323 = CARTESIAN_POINT ( 'NONE',  ( -0.1409938471676187022, 25.13008524939761656, 0.9676832235670267401 ) ) ;
#18324 = VERTEX_POINT ( 'NONE', #30666 ) ;
#18325 = TOROIDAL_SURFACE ( 'NONE', #19698, 0.7620000000000000107, 0.2540000000000000036 ) ;
#18326 = VERTEX_POINT ( 'NONE', #20857 ) ;
#18327 = LINE ( 'NONE', #8765, #22829 ) ;
#18328 = CARTESIAN_POINT ( 'NONE',  ( 2.259516459295608737, 118.2243428780609662, 0.9293431707136512454 ) ) ;
#18329 = CARTESIAN_POINT ( 'NONE',  ( -10.43918028506331730, 123.9810924921358151, 0.8290978625009026715 ) ) ;
#18330 = DIRECTION ( 'NONE',  ( -1.224646799147353207E-16, -7.780346281855952181E-32, 1.000000000000000000 ) ) ;
#18331 = CARTESIAN_POINT ( 'NONE',  ( 3.201139452527619333, -14.28037012539873274, 4.574913560108570643 ) ) ;
#18332 = CARTESIAN_POINT ( 'NONE',  ( 0.5282936316506747776, 119.4440140289964774, -0.5434071943388011361 ) ) ;
#18333 = CARTESIAN_POINT ( 'NONE',  ( -2.584978638890317537, 158.3255140430775043, -1.682483135129622998 ) ) ;
#18334 = DIRECTION ( 'NONE',  ( -1.000000000000000000, -1.092739197465705287E-15, 0.000000000000000000 ) ) ;
#18335 = CARTESIAN_POINT ( 'NONE',  ( -10.39928917620371784, 153.1223395828141918, -0.2078025466733117443 ) ) ;
#18336 = CARTESIAN_POINT ( 'NONE',  ( 4.123474937902314785, 118.2429491485453354, -0.1804386993445105669 ) ) ;
#18337 = CARTESIAN_POINT ( 'NONE',  ( 9.835128631861913107, 124.8790005272986861, -0.1409026022053573302 ) ) ;
#18338 = EDGE_CURVE ( 'NONE', #15239, #40888, #17463, .T. ) ;
#18339 = ORIENTED_EDGE ( 'NONE', *, *, #40728, .T. ) ;
#18340 = CARTESIAN_POINT ( 'NONE',  ( 2.831922340016455042, -13.93067033233365315, 0.4309514144534042912 ) ) ;
#18341 = CARTESIAN_POINT ( 'NONE',  ( -5.885917553499150578, 77.12042444889114279, 1.270000000000003348 ) ) ;
#18342 = CARTESIAN_POINT ( 'NONE',  ( 0.9281906404964570534, 34.59732502943162302, 2.863135987906453739 ) ) ;
#18343 = CARTESIAN_POINT ( 'NONE',  ( -48.99983924689409065, 17.84334367881407957, 5.121602422844266478 ) ) ;
#18344 = CARTESIAN_POINT ( 'NONE',  ( -1.959332070151295291, -8.942847522256865744, 4.198131957625402144 ) ) ;
#18345 = CARTESIAN_POINT ( 'NONE',  ( 10.87485472805859210, 124.6990478933366404, 1.296628760762302823 ) ) ;
#18346 = CARTESIAN_POINT ( 'NONE',  ( -2.746491374733735835, 29.57032072151200097, 1.693051300424941230 ) ) ;
#18347 = CARTESIAN_POINT ( 'NONE',  ( -0.8777885371163713923, 105.9485402691003060, 5.279836415571006469 ) ) ;
#18348 = EDGE_CURVE ( 'NONE', #31017, #32583, #15627, .T. ) ;
#18349 = CARTESIAN_POINT ( 'NONE',  ( 3.728136974946417492, 6.765255174955887796, 2.739693761753763113 ) ) ;
#18350 = CARTESIAN_POINT ( 'NONE',  ( 15.78437780952694069, 146.2378312303354448, 0.3154094333657936899 ) ) ;
#18351 = CARTESIAN_POINT ( 'NONE',  ( -5.378050908718009282, 0.3500678860072145016, 6.480130142454380682 ) ) ;
#18352 = CARTESIAN_POINT ( 'NONE',  ( -57.56998337575458891, 1.440017903778734176, -1.358936928125946242 ) ) ;
#18353 = CARTESIAN_POINT ( 'NONE',  ( -8.764338194681526417, 117.8116005833410043, -0.5569156411200119061 ) ) ;
#18354 = CARTESIAN_POINT ( 'NONE',  ( -1.009032787326002323, 123.9312678891798640, -0.1103529103309998094 ) ) ;
#18355 = CYLINDRICAL_SURFACE ( 'NONE', #2215, 12.69999999999999751 ) ;
#18356 = DIRECTION ( 'NONE',  ( -0.8745520943968229099, 0.4849315768086570055, -5.361993529360569999E-16 ) ) ;
#18357 = CARTESIAN_POINT ( 'NONE',  ( -0.5673920217975719771, -4.456920702667952483, 8.403146712094516246 ) ) ;
#18358 = CARTESIAN_POINT ( 'NONE',  ( 2.549837469103328313, 117.9394487944890955, 1.339571799219352100 ) ) ;
#18359 = DIRECTION ( 'NONE',  ( 1.011795553208986377E-16, 1.000000000000000000, -0.000000000000000000 ) ) ;
#18360 = FACE_OUTER_BOUND ( 'NONE', #39293, .T. ) ;
#18361 = CARTESIAN_POINT ( 'NONE',  ( 0.3886773557327865558, 118.1497763966932695, -1.061209395727771509 ) ) ;
#18362 = CARTESIAN_POINT ( 'NONE',  ( -8.185302851676581781, 117.6493956690293317, 0.2478838862282038424 ) ) ;
#18363 = ORIENTED_EDGE ( 'NONE', *, *, #22449, .T. ) ;
#18364 = CARTESIAN_POINT ( 'NONE',  ( -58.55612285180489351, 0.6590214021355567109, -1.070617094346549358E-14 ) ) ;
#18365 = ORIENTED_EDGE ( 'NONE', *, *, #18254, .F. ) ;
#18366 = CARTESIAN_POINT ( 'NONE',  ( -42.61647787783741137, 21.91010357080785198, -1.992259954791246956 ) ) ;
#18367 = CARTESIAN_POINT ( 'NONE',  ( -4.599243292695419427, 121.2024757821991159, -0.09190382657876439154 ) ) ;
#18368 = CARTESIAN_POINT ( 'NONE',  ( 4.192023472006414231, -15.34368243816432198, 4.862536176465709126 ) ) ;
#18369 = CARTESIAN_POINT ( 'NONE',  ( -6.947343058555404127, 158.0090104422344268, 1.506406725519188194 ) ) ;
#18370 = CARTESIAN_POINT ( 'NONE',  ( 2.024878990865616846, 117.2046888992736200, -0.4535333368958820444 ) ) ;
#18371 = CARTESIAN_POINT ( 'NONE',  ( -1.932895124392534303, 20.38400505531995321, -4.219463811995566083 ) ) ;
#18372 = CARTESIAN_POINT ( 'NONE',  ( -23.26560126724731958, 148.8247458934765461, -0.9199859812867272613 ) ) ;
#18373 = CARTESIAN_POINT ( 'NONE',  ( -48.70299960009106854, 18.26799440206204039, -5.162729530914248244 ) ) ;
#18374 = ORIENTED_EDGE ( 'NONE', *, *, #16231, .T. ) ;
#18375 = CARTESIAN_POINT ( 'NONE',  ( 2.183058710814191450, 116.1883852919004596, 0.05356175840457068349 ) ) ;
#18376 = DIRECTION ( 'NONE',  ( -0.8745520943968240202, 0.4849315768086551737, -5.361993529360572958E-16 ) ) ;
#18377 = CARTESIAN_POINT ( 'NONE',  ( -0.009513407573735708014, 119.7614543879625586, 0.4760898169610159325 ) ) ;
#18378 = CARTESIAN_POINT ( 'NONE',  ( -50.98289254807885129, 14.49328483455382788, -4.546320080528299279 ) ) ;
#18379 = CARTESIAN_POINT ( 'NONE',  ( 16.91343413265443729, 151.2926467857828072, -1.744909534579184074 ) ) ;
#18380 = AXIS2_PLACEMENT_3D ( 'NONE', #2351, #15096, #31503 ) ;
#18381 = CARTESIAN_POINT ( 'NONE',  ( -11.86420439699956120, 156.4809912657682673, -1.954521554489340618 ) ) ;
#18382 = CARTESIAN_POINT ( 'NONE',  ( -54.77668461537430034, 8.146287316968315650, -3.518595155146543529 ) ) ;
#18383 = CARTESIAN_POINT ( 'NONE',  ( 4.473055752542707708, 120.8671296916768227, -0.3242568198034685989 ) ) ;
#18384 = ORIENTED_EDGE ( 'NONE', *, *, #7838, .T. ) ;
#18385 = CARTESIAN_POINT ( 'NONE',  ( -12.00230265366671389, 124.3217332413628640, -1.707838685025481196 ) ) ;
#18386 = CARTESIAN_POINT ( 'NONE',  ( 2.493951430369484523, -15.64112390455543711, 5.038688225235472551 ) ) ;
#18387 = CARTESIAN_POINT ( 'NONE',  ( -46.60530155212503445, 26.17382724835477958, -1.270000000000008233 ) ) ;
#18388 = AXIS2_PLACEMENT_3D ( 'NONE', #36972, #11177, #20755 ) ;
#18389 = CARTESIAN_POINT ( 'NONE',  ( -58.30521585032268206, -0.1116666926106041347, -0.6575736669891941721 ) ) ;
#18390 = CARTESIAN_POINT ( 'NONE',  ( -4.848785805035457308, 117.5456108509605002, 0.9615705178007863951 ) ) ;
#18391 = CARTESIAN_POINT ( 'NONE',  ( 17.72773402338096460, 148.0643276405518804, 2.286219595833943963 ) ) ;
#18392 = CYLINDRICAL_SURFACE ( 'NONE', #16467, 0.2540000000000006142 ) ;
#18393 = ADVANCED_FACE ( 'NONE', ( #21068 ), #27480, .F. ) ;
#18394 = AXIS2_PLACEMENT_3D ( 'NONE', #1279, #37053, #7245 ) ;
#18395 = EDGE_CURVE ( 'NONE', #37991, #26452, #38174, .T. ) ;
#18396 = CARTESIAN_POINT ( 'NONE',  ( -7.580879709009198386, 3.543476842659112780, 3.722543307504006194 ) ) ;
#18397 = CARTESIAN_POINT ( 'NONE',  ( -0.001786757842290606548, 120.9379535345006076, 0.08941666878750630099 ) ) ;
#18398 = CARTESIAN_POINT ( 'NONE',  ( -8.270297712355500153, 69.35377921309405735, 1.270000000000002460 ) ) ;
#18400 = EDGE_LOOP ( 'NONE', ( #20343, #40839, #15344, #35212 ) ) ;
#18399 = CARTESIAN_POINT ( 'NONE',  ( -42.93826774478920072, 21.39662913260299959, -1.244340269653810394 ) ) ;
#18401 = CARTESIAN_POINT ( 'NONE',  ( -1.102837227558988831, 118.1588900165301652, 0.8471146098009928460 ) ) ;
#18402 = AXIS2_PLACEMENT_3D ( 'NONE', #3027, #13644, #39643 ) ;
#18403 = CARTESIAN_POINT ( 'NONE',  ( -58.87911280034276018, -0.2081424763510641984, -1.061797465414398100E-14 ) ) ;
#18404 = DIRECTION ( 'NONE',  ( -0.8745520943968243532, 0.4849315768086547296, -5.361993529360573944E-16 ) ) ;
#18405 = DIRECTION ( 'NONE',  ( -5.188838149069471174E-16, 1.699382548006136313E-16, 1.000000000000000000 ) ) ;
#18406 = CARTESIAN_POINT ( 'NONE',  ( -48.20156657701304681, 19.76063879377972654, 5.201425424509390716 ) ) ;
#18407 = CARTESIAN_POINT ( 'NONE',  ( -15.44479738614508868, 120.7004057517279989, -0.1507993925391200030 ) ) ;
#18408 = ORIENTED_EDGE ( 'NONE', *, *, #13078, .T. ) ;
#18409 = CARTESIAN_POINT ( 'NONE',  ( -48.69154271504742582, 20.42972839736894386, -3.938715850604340041 ) ) ;
#18410 = CARTESIAN_POINT ( 'NONE',  ( -7.836266847366137434, 122.3234956677103185, -0.6997315686990351891 ) ) ;
#18411 = CARTESIAN_POINT ( 'NONE',  ( -8.343164213270990004, 120.0286413096533664, 1.117317573728694002 ) ) ;
#18412 = ORIENTED_EDGE ( 'NONE', *, *, #6562, .T. ) ;
#18413 = CARTESIAN_POINT ( 'NONE',  ( 1.447157367358747004, 115.6909491485452719, -1.681836580404131087 ) ) ;
#18414 = CARTESIAN_POINT ( 'NONE',  ( -7.049298115861525105, 122.0434499869739540, -0.3314598731120508290 ) ) ;
#18415 = CARTESIAN_POINT ( 'NONE',  ( 5.179289707447474633, -13.00434337860746581, 2.646125397160491222 ) ) ;
#18416 = CARTESIAN_POINT ( 'NONE',  ( -22.03832501185546633, 149.1257232373000647, 1.146528549967842370 ) ) ;
#18417 = DIRECTION ( 'NONE',  ( -9.627370216492862708E-17, -1.000000000000000000, 0.000000000000000000 ) ) ;
#18418 = CARTESIAN_POINT ( 'NONE',  ( 18.71175911766644617, 125.2636347375217838, 0.5504587009833171729 ) ) ;
#18419 = CARTESIAN_POINT ( 'NONE',  ( 15.76967257419122781, 146.5682726256061130, 0.3822029702838447007 ) ) ;
#18420 = DIRECTION ( 'NONE',  ( -0.8745520943968253524, 0.4849315768086530087, -4.268512490100385764E-16 ) ) ;
#18421 = CARTESIAN_POINT ( 'NONE',  ( 0.3093957028193324299, 29.65535775802675289, -0.9258560203679269129 ) ) ;
#18422 = CARTESIAN_POINT ( 'NONE',  ( -21.90252518039365981, 151.4352167165723415, -0.5139180553509251625 ) ) ;
#18423 = CARTESIAN_POINT ( 'NONE',  ( -41.26650596300371632, 23.23696532716443741, -1.524000000000029775 ) ) ;
#18424 = CARTESIAN_POINT ( 'NONE',  ( -7.383526124176625238, 117.2783386306103921, -0.1475404267317128315 ) ) ;
#18425 = ORIENTED_EDGE ( 'NONE', *, *, #21856, .T. ) ;
#18426 = CARTESIAN_POINT ( 'NONE',  ( 2.893028018094861320, 117.2553914413831535, 0.7100786824799962815 ) ) ;
#18427 = DIRECTION ( 'NONE',  ( -0.4849315768086480127, -0.8745520943968279060, -1.030032898892941415E-16 ) ) ;
#18428 = CARTESIAN_POINT ( 'NONE',  ( 9.289280848106727717, 118.8811571165754941, 1.201727579052786599 ) ) ;
#18429 = CARTESIAN_POINT ( 'NONE',  ( 2.710741864450562755, 158.4754809254847601, -1.535472453293832418 ) ) ;
#18430 = CARTESIAN_POINT ( 'NONE',  ( 7.231359443275770182, 22.16797014818540745, 4.386519482779798196 ) ) ;
#18431 = CARTESIAN_POINT ( 'NONE',  ( -14.73734951358261824, 121.3346631531286164, -1.319546682830233797 ) ) ;
#18432 = CARTESIAN_POINT ( 'NONE',  ( 4.746482201166442927, 117.7550804213460651, -0.8965027487333476763 ) ) ;
#18433 = CIRCLE ( 'NONE', #5540, 0.3810000000000015041 ) ;
#18434 = CARTESIAN_POINT ( 'NONE',  ( 5.469471049222477177, 117.5088849381099436, 0.8278104034524698118 ) ) ;
#18435 = ORIENTED_EDGE ( 'NONE', *, *, #33633, .F. ) ;
#18436 = CARTESIAN_POINT ( 'NONE',  ( -15.23158847265895410, 143.4365109762209158, -0.1756275167766374046 ) ) ;
#18437 = CARTESIAN_POINT ( 'NONE',  ( -6.637665810843349057, 119.8184877057495754, -1.268479684707346289 ) ) ;
#18438 = CARTESIAN_POINT ( 'NONE',  ( 3.006733222167471631, -15.59844357659602387, 5.538909454127313836 ) ) ;
#18439 = CIRCLE ( 'NONE', #22525, 0.5080000000000000071 ) ;
#18440 = CARTESIAN_POINT ( 'NONE',  ( 4.787476607852438448, 115.6909491485453145, 1.476299238943078906 ) ) ;
#18441 = CARTESIAN_POINT ( 'NONE',  ( -0.9880787409092588458, 117.9496054967312375, -1.392611192464434211 ) ) ;
#18442 = ORIENTED_EDGE ( 'NONE', *, *, #19832, .T. ) ;
#18443 = CARTESIAN_POINT ( 'NONE',  ( 1.300143943178173833, 119.1766673560425858, 0.6697961403939317604 ) ) ;
#18444 = CARTESIAN_POINT ( 'NONE',  ( -6.591743005429100447E-14, 88.48546620154573361, -4.217761848057333172E-18 ) ) ;
#18445 = TOROIDAL_SURFACE ( 'NONE', #23898, 0.3809999999999997278, 0.2540000000000000036 ) ;
#18446 = CYLINDRICAL_SURFACE ( 'NONE', #17103, 14.73199999999999577 ) ;
#18447 = CARTESIAN_POINT ( 'NONE',  ( -2.162440637018797407, 123.3349985135950959, 0.07568789353404307974 ) ) ;
#18448 = CARTESIAN_POINT ( 'NONE',  ( -8.215080244096204964, -10.21703095211954704, 2.011605797521776928 ) ) ;
#18449 = CARTESIAN_POINT ( 'NONE',  ( 3.075464349291132216, 156.1450793681712241, 0.7387695966741768538 ) ) ;
#18450 = DIRECTION ( 'NONE',  ( -0.9891443546370349837, 0.000000000000000000, -0.1469470846586743984 ) ) ;
#18451 = ADVANCED_FACE ( 'NONE', ( #7688, #24473 ), #10655, .F. ) ;
#18452 = CARTESIAN_POINT ( 'NONE',  ( 7.877688851764411915, 158.6543443936584481, -0.4710593659051897641 ) ) ;
#18453 = CARTESIAN_POINT ( 'NONE',  ( 4.918180946948674581, 56.51499999999999346, -4.748993904426717982 ) ) ;
#18454 = CARTESIAN_POINT ( 'NONE',  ( -57.97322207812975137, 0.5626473900411875784, 0.8941911358200723692 ) ) ;
#18455 = CARTESIAN_POINT ( 'NONE',  ( -5.562421465964138001, 116.6996505075888422, -0.1685898161880411972 ) ) ;
#18456 = VECTOR ( 'NONE', #31246, 1000.000000000000000 ) ;
#18457 = DIRECTION ( 'NONE',  ( 0.9807655518882848478, -0.1951894777626808908, 8.537024980200819846E-16 ) ) ;
#18458 = CARTESIAN_POINT ( 'NONE',  ( -4.168157594931272136, 118.2394498548492265, 0.2219570363417781578 ) ) ;
#18459 = CARTESIAN_POINT ( 'NONE',  ( 3.174366308151880922, 104.6144662015457243, 0.06343139340882769650 ) ) ;
#18460 = EDGE_LOOP ( 'NONE', ( #36724, #3306, #41476, #24106 ) ) ;
#18461 = CARTESIAN_POINT ( 'NONE',  ( -48.98489377192316852, 18.65252824715059177, 5.272350768541908650 ) ) ;
#18462 = CARTESIAN_POINT ( 'NONE',  ( 4.359163536690966900, 119.4473459596788842, -0.7549756355859075230 ) ) ;
#18463 = TOROIDAL_SURFACE ( 'NONE', #4130, 0.7620000000000000107, 0.2540000000000000036 ) ;
#18464 = CARTESIAN_POINT ( 'NONE',  ( -16.04872481256650829, 146.6973543426590254, -1.173426683271128868 ) ) ;
#18465 = CARTESIAN_POINT ( 'NONE',  ( 4.959033476919109340, 117.6447102886128988, -0.6722175906395938538 ) ) ;
#18466 = CARTESIAN_POINT ( 'NONE',  ( 0.1336191844408766705, 117.3993836134489044, -1.490790351259109414 ) ) ;
#18467 = ORIENTED_EDGE ( 'NONE', *, *, #10267, .T. ) ;
#18468 = CARTESIAN_POINT ( 'NONE',  ( -4.598301960400187127, 22.30806413504685537, 0.5496829067130363233 ) ) ;
#18469 = CARTESIAN_POINT ( 'NONE',  ( -28.99017888285159117, 62.64366196047017610, 1.523999999999993804 ) ) ;
#18470 = DIRECTION ( 'NONE',  ( -0.8745520943968243532, 0.4849315768086547296, -5.361993529360573944E-16 ) ) ;
#18471 = DIRECTION ( 'NONE',  ( -5.206863593109713661E-17, 1.000000000000000000, -1.077750396879097183E-30 ) ) ;
#18472 = CARTESIAN_POINT ( 'NONE',  ( -12.21488373879589062, 56.36092316367925292, -5.016499999999999737 ) ) ;
#18473 = CARTESIAN_POINT ( 'NONE',  ( 6.071400464523738272, 121.4469273266857670, 0.1932373124915481855 ) ) ;
#18474 = CARTESIAN_POINT ( 'NONE',  ( 5.332935397695205637, 105.1224662015457199, 0.1065647409268305201 ) ) ;
#18475 = CARTESIAN_POINT ( 'NONE',  ( 2.899385524442493534, 117.0242007548465608, 0.5112881796358940134 ) ) ;
#18476 = CARTESIAN_POINT ( 'NONE',  ( 4.808131379915037584, 104.6144662015457527, -0.4149153341867691802 ) ) ;
#18478 = CARTESIAN_POINT ( 'NONE',  ( 21.26977539036077403, 145.8710773725474610, -1.472442194194814702 ) ) ;
#18477 = CARTESIAN_POINT ( 'NONE',  ( 1.850858793973401584, -15.28950465061244834, 5.390636727418374186 ) ) ;
#18479 = CARTESIAN_POINT ( 'NONE',  ( -4.278356142284035712, 119.7015364213435333, 0.7555980432150397608 ) ) ;
#18480 = CARTESIAN_POINT ( 'NONE',  ( 1.072590735131739414, 20.86836736082219801, 4.503669761903479341 ) ) ;
#18481 = CARTESIAN_POINT ( 'NONE',  ( -10.49915001570439266, 157.9057380314836223, -0.9855651801815565882 ) ) ;
#18482 = CARTESIAN_POINT ( 'NONE',  ( -0.7773729966126706747, -2.891840825076433585, -0.5888577047253038543 ) ) ;
#18483 = ORIENTED_EDGE ( 'NONE', *, *, #12274, .F. ) ;
#18484 = CARTESIAN_POINT ( 'NONE',  ( -56.40799993875704388, 3.472264316502340797, 0.7602746155037158893 ) ) ;
#18485 = CARTESIAN_POINT ( 'NONE',  ( -9.542306315654425219, 124.2661852542617709, 0.2373755145837090630 ) ) ;
#18486 = CARTESIAN_POINT ( 'NONE',  ( 2.287996554222524903, -15.35138490607948469, 5.941601703801219436 ) ) ;
#18487 = CARTESIAN_POINT ( 'NONE',  ( 16.63213601294257415, 144.0643239018434940, -1.266953209168786953 ) ) ;
#18488 = VERTEX_POINT ( 'NONE', #17875 ) ;
#18489 = CARTESIAN_POINT ( 'NONE',  ( 3.014676604589255238, 115.7029491485453292, 1.668003145632996231 ) ) ;
#18490 = AXIS2_PLACEMENT_3D ( 'NONE', #13458, #39448, #6440 ) ;
#18491 = CARTESIAN_POINT ( 'NONE',  ( -4.858315324244927069, 117.7455535390209604, -0.9239789875634819571 ) ) ;
#18492 = EDGE_CURVE ( 'NONE', #22451, #13790, #8770, .T. ) ;
#18493 = CARTESIAN_POINT ( 'NONE',  ( 8.935197197525127422, 123.9063447689825779, 0.1785465045940571871 ) ) ;
#18494 = ORIENTED_EDGE ( 'NONE', *, *, #11859, .F. ) ;
#18495 = CARTESIAN_POINT ( 'NONE',  ( 7.650403556475533939, 119.6133147451300971, 1.381840873585064688 ) ) ;
#18496 = CARTESIAN_POINT ( 'NONE',  ( -6.503981220335420706E-14, 66.64146620154573952, -9.408573323119121831E-18 ) ) ;
#18497 = CARTESIAN_POINT ( 'NONE',  ( 3.682264917456193665, 69.43546620154573645, 0.07358041635423968885 ) ) ;
#18498 = EDGE_CURVE ( 'NONE', #20056, #36001, #23857, .T. ) ;
#18499 = CARTESIAN_POINT ( 'NONE',  ( 0.002459401150240396027, 159.6023738651833810, -0.1230784904792617679 ) ) ;
#18500 = CARTESIAN_POINT ( 'NONE',  ( 20.66439279448287181, 152.5811724025633112, 0.09276230403812320280 ) ) ;
#18501 = CARTESIAN_POINT ( 'NONE',  ( -20.21600168833980149, 80.16988503754176065, 1.523999999999995580 ) ) ;
#18502 = CARTESIAN_POINT ( 'NONE',  ( 4.854022926505809465, 118.7629491485453030, -0.1809382747281913784 ) ) ;
#18503 = CARTESIAN_POINT ( 'NONE',  ( 1.803749805595953326, -15.30621593874753650, 5.393099756912645759 ) ) ;
#18504 = DIRECTION ( 'NONE',  ( -5.206863593109713661E-17, 1.000000000000000000, -1.077750396879097183E-30 ) ) ;
#18505 = CARTESIAN_POINT ( 'NONE',  ( -3.590474171207809651E-14, 56.51499999999999346, 0.000000000000000000 ) ) ;
#18506 = EDGE_CURVE ( 'NONE', #27187, #31705, #40221, .T. ) ;
#18507 = CARTESIAN_POINT ( 'NONE',  ( -4.767607816231247853, 117.8956932628570513, 0.7411698513071134364 ) ) ;
#18508 = ORIENTED_EDGE ( 'NONE', *, *, #35252, .F. ) ;
#18509 = VERTEX_POINT ( 'NONE', #27269 ) ;
#18510 = DIRECTION ( 'NONE',  ( -0.000000000000000000, -0.000000000000000000, -1.000000000000000000 ) ) ;
#18511 = CARTESIAN_POINT ( 'NONE',  ( -8.406060086832516376, 119.4770703846445059, -1.395343900433620110 ) ) ;
#18512 = CARTESIAN_POINT ( 'NONE',  ( -4.819599041176440224, 120.7138498849978987, -0.4051376471031730153 ) ) ;
#18513 = CARTESIAN_POINT ( 'NONE',  ( 4.911660101568102732, 117.6260080863869320, 0.9594402546315066171 ) ) ;
#18514 = CARTESIAN_POINT ( 'NONE',  ( -11.42297701379740893, 55.88459609804021255, -4.463034230327257212 ) ) ;
#18515 = CARTESIAN_POINT ( 'NONE',  ( -1.058122102717379942, 124.9344662015457459, -0.02114379780294212835 ) ) ;
#18516 = VECTOR ( 'NONE', #19155, 1000.000000000000114 ) ;
#18517 = FILL_AREA_STYLE ('',( #41124 ) ) ;
#18518 = CARTESIAN_POINT ( 'NONE',  ( -57.93941708942283952, 2.052042089854988483, 1.628789306319508023 ) ) ;
#18519 = DIRECTION ( 'NONE',  ( 5.188838149069472160E-16, -1.699382548006136559E-16, -1.000000000000000000 ) ) ;
#18520 = CARTESIAN_POINT ( 'NONE',  ( 3.391857759029038633, -13.93828481737184610, 3.530066096054821134 ) ) ;
#18521 = CARTESIAN_POINT ( 'NONE',  ( 3.253275476659236443, 108.9521120498200730, -3.903703133364782030 ) ) ;
#18522 = CARTESIAN_POINT ( 'NONE',  ( -7.266810130343835716, 121.1388872696715282, -1.097806971394259312 ) ) ;
#18523 = CARTESIAN_POINT ( 'NONE',  ( -7.785295067471754926, 122.6196652447830502, -0.2112362379013654756 ) ) ;
#18524 = DIRECTION ( 'NONE',  ( -0.8745520943968246863, 0.4849315768086538414, -5.122214988120500191E-16 ) ) ;
#18525 = EDGE_CURVE ( 'NONE', #11900, #23570, #33383, .T. ) ;
#18526 = CARTESIAN_POINT ( 'NONE',  ( -0.2141370455737806877, 115.7030700810080930, 1.756908310108165505 ) ) ;
#18527 = CARTESIAN_POINT ( 'NONE',  ( 4.419457123578296454, 17.78516144714274105, -1.360477052881604143 ) ) ;
#18529 = VERTEX_POINT ( 'NONE', #883 ) ;
#18528 = CARTESIAN_POINT ( 'NONE',  ( 18.48423909989026725, 154.1703991122031994, 0.9245180971295520189 ) ) ;
#18530 = CARTESIAN_POINT ( 'NONE',  ( 2.860261174899399350, 104.6144662015456959, -3.897939397042970544 ) ) ;
#18531 = CARTESIAN_POINT ( 'NONE',  ( 4.104683988343100332, -15.63859574289259946, 3.129333468668611840 ) ) ;
#18532 = CARTESIAN_POINT ( 'NONE',  ( -12.06323264149831154, 122.4500365997666336, 1.303827596403756672 ) ) ;
#18533 = CARTESIAN_POINT ( 'NONE',  ( 0.9751022921854990422, 22.16746322748675624, -0.05045228706074462999 ) ) ;
#18534 = CARTESIAN_POINT ( 'NONE',  ( 0.9280917288853990366, 18.63875360461660335, -0.3060232888646727822 ) ) ;
#18535 = EDGE_CURVE ( 'NONE', #1100, #18074, #35136, .T. ) ;
#18536 = ORIENTED_EDGE ( 'NONE', *, *, #7471, .F. ) ;
#18537 = AXIS2_PLACEMENT_3D ( 'NONE', #8409, #27993, #24796 ) ;
#18538 = VERTEX_POINT ( 'NONE', #7895 ) ;
#18539 = CARTESIAN_POINT ( 'NONE',  ( -41.05189575270516400, 23.09451173561988213, 0.9172222222222163879 ) ) ;
#18540 = CARTESIAN_POINT ( 'NONE',  ( 3.998531074477424507, 117.0582680968029905, 1.101271957883943164 ) ) ;
#18541 = CARTESIAN_POINT ( 'NONE',  ( -16.05848832435436435, 147.7157881801689427, 0.7882342824236393541 ) ) ;
#18542 = DIRECTION ( 'NONE',  ( 0.9998501190848636533, 0.01731298258487451447, 5.158639060800524920E-16 ) ) ;
#18543 = CARTESIAN_POINT ( 'NONE',  ( 3.377503200524144322, -12.59127376242380514, 1.184662976626496000 ) ) ;
#18544 = CARTESIAN_POINT ( 'NONE',  ( 0.5414988153859304765, 119.6443647996702566, -0.5124704023889977700 ) ) ;
#18545 = CARTESIAN_POINT ( 'NONE',  ( -19.94553544501724573, 148.6304843473828043, -2.499072228797274864 ) ) ;
#18546 = LINE ( 'NONE', #14721, #34496 ) ;
#18547 = EDGE_CURVE ( 'NONE', #1374, #25364, #17667, .T. ) ;
#18548 = CARTESIAN_POINT ( 'NONE',  ( -3.682264917456324227, 88.48546620154573361, -0.07358041635423923088 ) ) ;
#18549 = CARTESIAN_POINT ( 'NONE',  ( -3.991072007095600949, 33.40439263831326855, 3.842775004540742501 ) ) ;
#18550 = CARTESIAN_POINT ( 'NONE',  ( 15.40459090795122776, 148.0444422243178337, -0.2810841713230231020 ) ) ;
#18551 = ORIENTED_EDGE ( 'NONE', *, *, #7890, .F. ) ;
#18552 = CARTESIAN_POINT ( 'NONE',  ( 2.567065079198288746, -15.08448375773686934, 4.691402903081304920 ) ) ;
#18553 = DIRECTION ( 'NONE',  ( -0.1469470846586743706, -9.335746474409589170E-17, 0.9891443546370348727 ) ) ;
#18554 = DIRECTION ( 'NONE',  ( 1.000000000000000000, -9.627370216492862708E-17, 0.000000000000000000 ) ) ;
#18555 = CIRCLE ( 'NONE', #34239, 0.6350000000000027844 ) ;
#18556 = CARTESIAN_POINT ( 'NONE',  ( -58.43299954449013001, -0.3955325680177061431, 0.3375922266957475104 ) ) ;
#18557 = CARTESIAN_POINT ( 'NONE',  ( -4.626086514281606554, -10.66701884381306087, 0.02375484599842511355 ) ) ;
#18558 = CARTESIAN_POINT ( 'NONE',  ( 16.27782172975856412, 148.1602266505728380, 1.760797687140677414 ) ) ;
#18559 = FACE_OUTER_BOUND ( 'NONE', #41194, .T. ) ;
#18560 = CARTESIAN_POINT ( 'NONE',  ( 3.715898061424960375, 116.6275173757784813, 0.03328880940299697860 ) ) ;
#18561 = CARTESIAN_POINT ( 'NONE',  ( -7.669269000495163802, 124.9344662015457317, -0.1532502464757266036 ) ) ;
#18562 = AXIS2_PLACEMENT_3D ( 'NONE', #40235, #37031, #24011 ) ;
#18563 = CARTESIAN_POINT ( 'NONE',  ( -3.158589313471108273, 4.191505055319898254, 3.400481138232230194 ) ) ;
#18564 = CARTESIAN_POINT ( 'NONE',  ( 4.223292309264916611, 155.8535809751167562, 0.1210084730045380141 ) ) ;
#18565 = EDGE_CURVE ( 'NONE', #1374, #30952, #23166, .T. ) ;
#18566 = CARTESIAN_POINT ( 'NONE',  ( -1.603550922812138735, -3.093932695209369754, -8.287855504117967342 ) ) ;
#18567 = CARTESIAN_POINT ( 'NONE',  ( -57.72731561024293967, 0.8685078910841970146, -1.009486960136972124E-14 ) ) ;
#18568 = CARTESIAN_POINT ( 'NONE',  ( 2.165612022977871920, 116.6455396352414624, -0.3652780253405325528 ) ) ;
#18569 = CARTESIAN_POINT ( 'NONE',  ( -0.3459730346048953131, 118.1497763966932695, -1.075889458897477668 ) ) ;
#18570 = CARTESIAN_POINT ( 'NONE',  ( 11.58677707360137710, 55.24500000000000455, 4.474811398758258285 ) ) ;
#18571 = CARTESIAN_POINT ( 'NONE',  ( -3.991072007095600949, 33.40439263831326855, 3.842775004540742501 ) ) ;
#18572 = CARTESIAN_POINT ( 'NONE',  ( -4.559029627765868398, 31.49133049583988253, -0.6947656260628575220 ) ) ;
#18573 = CARTESIAN_POINT ( 'NONE',  ( 0.7773589538612868388, 118.1588881499372832, 0.8997936918793348893 ) ) ;
#18574 = CYLINDRICAL_SURFACE ( 'NONE', #7632, 0.2539999999999998925 ) ;
#18575 = DIRECTION ( 'NONE',  ( -0.000000000000000000, -0.000000000000000000, -1.000000000000000000 ) ) ;
#18576 = CARTESIAN_POINT ( 'NONE',  ( 0.2562694446381907354, 108.5751225745497806, -4.260274975122999130 ) ) ;
#18577 = CARTESIAN_POINT ( 'NONE',  ( -23.01821387067777991, 149.5377445326608665, 0.2676165590851173892 ) ) ;
#18578 = EDGE_CURVE ( 'NONE', #17268, #38830, #36142, .T. ) ;
#18579 = ORIENTED_EDGE ( 'NONE', *, *, #31551, .F. ) ;
#18580 = CARTESIAN_POINT ( 'NONE',  ( -58.16194989728258946, 1.772972946764553193, -1.069098630790430628E-14 ) ) ;
#18581 = ORIENTED_EDGE ( 'NONE', *, *, #16439, .T. ) ;
#18582 = CARTESIAN_POINT ( 'NONE',  ( -42.47169588413672159, 21.98427696618753302, -1.915014136677441581 ) ) ;
#18583 = AXIS2_PLACEMENT_3D ( 'NONE', #34162, #33745, #7756 ) ;
#18584 = CARTESIAN_POINT ( 'NONE',  ( -15.53033519385735417, 147.5364864818501189, -0.1767648362992366440 ) ) ;
#18585 = CARTESIAN_POINT ( 'NONE',  ( 3.223661160190148145, -15.48894043311785396, 5.519697737696615647 ) ) ;
#18586 = CARTESIAN_POINT ( 'NONE',  ( -18.13891979603535631, 131.7244750738095149, 1.506900917850658050 ) ) ;
#18587 = CARTESIAN_POINT ( 'NONE',  ( 3.950580610160879580, 117.4679918459733585, -0.5815556119072163854 ) ) ;
#18588 = CARTESIAN_POINT ( 'NONE',  ( -3.234384296441582762, 11.31316835407710819, -3.315160845070126427 ) ) ;
#18589 = CARTESIAN_POINT ( 'NONE',  ( -15.81407516854451245, 121.2341309109925334, -0.7422539548746109883 ) ) ;
#18590 = CARTESIAN_POINT ( 'NONE',  ( -58.23230438342547188, 0.5587453749347339738, -1.096084957074963340 ) ) ;
#18591 = CIRCLE ( 'NONE', #32901, 5.080000000000006288 ) ;
#18592 = ORIENTED_EDGE ( 'NONE', *, *, #37489, .F. ) ;
#18593 = CARTESIAN_POINT ( 'NONE',  ( 2.182332163943836001, 116.1897970688731760, 0.04360819029793291252 ) ) ;
#18594 = CARTESIAN_POINT ( 'NONE',  ( -0.02615319344480911481, 156.8698190429800832, 1.308812744920978322 ) ) ;
#18595 = CARTESIAN_POINT ( 'NONE',  ( -57.21666742898756297, 2.192505647111198552, -1.643075081891994138 ) ) ;
#18596 = EDGE_CURVE ( 'NONE', #6334, #22648, #22105, .T. ) ;
#18597 = CARTESIAN_POINT ( 'NONE',  ( 10.65007529713506962, 155.7851685111067184, -1.746298732392691289 ) ) ;
#18598 = CARTESIAN_POINT ( 'NONE',  ( -13.40516742707921516, 121.5866728338796463, -1.646856811522066089 ) ) ;
#18599 = CARTESIAN_POINT ( 'NONE',  ( -56.80697847991661575, 4.636179106009441497, -2.484889565616585472 ) ) ;
#18600 = AXIS2_PLACEMENT_3D ( 'NONE', #11391, #24377, #21798 ) ;
#18601 = ADVANCED_FACE ( 'NONE', ( #12336 ), #29313, .T. ) ;
#18602 = CARTESIAN_POINT ( 'NONE',  ( 12.88338908221804324, 130.8243885708800747, -0.7627239795610333273 ) ) ;
#18603 = ORIENTED_EDGE ( 'NONE', *, *, #10800, .T. ) ;
#18604 = CARTESIAN_POINT ( 'NONE',  ( -9.190671247346116957, 121.6705353891887995, -1.423780222299954046 ) ) ;
#18605 = CARTESIAN_POINT ( 'NONE',  ( 4.210067206397440032, -15.44688347603401191, 1.362376457177303157 ) ) ;
#18606 = CARTESIAN_POINT ( 'NONE',  ( -4.108446860257354061, 118.2429491485453070, -0.3498540877621626466 ) ) ;
#18607 = CARTESIAN_POINT ( 'NONE',  ( -58.37241122568488549, -0.2962816677227753104, -0.2416009568454014489 ) ) ;
#18608 = CARTESIAN_POINT ( 'NONE',  ( -4.799585727462988949, 117.4716807894286461, 1.004530280717990331 ) ) ;
#18609 = CARTESIAN_POINT ( 'NONE',  ( 11.20916139128192235, 123.4744472594011739, 1.589032359792267757 ) ) ;
#18610 = FACE_OUTER_BOUND ( 'NONE', #41492, .T. ) ;
#18611 = AXIS2_PLACEMENT_3D ( 'NONE', #40046, #20621, #24244 ) ;
#18612 = CARTESIAN_POINT ( 'NONE',  ( -1.796629210684171918, -4.683219827815034542, 8.244768259809569955 ) ) ;
#18613 = CARTESIAN_POINT ( 'NONE',  ( 7.049298115861396319, 122.0434499869739540, 0.3314598731120510511 ) ) ;
#18614 = DIRECTION ( 'NONE',  ( -0.000000000000000000, 0.000000000000000000, -1.000000000000000000 ) ) ;
#18615 = TOROIDAL_SURFACE ( 'NONE', #24065, 0.8889999999999989022, 0.2540000000000000036 ) ;
#18617 = ORIENTED_EDGE ( 'NONE', *, *, #42077, .F. ) ;
#18616 = CARTESIAN_POINT ( 'NONE',  ( -41.05189575270522795, 23.09451173561975779, -1.171222222222227272 ) ) ;
#18618 = CARTESIAN_POINT ( 'NONE',  ( -0.5515347699655459568, 117.3993826269703362, 1.472900392318948093 ) ) ;
#18619 = CARTESIAN_POINT ( 'NONE',  ( -58.24807683554808335, 1.288543178753334573, 1.357556113208942428 ) ) ;
#18620 = CARTESIAN_POINT ( 'NONE',  ( -7.974902364581113900, 121.6049040996757782, -1.136138042282031968 ) ) ;
#18621 = CIRCLE ( 'NONE', #37678, 0.2540000000000067204 ) ;
#18622 = CARTESIAN_POINT ( 'NONE',  ( -5.177913976931289852, 65.30181249999998272, -5.372100000000007647 ) ) ;
#18623 = CARTESIAN_POINT ( 'NONE',  ( -50.58128808078254934, 18.64259194233895656, 3.042287330737921902 ) ) ;
#18624 = CARTESIAN_POINT ( 'NONE',  ( -22.82234304556254401, 150.4043717142618277, -0.2269822898261399657 ) ) ;
#18625 = EDGE_LOOP ( 'NONE', ( #12891, #3525, #462, #10328 ) ) ;
#18626 = CARTESIAN_POINT ( 'NONE',  ( -50.42190507837991476, 20.37545339363690999, -1.629190407695439324 ) ) ;
#18627 = CARTESIAN_POINT ( 'NONE',  ( 7.852298358788947219, 122.3486847557867208, -0.3610446264703879860 ) ) ;
#18628 = CARTESIAN_POINT ( 'NONE',  ( -8.348968351562039203, 120.0002459142761211, 1.116349756213214972 ) ) ;
#18629 = ORIENTED_EDGE ( 'NONE', *, *, #36018, .F. ) ;
#18630 = CARTESIAN_POINT ( 'NONE',  ( 2.051617846517921340, 115.7029490350661405, -1.635872274556314121 ) ) ;
#18632 = AXIS2_PLACEMENT_3D ( 'NONE', #22148, #35180, #41994 ) ;
#18631 = CARTESIAN_POINT ( 'NONE',  ( -15.22644562805688295, 143.4365109762209158, -0.4329964906482475229 ) ) ;
#18633 = CARTESIAN_POINT ( 'NONE',  ( 2.999908722124702720, -15.10219813539979938, 5.696538855611934515 ) ) ;
#18634 = CARTESIAN_POINT ( 'NONE',  ( -21.56827676951031236, 148.6087350971780836, 1.383610176320235308 ) ) ;
#18635 = CARTESIAN_POINT ( 'NONE',  ( 1.028482355383298241, 117.3993836102110464, -1.440227903949694577 ) ) ;
#18636 = CARTESIAN_POINT ( 'NONE',  ( 20.28976221201013175, 128.9598305440861452, 0.6839793015867966508 ) ) ;
#18637 = CARTESIAN_POINT ( 'NONE',  ( 7.775851458259090521, 154.6677978696501725, 0.2111400444086546369 ) ) ;
#18638 = DIRECTION ( 'NONE',  ( 6.146657985744592735E-16, 3.905054717696927382E-31, 1.000000000000000000 ) ) ;
#18639 = CARTESIAN_POINT ( 'NONE',  ( 0.2459283266301676152, 20.16186220226971315, -0.9436028068393225166 ) ) ;
#18640 = CARTESIAN_POINT ( 'NONE',  ( -22.66113959641441511, 150.6410255081855212, -0.5295512721432396042 ) ) ;
#18641 = CARTESIAN_POINT ( 'NONE',  ( -6.651972016613293606E-14, 104.1064662015457287, 7.011588703784780528E-31 ) ) ;
#18642 = DIRECTION ( 'NONE',  ( -1.000000000000000000, 0.000000000000000000, 0.000000000000000000 ) ) ;
#18643 = ORIENTED_EDGE ( 'NONE', *, *, #914, .F. ) ;
#18644 = CARTESIAN_POINT ( 'NONE',  ( 8.329591456240351022, 119.8454013155109834, 1.442285711102194723 ) ) ;
#18645 = CARTESIAN_POINT ( 'NONE',  ( 7.956670401304478446, 118.4344479264803169, 1.111586840565143675 ) ) ;
#18646 = CARTESIAN_POINT ( 'NONE',  ( 7.786520497867073232, 119.2688035297948659, -1.033142384104571043 ) ) ;
#18647 = AXIS2_PLACEMENT_3D ( 'NONE', #3749, #16706, #25876 ) ;
#18648 = CARTESIAN_POINT ( 'NONE',  ( -5.424866478234207534, 26.46299946464603181, -6.465121161284864471 ) ) ;
#18649 = CARTESIAN_POINT ( 'NONE',  ( -14.30926610799427934, 121.2650221238243944, -1.406141635412307300 ) ) ;
#18650 = CARTESIAN_POINT ( 'NONE',  ( 4.905962780720105165, 117.7163134916238363, -0.7387128614738237564 ) ) ;
#18651 = ADVANCED_FACE ( 'NONE', ( #2132 ), #11914, .T. ) ;
#18652 = CARTESIAN_POINT ( 'NONE',  ( 5.227922695814323006, 116.4790307410953289, 1.091139864702252549 ) ) ;
#18653 = B_SPLINE_CURVE_WITH_KNOTS ( 'NONE', 3,
 ( #34928, #5756, #23146, #7003, #36183, #29575, #19129, #6162, #29355, #3816, #411, #2967, #35967, #10177, #39161, #6365, #19973, #22310 ),
 .UNSPECIFIED., .F., .F.,
 ( 4, 1, 1, 1, 1, 1, 2, 1, 1, 1, 2, 1, 1, 4 ),
 ( 0.000000000000000000, 0.1631003137318064733, 0.3262006274636129466, 0.4077507843295161694, 0.4893009411954193921, 0.5708510980613227259, 0.6524012549272260042, 0.6576100072399926333, 0.6628187595527593734, 0.6680275118655260025, 0.6732362641782927426, 0.7053937736304701778, 0.7375512830826475019, 0.7543499533669120183 ),
 .UNSPECIFIED. ) ;
#18654 = CARTESIAN_POINT ( 'NONE',  ( -5.292481242636031702, 121.3432423864224177, -0.03610140192510977175 ) ) ;
#18655 = CARTESIAN_POINT ( 'NONE',  ( -2.358209769532914724, 119.0637060312156024, -0.7902384042126600061 ) ) ;
#18656 = CARTESIAN_POINT ( 'NONE',  ( 2.643346398695107347, -15.60183157139904964, 5.704389875863137505 ) ) ;
#18657 = DIRECTION ( 'NONE',  ( 0.000000000000000000, 0.000000000000000000, -1.000000000000000000 ) ) ;
#18658 = CARTESIAN_POINT ( 'NONE',  ( -2.723305694757628626, 118.1651002906158539, -0.8146868860962922509 ) ) ;
#18659 = VERTEX_POINT ( 'NONE', #8724 ) ;
#18660 = CARTESIAN_POINT ( 'NONE',  ( 18.80567741551205785, 148.1672603684278329, 2.476295349149460812 ) ) ;
#18661 = FILL_AREA_STYLE ('',( #41264 ) ) ;
#18662 = FACE_OUTER_BOUND ( 'NONE', #37979, .T. ) ;
#18663 = CARTESIAN_POINT ( 'NONE',  ( -2.994815693583476879, 122.7580772961051707, 0.09506955764664398734 ) ) ;
#18664 = CARTESIAN_POINT ( 'NONE',  ( 4.267473507877284078, -4.198009126799147062, -7.300781474974544771 ) ) ;
#18665 = CARTESIAN_POINT ( 'NONE',  ( 8.311356586561950976, 122.7091975629380585, 0.7066836605292580176 ) ) ;
#18666 = CARTESIAN_POINT ( 'NONE',  ( -43.82859865241511699, 24.63416949198730421, -1.524000000000007127 ) ) ;
#18667 = CARTESIAN_POINT ( 'NONE',  ( 22.01496335533477833, 136.8935083344700558, -0.5016514318445886023 ) ) ;
#18668 = CYLINDRICAL_SURFACE ( 'NONE', #25393, 1.270000000000000240 ) ;
#18669 = CARTESIAN_POINT ( 'NONE',  ( -57.98746369505321496, 0.5317391348542490626, 0.8755459602923044704 ) ) ;
#18670 = CARTESIAN_POINT ( 'NONE',  ( 6.073982626571928556, 78.87340550758391089, 4.346604155593825958 ) ) ;
#18671 = DIRECTION ( 'NONE',  ( -0.8138664877804110409, 0.5810519254489896479, 0.000000000000000000 ) ) ;
#18672 = CARTESIAN_POINT ( 'NONE',  ( -0.2924095564369283418, 116.4254662015451913, -0.005843038833676939166 ) ) ;
#18673 = ORIENTED_EDGE ( 'NONE', *, *, #2127, .T. ) ;
#18674 = CARTESIAN_POINT ( 'NONE',  ( -58.70413935429054675, 0.2332485698458008905, 0.6626129746612759996 ) ) ;
#18675 = CARTESIAN_POINT ( 'NONE',  ( -4.830459837891577735, 119.9522586551379817, -0.8951123600124439861 ) ) ;
#18676 = CARTESIAN_POINT ( 'NONE',  ( -5.260208640450895423, 116.0444662015457595, -1.274361246762516942 ) ) ;
#18677 = CARTESIAN_POINT ( 'NONE',  ( -0.6802018490772304693, 156.3636429644085695, -0.5246204485115751881 ) ) ;
#18678 = CARTESIAN_POINT ( 'NONE',  ( 5.035933200060415338, 117.3993844219003648, -0.5513780243448201945 ) ) ;
#18679 = CARTESIAN_POINT ( 'NONE',  ( 0.2924095564367995559, 116.4254662015451913, 0.005843038833676869777 ) ) ;
#18680 = ORIENTED_EDGE ( 'NONE', *, *, #10292, .T. ) ;
#18681 = CARTESIAN_POINT ( 'NONE',  ( 4.377640660406503237, 26.40621510375495973, 1.544744264128281364 ) ) ;
#18682 = CARTESIAN_POINT ( 'NONE',  ( -30.03238267955204677, 57.98137616130296834, 1.269999999999994023 ) ) ;
#18683 = CARTESIAN_POINT ( 'NONE',  ( -43.04734275525326126, 21.71211564561782481, 2.244749861970594118 ) ) ;
#18684 = DIRECTION ( 'NONE',  ( -0.5149185422762211362, 0.8572391118119444542, 0.000000000000000000 ) ) ;
#18685 = CARTESIAN_POINT ( 'NONE',  ( 6.994627636368861978, 121.9501463612105425, 0.2166421691076159950 ) ) ;
#18686 = CARTESIAN_POINT ( 'NONE',  ( -3.990024091077861268, 18.91925256873344807, 2.329872802929966902 ) ) ;
#18687 = CARTESIAN_POINT ( 'NONE',  ( 22.64839633469820868, 142.3612397021088611, 1.542087416992684146 ) ) ;
#18688 = CARTESIAN_POINT ( 'NONE',  ( -6.135835944515187101, 77.40800365160224317, 1.524000000000003130 ) ) ;
#18690 = CARTESIAN_POINT ( 'NONE',  ( 21.33845497820654202, 148.5140355411650717, -1.460612514688959029 ) ) ;
#18689 = CARTESIAN_POINT ( 'NONE',  ( 5.511339492779238292, 57.14999999999997016, 5.111277471990169907 ) ) ;
#18691 = CARTESIAN_POINT ( 'NONE',  ( -9.322612814602798892, 121.5662863950884400, 1.087844926965479964 ) ) ;
#18692 = CARTESIAN_POINT ( 'NONE',  ( -0.9239673467531356321, 25.61616486456964736, -4.531977062890359065 ) ) ;
#18693 = CARTESIAN_POINT ( 'NONE',  ( -22.26995438616712519, 150.5193240506149550, -1.407572089812798799 ) ) ;
#18694 = CARTESIAN_POINT ( 'NONE',  ( -0.8879284396340286767, 8.347861319067646946, 0.4041202799994399464 ) ) ;
#18695 = ORIENTED_EDGE ( 'NONE', *, *, #28163, .F. ) ;
#18696 = CARTESIAN_POINT ( 'NONE',  ( -55.75614604655159923, 4.795084387130554404, 1.238208353029749853 ) ) ;
#18697 = CARTESIAN_POINT ( 'NONE',  ( -3.676778326629141169, 120.9289264519876070, 0.1742216996082329994 ) ) ;
#18698 = CARTESIAN_POINT ( 'NONE',  ( 4.549387865739121573, -13.93190642666217194, 4.188617477609191120 ) ) ;
#18699 = CARTESIAN_POINT ( 'NONE',  ( 10.40651172546656333, 123.5464890276372785, -0.9122707376378307309 ) ) ;
#18700 = ORIENTED_EDGE ( 'NONE', *, *, #22369, .F. ) ;
#18701 = CARTESIAN_POINT ( 'NONE',  ( 1.900651210107762834, 115.7024232297718100, 1.719628578966114096 ) ) ;
#18702 = CARTESIAN_POINT ( 'NONE',  ( -4.716505708007757036, 117.7575842814051299, -1.081295402246875037 ) ) ;
#18703 = CARTESIAN_POINT ( 'NONE',  ( -7.220421660630267272E-14, 120.9974662015457341, -1.809054757420055726E-18 ) ) ;
#18705 = VERTEX_POINT ( 'NONE', #24687 ) ;
#18704 = AXIS2_PLACEMENT_3D ( 'NONE', #15481, #34881, #15264 ) ;
#18706 = CARTESIAN_POINT ( 'NONE',  ( 1.216597929035199588, 118.5604221528582372, 0.6894197161374838734 ) ) ;
#18707 = CARTESIAN_POINT ( 'NONE',  ( 14.95453923199683111, 61.75387968257833649, -5.016499999999999737 ) ) ;
#18708 = DIRECTION ( 'NONE',  ( -0.9998004120163609398, 0.000000000000000000, -0.01997839162482749689 ) ) ;
#18709 = CARTESIAN_POINT ( 'NONE',  ( 4.995400918032669502, 117.4677412550548610, -0.7873132084926519614 ) ) ;
#18710 = CARTESIAN_POINT ( 'NONE',  ( 23.04498962259524930, 149.8694456586574972, 0.007884547560928708426 ) ) ;
#18711 = CARTESIAN_POINT ( 'NONE',  ( -5.177913976931287188, 57.15000000000002700, -5.372100000000004094 ) ) ;
#18712 = CARTESIAN_POINT ( 'NONE',  ( -46.90713744787128547, 25.32984766614545080, 1.752173880707143860 ) ) ;
#18713 = CARTESIAN_POINT ( 'NONE',  ( 5.777868923222713171, 78.89722547516475970, 5.030779815616707396 ) ) ;
#18714 = B_SPLINE_CURVE_WITH_KNOTS ( 'NONE', 3,
 ( #15530, #28320, #31726, #5341 ),
 .UNSPECIFIED., .F., .F.,
 ( 4, 4 ),
 ( 0.4905041263739809976, 1.000000000000000000 ),
 .UNSPECIFIED. ) ;
#18715 = CARTESIAN_POINT ( 'NONE',  ( 1.740647812522833959, -15.18628559522394639, 5.503367792502267264 ) ) ;
#18716 = CARTESIAN_POINT ( 'NONE',  ( -44.66298991629287940, 23.47648082339880915, 1.964675176939932655 ) ) ;
#18717 = DIRECTION ( 'NONE',  ( 9.627370216492862708E-17, 1.000000000000000000, -0.000000000000000000 ) ) ;
#18718 = CARTESIAN_POINT ( 'NONE',  ( -4.555200029879727275, 118.0893311008628501, 0.5840147855654914677 ) ) ;
#18719 = B_SPLINE_CURVE_WITH_KNOTS ( 'NONE', 3,
 ( #10701, #14105, #37326, #27104, #14519, #11538, #40536, #39908, #27729, #24318, #7940, #23681, #7523, #20700, #33724, #8141 ),
 .UNSPECIFIED., .F., .F.,
 ( 4, 2, 1, 1, 2, 2, 2, 2, 4 ),
 ( 0.000000000000000000, 0.06250000000000000000, 0.1250000000000000000, 0.2500000000000000000, 0.5000000000000000000, 0.6250000000000000000, 0.7500000000000000000, 0.8750000000000000000, 1.000000000000000000 ),
 .UNSPECIFIED. ) ;
#18720 = ORIENTED_EDGE ( 'NONE', *, *, #2932, .T. ) ;
#18721 = CARTESIAN_POINT ( 'NONE',  ( -0.7080441033280816532, 118.7629491485454025, 1.246623510331355211 ) ) ;
#18722 = CARTESIAN_POINT ( 'NONE',  ( -3.504900662208191520, 118.6790270643119527, -0.9350548551792551288 ) ) ;
#18723 = CARTESIAN_POINT ( 'NONE',  ( -2.643983731439692786, 108.0685014782224442, -4.389169220726125253 ) ) ;
#18724 = CARTESIAN_POINT ( 'NONE',  ( 4.642288039849367998, 117.9634434738006092, 0.9175853795829764792 ) ) ;
#18725 = CARTESIAN_POINT ( 'NONE',  ( 1.979187190576821465, -15.21425526833739639, 5.301287498526151332 ) ) ;
#18726 = CARTESIAN_POINT ( 'NONE',  ( -0.3781434503562681737, 120.9711055683163323, 0.4753422346318208480 ) ) ;
#18727 = CARTESIAN_POINT ( 'NONE',  ( 1.968029828064305153, -3.592386099649644837, 4.203610184747879508 ) ) ;
#18728 = CARTESIAN_POINT ( 'NONE',  ( 4.814838716269237651, 117.4047667081807305, -1.012532368900667556 ) ) ;
#18729 = CARTESIAN_POINT ( 'NONE',  ( -5.871452009091383317, 57.14999999999997016, -5.016499999999999737 ) ) ;
#18730 = CARTESIAN_POINT ( 'NONE',  ( 1.441108623025248781, 106.3840144300045409, -5.062828720429449980 ) ) ;
#18731 = CARTESIAN_POINT ( 'NONE',  ( -5.146579651471840045, 156.3268443366877989, -1.619031734741227968 ) ) ;
#18732 = CARTESIAN_POINT ( 'NONE',  ( 6.078424119085688027, 121.4421096791099188, 0.1217658744218859945 ) ) ;
#18733 = CARTESIAN_POINT ( 'NONE',  ( 0.4675636154070875738, 39.04908508565743830, 1.310637636393764627 ) ) ;
#18734 = AXIS2_PLACEMENT_3D ( 'NONE', #27861, #24657, #40663 ) ;
#18735 = CARTESIAN_POINT ( 'NONE',  ( -4.855072294470597072, 115.7029491485453718, 1.279409886141102071 ) ) ;
#18736 = CARTESIAN_POINT ( 'NONE',  ( 4.087030650986479330, 6.990161447142720696, 2.163025551504125232 ) ) ;
#18738 = ORIENTED_EDGE ( 'NONE', *, *, #17768, .F. ) ;
#18737 = CARTESIAN_POINT ( 'NONE',  ( 9.693497654998099122, 118.1218853900603136, 0.6301662642801912906 ) ) ;
#18739 = CARTESIAN_POINT ( 'NONE',  ( -0.1152527507162018766, 104.6144662015368851, -5.344087831667617472 ) ) ;
#18740 = CARTESIAN_POINT ( 'NONE',  ( 4.222520559145931607, -15.42613134656034646, 1.120547993087879446 ) ) ;
#18741 = CARTESIAN_POINT ( 'NONE',  ( -15.49426794143308683, 128.5596447653542498, 1.561415741013214120 ) ) ;
#18742 = CARTESIAN_POINT ( 'NONE',  ( -0.2169513509689728059, 19.34598098455444770, 0.9497947498389193166 ) ) ;
#18743 = CARTESIAN_POINT ( 'NONE',  ( 0.6244633603679663469, 9.902617207799803367, -0.7572168304597820532 ) ) ;
#18744 = EDGE_CURVE ( 'NONE', #38897, #22759, #37695, .T. ) ;
#18745 = EDGE_CURVE ( 'NONE', #22648, #15317, #13688, .T. ) ;
#18746 = VERTEX_POINT ( 'NONE', #35133 ) ;
#18747 = VERTEX_POINT ( 'NONE', #5960 ) ;
#18748 = CARTESIAN_POINT ( 'NONE',  ( -4.908369780149227424, 117.6445054487819704, -0.9443798348817722399 ) ) ;
#18749 = CARTESIAN_POINT ( 'NONE',  ( 0.7907262360440370230, 106.8474934270474392, 4.937153267606968932 ) ) ;
#18750 = SURFACE_SIDE_STYLE ('',( #2601 ) ) ;
#18751 = CARTESIAN_POINT ( 'NONE',  ( -11.19133892028646926, 126.1638007343821641, 0.6664143115430061215 ) ) ;
#18752 = CARTESIAN_POINT ( 'NONE',  ( 3.427377709871179512, -13.85078959623727002, 3.379007147668904754 ) ) ;
#18753 = CARTESIAN_POINT ( 'NONE',  ( 14.94938132205795789, 131.2528086460777388, -1.477614431843955467 ) ) ;
#18754 = CARTESIAN_POINT ( 'NONE',  ( -11.40914533023179800, 121.1873859956591843, -1.678693868224012009 ) ) ;
#18755 = DIRECTION ( 'NONE',  ( -0.8745520943968240202, 0.4849315768086553402, -5.361993529360572958E-16 ) ) ;
#18756 = CARTESIAN_POINT ( 'NONE',  ( 7.869695484959776444, 122.1458944043033057, 0.8493936842156786238 ) ) ;
#18757 = CARTESIAN_POINT ( 'NONE',  ( -3.202519050486192231, 34.47767571226007277, 3.235088606727665184 ) ) ;
#18758 = CARTESIAN_POINT ( 'NONE',  ( 13.04043193504457498, 133.9378623523624299, -0.05483593244790751359 ) ) ;
#18759 = VERTEX_POINT ( 'NONE', #5333 ) ;
#18760 = CARTESIAN_POINT ( 'NONE',  ( -2.163474658736635359, 107.1110135075344942, -4.788244450165834998 ) ) ;
#18761 = CARTESIAN_POINT ( 'NONE',  ( 1.247998466936322838E-15, 12.96302561210691806, 0.000000000000000000 ) ) ;
#18762 = CARTESIAN_POINT ( 'NONE',  ( -21.32888081312384898, 55.91420173801096638, -1.270000000000000240 ) ) ;
#18763 = CARTESIAN_POINT ( 'NONE',  ( 4.906163051172606870, 117.7581308566543186, -0.5365533941472381274 ) ) ;
#18764 = B_SPLINE_CURVE_WITH_KNOTS ( 'NONE', 3,
 ( #22408, #33084, #3274, #83, #15821, #19228, #37870, #21657, #34682, #8904 ),
 .UNSPECIFIED., .F., .F.,
 ( 4, 2, 2, 2, 4 ),
 ( -0.0004895961982421346420, 0.0005229314014804247769, 0.001535459001202984196, 0.002547986600925542747, 0.003560514200648101299 ),
 .UNSPECIFIED. ) ;
#18765 = VECTOR ( 'NONE', #3507, 1000.000000000000114 ) ;
#18766 = CARTESIAN_POINT ( 'NONE',  ( 7.630415381941168640, 23.66608445915806058, -3.560124470299026900 ) ) ;
#18767 = CARTESIAN_POINT ( 'NONE',  ( -0.007600002268445282295, 120.2037396364829505, 0.3803351912374557386 ) ) ;
#18768 = DIRECTION ( 'NONE',  ( 0.000000000000000000, 1.000000000000000000, 0.000000000000000000 ) ) ;
#18769 = CARTESIAN_POINT ( 'NONE',  ( 11.72569139212691169, 118.7251779360019270, 0.1869994294823658365 ) ) ;
#18770 = CARTESIAN_POINT ( 'NONE',  ( -7.475619626241609694, 123.6620266863018855, -0.1149006695610368389 ) ) ;
#18771 = DIRECTION ( 'NONE',  ( 0.9998004120163609398, 0.000000000000000000, 0.01997839162482749689 ) ) ;
#18772 = CARTESIAN_POINT ( 'NONE',  ( 0.6412933796112577634, 156.3034662015457741, 0.01281456791805622546 ) ) ;
#18773 = ADVANCED_FACE ( 'NONE', ( #37476 ), #2350, .T. ) ;
#18774 = CARTESIAN_POINT ( 'NONE',  ( 7.865828698536367902, -6.344330755464622662, 3.006797519310529854 ) ) ;
#18775 = CARTESIAN_POINT ( 'NONE',  ( -2.140231652025115672, 116.5286393870344028, -0.3979261928235908741 ) ) ;
#18776 = CARTESIAN_POINT ( 'NONE',  ( -0.3991458833605321943, 123.7646714092001190, -0.1312610764096185101 ) ) ;
#18777 = DIRECTION ( 'NONE',  ( -0.7770581983690878491, 0.6294287539883980376, -5.101669463485847584E-16 ) ) ;
#18778 = CARTESIAN_POINT ( 'NONE',  ( -17.14500000000466784, 71.11999999999886768, 1.269999999999998241 ) ) ;
#18779 = CARTESIAN_POINT ( 'NONE',  ( 8.411406395146093118, -11.38171290258811119, -0.9481482025471229536 ) ) ;
#18780 = CARTESIAN_POINT ( 'NONE',  ( 0.4906649483725750716, 117.9394484190330843, 1.408234383443731641 ) ) ;
#18781 = CARTESIAN_POINT ( 'NONE',  ( 3.682264917456193221, 78.83346620154574680, 0.07358041635424013294 ) ) ;
#18782 = CARTESIAN_POINT ( 'NONE',  ( 4.997525182441555636, 56.61525291752811029, -5.184946129310890051 ) ) ;
#18783 = CARTESIAN_POINT ( 'NONE',  ( 0.4023205627559981457, 108.3383513567250986, -4.340400160729728007 ) ) ;
#18784 = CARTESIAN_POINT ( 'NONE',  ( -1.391432384042666337, 159.5643428290674990, 0.4004207282219807706 ) ) ;
#18785 = ORIENTED_EDGE ( 'NONE', *, *, #42044, .T. ) ;
#18786 = CARTESIAN_POINT ( 'NONE',  ( -58.83227707057486811, -0.08366279997995551554, -5.898546760656774196E-15 ) ) ;
#18787 = ORIENTED_EDGE ( 'NONE', *, *, #33646, .F. ) ;
#18788 = CARTESIAN_POINT ( 'NONE',  ( -42.07367843439164545, 22.17357734922909529, -1.489526742666034576 ) ) ;
#18789 = CARTESIAN_POINT ( 'NONE',  ( -15.64525404011971332, 147.2221590072177548, -0.1788206097943383921 ) ) ;
#18790 = CARTESIAN_POINT ( 'NONE',  ( 4.016706779461339138, -15.37834506377831723, 5.009826762111060816 ) ) ;
#18791 = CARTESIAN_POINT ( 'NONE',  ( -6.779039758441160579, 118.9580315507705706, 0.9776869392460788566 ) ) ;
#18792 = CARTESIAN_POINT ( 'NONE',  ( 4.901524533163292396, 117.5843641943970681, -0.6192240155325964279 ) ) ;
#18793 = CARTESIAN_POINT ( 'NONE',  ( 3.728136974946417492, 6.765255174955887796, 2.739693761753763113 ) ) ;
#18794 = AXIS2_PLACEMENT_3D ( 'NONE', #25762, #32579, #25354 ) ;
#18795 = EDGE_CURVE ( 'NONE', #23884, #35416, #21801, .T. ) ;
#18796 = CARTESIAN_POINT ( 'NONE',  ( -53.83932746694286919, 9.555192732579641302, -3.787265504858273513 ) ) ;
#18797 = ORIENTED_EDGE ( 'NONE', *, *, #5598, .T. ) ;
#18798 = AXIS2_PLACEMENT_3D ( 'NONE', #30361, #24170, #39771 ) ;
#18799 = CARTESIAN_POINT ( 'NONE',  ( -4.801770124281918406, 117.3993836135855133, 1.016061139389656587 ) ) ;
#18800 = CARTESIAN_POINT ( 'NONE',  ( -13.85159022459153988, 59.63164443796365077, -5.016499999999999737 ) ) ;
#18801 = CARTESIAN_POINT ( 'NONE',  ( -6.570524231284120553, 120.8223817900871495, 0.7604033795411313523 ) ) ;
#18802 = CARTESIAN_POINT ( 'NONE',  ( 5.149812983838432778, 116.8469558424508534, 0.1790270373415662197 ) ) ;
#18803 = CARTESIAN_POINT ( 'NONE',  ( 7.566762702257193496, 120.1328256275108828, -1.061688055624673721 ) ) ;
#18804 = CARTESIAN_POINT ( 'NONE',  ( -16.78381336521981382, 153.6818489539412553, -2.151947388239846770 ) ) ;
#18805 = CARTESIAN_POINT ( 'NONE',  ( -53.68435271313694557, 11.12367579685427721, -3.945100831076026715 ) ) ;
#18806 = ADVANCED_FACE ( 'NONE', ( #15521, #5539 ), #24902, .F. ) ;
#18807 = CARTESIAN_POINT ( 'NONE',  ( 11.89914747278627161, 128.3619849303985632, -0.5991027734528262538 ) ) ;
#18808 = B_SPLINE_CURVE_WITH_KNOTS ( 'NONE', 3,
 ( #2274, #2696, #28021, #8224 ),
 .UNSPECIFIED., .F., .F.,
 ( 4, 4 ),
 ( 0.000000000000000000, 0.9716897010375963317 ),
 .UNSPECIFIED. ) ;
#18809 = ORIENTED_EDGE ( 'NONE', *, *, #18744, .F. ) ;
#18810 = CARTESIAN_POINT ( 'NONE',  ( -16.72996320514150881, 149.5530097695598215, -2.252745029998447723 ) ) ;
#18811 = CARTESIAN_POINT ( 'NONE',  ( 2.686089547800571964, -15.51909802064466248, 4.724564614977055044 ) ) ;
#18812 = CARTESIAN_POINT ( 'NONE',  ( -4.110765650185568276, 118.2429491485452928, -0.3474004633102953932 ) ) ;
#18813 = VECTOR ( 'NONE', #39209, 1000.000000000000000 ) ;
#18814 = CARTESIAN_POINT ( 'NONE',  ( -47.85244527695891037, 19.39403540832952544, -5.219971639306605127 ) ) ;
#18815 = PRODUCT_RELATED_PRODUCT_CATEGORY ( 'part', '', ( #20129 ) ) ;
#18816 = CARTESIAN_POINT ( 'NONE',  ( -4.815039658666428579, 117.6402044532089377, 0.9372080113549726699 ) ) ;
#18817 = CARTESIAN_POINT ( 'NONE',  ( 8.183297913988958783, 121.2453320564195280, 1.294587653635732138 ) ) ;
#18818 = CARTESIAN_POINT ( 'NONE',  ( 20.83467972660109169, 65.95194780259438971, -5.016499999999999737 ) ) ;
#18819 =( BOUNDED_CURVE ( )  B_SPLINE_CURVE ( 3, ( #35314, #3151, #31693, #12725 ),
 .UNSPECIFIED., .F., .T. ) 
 B_SPLINE_CURVE_WITH_KNOTS ( ( 4, 4 ),
 ( 0.4854033284062813647, 0.4997054356531658859 ),
 .UNSPECIFIED. ) 
 CURVE ( )  GEOMETRIC_REPRESENTATION_ITEM ( )  RATIONAL_B_SPLINE_CURVE ( ( 0.9433178161976487619, 0.9612738889930489972, 0.9797754291796525461, 0.9988224367574596307 ) ) 
 REPRESENTATION_ITEM ( '' )  );
#18820 = VECTOR ( 'NONE', #34870, 1000.000000000000114 ) ;
#18821 = CARTESIAN_POINT ( 'NONE',  ( 7.890306666665830804, -2.504341373917490898, 2.985612812370990632 ) ) ;
#18822 = CARTESIAN_POINT ( 'NONE',  ( 15.75631923737907947, 146.9135488020124001, 0.6449975968329650922 ) ) ;
#18823 = CARTESIAN_POINT ( 'NONE',  ( -20.37123700195716225, 79.57406833244878896, 1.269999999999995355 ) ) ;
#18824 = EDGE_CURVE ( 'NONE', #2670, #3374, #18919, .T. ) ;
#18825 = CIRCLE ( 'NONE', #20189, 0.2540000000000000036 ) ;
#18826 = EDGE_CURVE ( 'NONE', #27965, #10570, #10276, .T. ) ;
#18827 = CARTESIAN_POINT ( 'NONE',  ( -45.52520984822221095, 18.49555408152312452, -0.5880787195337440210 ) ) ;
#18828 = DIRECTION ( 'NONE',  ( -0.4849315768086535083, -0.8745520943968250194, -1.030032898892974695E-16 ) ) ;
#18829 = CARTESIAN_POINT ( 'NONE',  ( -57.24023649071029496, 3.661034843983918208, 2.195083147259549339 ) ) ;
#18830 = CARTESIAN_POINT ( 'NONE',  ( -56.41464036832825713, 4.421983009390323183, 2.556334463401503054 ) ) ;
#18831 = FACE_OUTER_BOUND ( 'NONE', #8038, .T. ) ;
#18832 = EDGE_CURVE ( 'NONE', #26111, #30442, #27275, .T. ) ;
#18833 = CARTESIAN_POINT ( 'NONE',  ( -29.82321757229076908, 71.17901112636586447, -1.270000000000007123 ) ) ;
#18834 = CARTESIAN_POINT ( 'NONE',  ( -52.19327494808134560, 16.79818233314609444, 2.080405417473075946 ) ) ;
#18835 = CARTESIAN_POINT ( 'NONE',  ( -22.97142009758403702, 150.1545470440437953, -0.2295619762022473587 ) ) ;
#18836 = ORIENTED_EDGE ( 'NONE', *, *, #2411, .T. ) ;
#18837 = CARTESIAN_POINT ( 'NONE',  ( -50.25741847910705928, 21.95975045971864503, -0.7628348698132428884 ) ) ;
#18838 = CARTESIAN_POINT ( 'NONE',  ( 5.997220096930487188, 121.4340474584781333, 0.01630150470699537335 ) ) ;
#18839 = DIRECTION ( 'NONE',  ( 0.9849462604886047856, 0.000000000000000000, -0.1728608224830407714 ) ) ;
#18840 = VERTEX_POINT ( 'NONE', #18497 ) ;
#18841 = CARTESIAN_POINT ( 'NONE',  ( 0.6554072075965952093, 115.7029491485453718, -1.735615680197917010 ) ) ;
#18842 = CARTESIAN_POINT ( 'NONE',  ( -4.578033532675611639, 121.1907927009877000, -0.1597499619731679310 ) ) ;
#18843 = CARTESIAN_POINT ( 'NONE',  ( 5.214050246812039546, -13.77884693253300696, 3.484500232556287269 ) ) ;
#18844 = CARTESIAN_POINT ( 'NONE',  ( -4.024684254631618607, 117.9114980025989752, 0.7134393008021915339 ) ) ;
#18845 = LINE ( 'NONE', #29280, #24733 ) ;
#18846 = CARTESIAN_POINT ( 'NONE',  ( -0.002459401150369191873, 159.6023738651833810, 0.1230784904792619899 ) ) ;
#18847 = VECTOR ( 'NONE', #11353, 1000.000000000000227 ) ;
#18848 = CARTESIAN_POINT ( 'NONE',  ( 10.39028434690761671, 153.1476064233308989, 0.3279402672483373582 ) ) ;
#18849 = CARTESIAN_POINT ( 'NONE',  ( -0.9676832378731173856, 3.540085264489355676, -0.1409938603398425416 ) ) ;
#18850 = CARTESIAN_POINT ( 'NONE',  ( -11.72380150228551976, 118.7251779360019270, -0.2815772452395033931 ) ) ;
#18851 = CARTESIAN_POINT ( 'NONE',  ( -6.376221727585796537E-14, 51.14746620154573264, 5.777789833161707559E-29 ) ) ;
#18852 = CARTESIAN_POINT ( 'NONE',  ( -5.913343974123855595, 116.9636705795739573, -0.1181626924810776913 ) ) ;
#18853 = ORIENTED_EDGE ( 'NONE', *, *, #2446, .F. ) ;
#18854 = CARTESIAN_POINT ( 'NONE',  ( 8.718793965502175780, 118.0120498888943246, 0.7790975575022228705 ) ) ;
#18855 = DIRECTION ( 'NONE',  ( -1.000000000000000000, 0.000000000000000000, 4.553079989440437711E-16 ) ) ;
#18856 = CARTESIAN_POINT ( 'NONE',  ( 20.18025034597661715, 150.8812763393641490, 2.199297964380012349 ) ) ;
#18857 = AXIS2_PLACEMENT_3D ( 'NONE', #32511, #6525, #25490 ) ;
#18858 = CARTESIAN_POINT ( 'NONE',  ( 12.60853345059990538, 122.2722385251898771, -1.300450782769299707 ) ) ;
#18859 = CARTESIAN_POINT ( 'NONE',  ( 2.488832714281139946, 5.747567886007050042, -8.044950587805361764 ) ) ;
#18860 = CARTESIAN_POINT ( 'NONE',  ( -21.58117366275210003, 150.4657531037631486, -1.865176240683389608 ) ) ;
#18861 = CARTESIAN_POINT ( 'NONE',  ( 4.763862057462126209, 117.8479813596402295, -0.8127542836191120612 ) ) ;
#18862 = CARTESIAN_POINT ( 'NONE',  ( 6.308735553862782730, 120.0717973201777511, 0.4535485300176086976 ) ) ;
#18863 = VECTOR ( 'NONE', #19212, 1000.000000000000000 ) ;
#18864 = CARTESIAN_POINT ( 'NONE',  ( -11.86471938700715256, 151.9842433124228762, -0.02191723269355095108 ) ) ;
#18865 = CARTESIAN_POINT ( 'NONE',  ( -18.57470247777332872, 148.7425187291823363, -2.467219961595396693 ) ) ;
#18866 = CARTESIAN_POINT ( 'NONE',  ( 4.647714231081432779, -15.48178215826023774, 3.998406189266252131 ) ) ;
#18867 = DIRECTION ( 'NONE',  ( -0.9998004120163609398, -4.016384292689130894E-17, -0.01997839162482749689 ) ) ;
#18868 = CARTESIAN_POINT ( 'NONE',  ( -1.940560682967259032, 118.1651005317671945, -0.8495063313247263048 ) ) ;
#18869 = EDGE_CURVE ( 'NONE', #7108, #39553, #21138, .T. ) ;
#18870 = VERTEX_POINT ( 'NONE', #14886 ) ;
#18871 = CARTESIAN_POINT ( 'NONE',  ( 10.55536611456372320, 121.9340018749941663, 1.633389464556823878 ) ) ;
#18872 = DIRECTION ( 'NONE',  ( -3.035386659626960118E-16, 0.000000000000000000, -1.000000000000000000 ) ) ;
#18873 = DIRECTION ( 'NONE',  ( 9.627370216492862708E-17, 1.000000000000000000, -0.000000000000000000 ) ) ;
#18874 = AXIS2_PLACEMENT_3D ( 'NONE', #21148, #32975, #29970 ) ;
#18875 = CARTESIAN_POINT ( 'NONE',  ( -5.854232237047567011, 124.7508695889173111, -0.1141955550013106363 ) ) ;
#18876 = CARTESIAN_POINT ( 'NONE',  ( -3.806420843250353681, -2.673146571556306750, -7.510622214715559686 ) ) ;
#18877 = CARTESIAN_POINT ( 'NONE',  ( 10.75107117262875533, 153.0872561326487187, 1.097343645257591760 ) ) ;
#18878 = CARTESIAN_POINT ( 'NONE',  ( 0.009748065369121088064, 159.5507987164374981, -0.4878330526048096361 ) ) ;
#18879 = CARTESIAN_POINT ( 'NONE',  ( 5.177913976931208140, 56.51499999999997925, -5.372099999999992548 ) ) ;
#18880 = CARTESIAN_POINT ( 'NONE',  ( -58.36517903063335666, -0.2819031691279192398, 0.08479348624783289434 ) ) ;
#18881 = CARTESIAN_POINT ( 'NONE',  ( 5.565051029437463548, 116.7025977693256351, 0.02599261142907015321 ) ) ;
#18882 = EDGE_CURVE ( 'NONE', #12419, #36071, #37978, .T. ) ;
#18883 = CARTESIAN_POINT ( 'NONE',  ( -4.468667403750213651, 27.88063884994054220, 0.5133561255362272258 ) ) ;
#18884 = CARTESIAN_POINT ( 'NONE',  ( -3.703049682113393359, 116.6240124373522065, -0.07399574541707870656 ) ) ;
#18885 = EDGE_CURVE ( 'NONE', #34968, #32786, #18653, .T. ) ;
#18886 = EDGE_LOOP ( 'NONE', ( #39556, #2730, #30086, #35546 ) ) ;
#18887 = CARTESIAN_POINT ( 'NONE',  ( 4.513834119875788531, 119.5960505434745613, -0.7443551714737827174 ) ) ;
#18888 = CARTESIAN_POINT ( 'NONE',  ( 5.304438957985845526, 116.0444662015456885, -1.082911341041116637 ) ) ;
#18889 = CARTESIAN_POINT ( 'NONE',  ( -5.891535241408227819, 121.4229528491920576, -0.4202535615248633172 ) ) ;
#18890 = CARTESIAN_POINT ( 'NONE',  ( 7.784012320830338005, 122.6313477005580665, 0.1555430910899518460 ) ) ;
#18891 = CARTESIAN_POINT ( 'NONE',  ( 15.72148175706224826, 120.8394623874526275, 0.3311059221235125305 ) ) ;
#18892 = ORIENTED_EDGE ( 'NONE', *, *, #1368, .F. ) ;
#18893 = CARTESIAN_POINT ( 'NONE',  ( -4.151662239014343392, 13.23730288530712862, 2.070234887608822572 ) ) ;
#18894 = CARTESIAN_POINT ( 'NONE',  ( -31.80708539008069735, 53.04900798501882520, 1.523999999999994914 ) ) ;
#18895 = CARTESIAN_POINT ( 'NONE',  ( -4.999848113220977552, 117.4046874637221833, 0.8305944942939621489 ) ) ;
#18896 = CARTESIAN_POINT ( 'NONE',  ( -10.23480564747663379, 76.83082906289159553, 1.270000000000000906 ) ) ;
#18897 = FACE_OUTER_BOUND ( 'NONE', #33462, .T. ) ;
#18898 = CARTESIAN_POINT ( 'NONE',  ( 7.802483560484270164, 122.5107354630703185, 0.4689056730029690367 ) ) ;
#18899 = CARTESIAN_POINT ( 'NONE',  ( 4.103230867730633058, 22.16771668783608007, 2.168033597859526651 ) ) ;
#18900 = CARTESIAN_POINT ( 'NONE',  ( 12.90531570856114207, 156.9034992427187376, 1.273604633583561796 ) ) ;
#18901 = CARTESIAN_POINT ( 'NONE',  ( -4.378631914228641620, 104.6144662015457243, -2.055837668634139970 ) ) ;
#18903 = CARTESIAN_POINT ( 'NONE',  ( 15.35657197080316294, 154.8698957928756954, -1.403577372161787906 ) ) ;
#18902 = CARTESIAN_POINT ( 'NONE',  ( 1.761579046708144691, 106.7079731062244718, 4.966399410128932601 ) ) ;
#18904 = CARTESIAN_POINT ( 'NONE',  ( -11.57150582532061378, 123.3156264706956478, 1.212837404772455274 ) ) ;
#18905 = CARTESIAN_POINT ( 'NONE',  ( 1.677595020332960152, 24.74158224480939339, -4.309653081027373211 ) ) ;
#18906 = CARTESIAN_POINT ( 'NONE',  ( -22.44014329066014568, 150.2745577238280816, -1.412889903812419412 ) ) ;
#18907 = COLOUR_RGB ( '', 0.08235294, 0.09019608, 0.10196078) ;
#18908 = ORIENTED_EDGE ( 'NONE', *, *, #32116, .T. ) ;
#18909 = CARTESIAN_POINT ( 'NONE',  ( -56.42856387642239469, 3.193865871111076338, -9.870345732644628497E-15 ) ) ;
#18910 = CARTESIAN_POINT ( 'NONE',  ( -15.47786622725302941, 148.0679034673509875, 0.4116497765502036832 ) ) ;
#18911 = CARTESIAN_POINT ( 'NONE',  ( 5.472227756958008449, -13.43587746834383445, 2.852490916751204697 ) ) ;
#18912 = CARTESIAN_POINT ( 'NONE',  ( 16.58715205660926983, 148.2569838091642964, -1.247478730927799484 ) ) ;
#18913 = VECTOR ( 'NONE', #10392, 1000.000000000000114 ) ;
#18914 = CARTESIAN_POINT ( 'NONE',  ( -4.663648155852026633, 118.0052748788920383, -0.7714184625502767956 ) ) ;
#18915 = CARTESIAN_POINT ( 'NONE',  ( 9.108749339472423046, 153.9337724597031070, 0.1375672075132169658 ) ) ;
#18916 = ORIENTED_EDGE ( 'NONE', *, *, #7992, .F. ) ;
#18917 = CARTESIAN_POINT ( 'NONE',  ( 6.391991208684993708, 157.5392376370035095, 1.942695856706931679 ) ) ;
#18918 = DIRECTION ( 'NONE',  ( 0.01731298258488073519, -0.9998501190848635423, 1.788962107505278613E-16 ) ) ;
#18919 = LINE ( 'NONE', #21899, #30006 ) ;
#18920 = CARTESIAN_POINT ( 'NONE',  ( 5.005702202344075147, 117.4009237673399610, -0.7895530272732956822 ) ) ;
#18921 = CARTESIAN_POINT ( 'NONE',  ( 23.22010346901273792, 149.3105122542552863, 0.009921264925044916486 ) ) ;
#18922 = EDGE_CURVE ( 'NONE', #26382, #26813, #25231, .T. ) ;
#18923 = DIRECTION ( 'NONE',  ( -1.000000000000000000, 0.000000000000000000, 0.000000000000000000 ) ) ;
#18924 = CARTESIAN_POINT ( 'NONE',  ( -11.58677707360137354, 55.24499999999999034, 4.474811398758258285 ) ) ;
#18925 = PRODUCT_DEFINITION_FORMATION_WITH_SPECIFIED_SOURCE ( 'ANY', '', #4534, .NOT_KNOWN. ) ;
#18926 = CARTESIAN_POINT ( 'NONE',  ( 5.583532163259939729, 78.91300747758680245, 5.082153855702582490 ) ) ;
#18928 = EDGE_CURVE ( 'NONE', #4992, #19512, #4885, .T. ) ;
#18927 = CARTESIAN_POINT ( 'NONE',  ( 2.003160442218029136, -15.10791216010797022, 5.854173571448314739 ) ) ;
#18929 = CARTESIAN_POINT ( 'NONE',  ( -46.67659519887701691, 22.71018310752411651, 3.598098858967599512 ) ) ;
#18930 = CARTESIAN_POINT ( 'NONE',  ( -10.92199999999999704, 55.24499999999999034, 0.000000000000000000 ) ) ;
#18931 = CARTESIAN_POINT ( 'NONE',  ( -4.595531677754072675, 118.0173238459723990, 0.6950376821852393139 ) ) ;
#18932 = EDGE_LOOP ( 'NONE', ( #4203, #3212, #24913, #35256 ) ) ;
#18933 = EDGE_LOOP ( 'NONE', ( #8716, #8564, #2144, #28723, #3352 ) ) ;
#18934 = CARTESIAN_POINT ( 'NONE',  ( -0.3690176902731273079, 115.6909491485452435, -1.766244235947253216 ) ) ;
#18935 = CIRCLE ( 'NONE', #33930, 15.21260244842765808 ) ;
#18936 = CARTESIAN_POINT ( 'NONE',  ( 3.677254471647890099, 118.8081103207223350, -0.7906174721324027432 ) ) ;
#18937 = CARTESIAN_POINT ( 'NONE',  ( -5.429077642219940714, 122.7706071131974994, -0.2216225483982831312 ) ) ;
#18938 = CARTESIAN_POINT ( 'NONE',  ( 4.721342683323704215, 117.8485734799888291, 1.008627725644892559 ) ) ;
#18939 = CIRCLE ( 'NONE', #8076, 14.73199999999999577 ) ;
#18940 = CARTESIAN_POINT ( 'NONE',  ( 3.220330141560203696, -14.30903721375789317, 2.546581355196453345 ) ) ;
#18941 = CARTESIAN_POINT ( 'NONE',  ( 0.01596947694123658501, 156.4635559983122448, -0.7991779281049287142 ) ) ;
#18942 = SURFACE_STYLE_USAGE ( .BOTH. , #38350 ) ;
#18943 = CARTESIAN_POINT ( 'NONE',  ( -0.2371737209061060558, 105.9787871742262979, 5.291462458420934212 ) ) ;
#18944 = DIRECTION ( 'NONE',  ( 0.01997839162482749689, 1.040247600000945640E-18, -0.9998004120163610509 ) ) ;
#18945 = CARTESIAN_POINT ( 'NONE',  ( 0.8068095026010809745, 106.0274289318137306, -5.250488437364327687 ) ) ;
#18946 = CARTESIAN_POINT ( 'NONE',  ( -12.21508602987361058, 126.0625018263836807, -1.612267168929819361 ) ) ;
#18947 = LINE ( 'NONE', #6189, #40514 ) ;
#18948 = FACE_OUTER_BOUND ( 'NONE', #22826, .T. ) ;
#18949 = CARTESIAN_POINT ( 'NONE',  ( -3.613484950294342024, 115.7029504968768521, 1.483737492548300674 ) ) ;
#18950 = CARTESIAN_POINT ( 'NONE',  ( 3.728136974946417492, 6.765255174955887796, 2.739693761753763113 ) ) ;
#18952 = VERTEX_POINT ( 'NONE', #32989 ) ;
#18951 = CARTESIAN_POINT ( 'NONE',  ( 19.93082032328723940, 128.8226523212408949, 1.025501306202716956 ) ) ;
#18953 = CARTESIAN_POINT ( 'NONE',  ( 3.161028851456020750, 105.1241932395464147, -4.308685071247855269 ) ) ;
#18954 = CARTESIAN_POINT ( 'NONE',  ( 1.842426711869078471, -15.45708672024491470, 5.391926158250404555 ) ) ;
#18955 = CARTESIAN_POINT ( 'NONE',  ( -7.655434399952044444, 119.7866739149480253, 1.082013720931114920 ) ) ;
#18956 = CARTESIAN_POINT ( 'NONE',  ( -0.3594991891230457370, 15.46976683256975704, -0.9053751552070300468 ) ) ;
#18957 = CARTESIAN_POINT ( 'NONE',  ( 0.6269268744496204748, 0.2942410971610713855, -0.7472855871245592807 ) ) ;
#18958 = ORIENTED_EDGE ( 'NONE', *, *, #16719, .T. ) ;
#18959 = ORIENTED_EDGE ( 'NONE', *, *, #21198, .T. ) ;
#18960 = CARTESIAN_POINT ( 'NONE',  ( -4.882471689226330902, 117.7035670401112952, -0.9281964497351922194 ) ) ;
#18961 = CARTESIAN_POINT ( 'NONE',  ( 5.124638537096516622, 121.7269124416356192, 0.3048162158978749425 ) ) ;
#18962 =( LENGTH_UNIT ( ) NAMED_UNIT ( * ) SI_UNIT ( .MILLI., .METRE. ) );
#18963 = CARTESIAN_POINT ( 'NONE',  ( -8.403980202277468337, 154.6912814427390970, 0.9387012965349954552 ) ) ;
#18964 = CARTESIAN_POINT ( 'NONE',  ( -9.118174893680297544, 124.1671967267183589, -0.1822028344259498389 ) ) ;
#18965 = CARTESIAN_POINT ( 'NONE',  ( 3.041920762657289057, -14.42862556718194078, 4.364129476586208867 ) ) ;
#18966 = CARTESIAN_POINT ( 'NONE',  ( 10.93624696698907961, 154.4230204216147513, -1.584134132468239198 ) ) ;
#18967 = CARTESIAN_POINT ( 'NONE',  ( -12.33952200554344536, 155.1253022143813496, -2.231822996700852269 ) ) ;
#18968 = DIRECTION ( 'NONE',  ( -0.000000000000000000, -0.000000000000000000, -1.000000000000000000 ) ) ;
#18969 = CARTESIAN_POINT ( 'NONE',  ( 8.798071512540863282, 117.6842349196870572, 0.1758064070670784795 ) ) ;
#18970 = CARTESIAN_POINT ( 'NONE',  ( 4.120272809047287765, 118.2429491485453354, -0.1840329633741082382 ) ) ;
#18971 = CARTESIAN_POINT ( 'NONE',  ( 11.92666644034612489, 151.9662372315928280, -0.1848526535252735803 ) ) ;
#18972 = ORIENTED_EDGE ( 'NONE', *, *, #29947, .T. ) ;
#18973 = CARTESIAN_POINT ( 'NONE',  ( -2.864724612585762387, 107.5205933461715517, -4.491126036370093111 ) ) ;
#18974 = CARTESIAN_POINT ( 'NONE',  ( -24.24876516830975248, 76.58816925568820011, 1.269999999999993801 ) ) ;
#18975 = VECTOR ( 'NONE', #3354, 1000.000000000000000 ) ;
#18976 = CIRCLE ( 'NONE', #33259, 2.540000000000000480 ) ;
#18977 = FACE_OUTER_BOUND ( 'NONE', #8080, .T. ) ;
#18978 = B_SPLINE_CURVE_WITH_KNOTS ( 'NONE', 3,
 ( #32778, #9767, #628, #35555 ),
 .UNSPECIFIED., .F., .F.,
 ( 4, 4 ),
 ( 0.000000000000000000, 0.0004289155515219138953 ),
 .UNSPECIFIED. ) ;
#18979 = CARTESIAN_POINT ( 'NONE',  ( 4.997973268168866667, 117.5914567208410091, -0.6225120149425793503 ) ) ;
#18980 = CARTESIAN_POINT ( 'NONE',  ( 1.217031898716552707, 25.17763362506526192, -8.368877290174015826 ) ) ;
#18981 = CARTESIAN_POINT ( 'NONE',  ( 14.47722597845726433, 150.4300676932417389, 1.698653275673423835 ) ) ;
#18982 = DIRECTION ( 'NONE',  ( -4.017660918040594346E-17, 1.000000000000000000, 2.376309959284834438E-19 ) ) ;
#18983 = CARTESIAN_POINT ( 'NONE',  ( 15.93439728059123794, 121.0320206851898206, 0.2674320648195326333 ) ) ;
#18984 = CARTESIAN_POINT ( 'NONE',  ( -5.239677827970801616, 116.1170857923940787, 1.027392938984838633 ) ) ;
#18985 = CARTESIAN_POINT ( 'NONE',  ( 0.4343283552818534288, -9.202337043772711667, -4.603842121470758997 ) ) ;
#18986 = DIRECTION ( 'NONE',  ( 0.1906721105965039909, -0.9816537812491094028, 2.657572025465702696E-16 ) ) ;
#18987 = CARTESIAN_POINT ( 'NONE',  ( 4.023942337083048493, 118.1249481555716301, 0.9214969356372304521 ) ) ;
#18988 = CARTESIAN_POINT ( 'NONE',  ( -7.610815090270081740, 30.95102479468643963, -3.615626113024899002 ) ) ;
#18989 = CARTESIAN_POINT ( 'NONE',  ( -5.481196946644558921, 117.2620904849268868, -0.8344542377508360476 ) ) ;
#18990 = CARTESIAN_POINT ( 'NONE',  ( -0.03413713131426455299, 107.6766875080336376, -4.617405654744151988 ) ) ;
#18991 = CARTESIAN_POINT ( 'NONE',  ( 5.586884702347363785, 110.9644662015457328, 0.1116392523995368424 ) ) ;
#18992 = CARTESIAN_POINT ( 'NONE',  ( 0.1058213901577000071, 105.9761915687834772, -5.295735085524063024 ) ) ;
#18993 = CARTESIAN_POINT ( 'NONE',  ( -0.9950013725589796909, 29.65466048987409309, -4.513790593961638287 ) ) ;
#18994 = CARTESIAN_POINT ( 'NONE',  ( 3.354524074468420380, 117.9394488116011814, 1.288362988575229240 ) ) ;
#18995 = DIRECTION ( 'NONE',  ( -5.206863593109713661E-17, 1.000000000000000000, -1.077750396879097183E-30 ) ) ;
#18996 = CARTESIAN_POINT ( 'NONE',  ( 2.666490510518176649, -13.49855353256042889, 0.05227394649444832425 ) ) ;
#18997 = CARTESIAN_POINT ( 'NONE',  ( 0.3848090724907686777, 122.5569158606515003, -0.2475921850528963741 ) ) ;
#18998 = CARTESIAN_POINT ( 'NONE',  ( -20.43054131464321443, 152.5480347002736607, 0.4178791510274247334 ) ) ;
#18999 = VERTEX_POINT ( 'NONE', #32135 ) ;
#19000 = CARTESIAN_POINT ( 'NONE',  ( -14.38915334913366983, 80.27078028363496287, 1.269999999999998019 ) ) ;
#19001 = AXIS2_PLACEMENT_3D ( 'NONE', #34018, #4431, #1646 ) ;
#19002 = ORIENTED_EDGE ( 'NONE', *, *, #25311, .F. ) ;
#19003 = DIRECTION ( 'NONE',  ( 0.9998004120163608288, 0.000000000000000000, 0.01997839162482736852 ) ) ;
#19004 = CARTESIAN_POINT ( 'NONE',  ( 4.596189786833723367, -15.64549520875656263, 3.377287787771500849 ) ) ;
#19005 = CARTESIAN_POINT ( 'NONE',  ( -4.992797058275008304, 118.5534682650580862, 0.8674252695128578106 ) ) ;
#19006 = CARTESIAN_POINT ( 'NONE',  ( 1.320630737124448117, 159.3505072347868747, -0.9467419726141094172 ) ) ;
#19007 = CARTESIAN_POINT ( 'NONE',  ( -3.426874451426485724, 1.805113900313119357, -3.130497002818263930 ) ) ;
#19008 = CARTESIAN_POINT ( 'NONE',  ( -56.05195996919411527, 5.170694913744002363, -2.763834368020857468 ) ) ;
#19009 = ORIENTED_EDGE ( 'NONE', *, *, #14409, .F. ) ;
#19010 = CARTESIAN_POINT ( 'NONE',  ( -58.01460528358209956, 0.4727233027800176179, -0.8404818439587155021 ) ) ;
#19011 = CARTESIAN_POINT ( 'NONE',  ( -0.01635612298167265014, 119.2343925067225427, 0.8185272769043292485 ) ) ;
#19012 = DIRECTION ( 'NONE',  ( -0.9998004120163609398, 0.000000000000000000, -0.01997839162482749689 ) ) ;
#19013 = CARTESIAN_POINT ( 'NONE',  ( -15.09269357795387911, 134.7883251604851580, 1.349233830697068148 ) ) ;
#19014 = CARTESIAN_POINT ( 'NONE',  ( 5.143063430802804703, 116.8705556046722620, 0.2506579733502571350 ) ) ;
#19015 = CARTESIAN_POINT ( 'NONE',  ( 9.673022701212177665, 121.1143850344477215, -1.180881524473704758 ) ) ;
#19016 = CARTESIAN_POINT ( 'NONE',  ( -2.782193507150807932, 158.7847427699215928, -1.504205172470084673 ) ) ;
#19017 = CARTESIAN_POINT ( 'NONE',  ( -49.01671973967521012, 18.67808020721676954, -5.174630477995056488 ) ) ;
#19018 = CARTESIAN_POINT ( 'NONE',  ( 0.004916276843073956807, 120.6356583033945782, -0.2460305967400716332 ) ) ;
#19019 = VERTEX_POINT ( 'NONE', #26367 ) ;
#19020 = CARTESIAN_POINT ( 'NONE',  ( 0.02969003158472036108, 157.1787724364823760, -1.485810588193620552 ) ) ;
#19021 = CARTESIAN_POINT ( 'NONE',  ( 3.745939827176673731, -15.15858284179406823, -0.4807645327530354340 ) ) ;
#19022 = CARTESIAN_POINT ( 'NONE',  ( -4.147540096004632915, 118.2392522295950670, -0.3974202085649201077 ) ) ;
#19023 = CARTESIAN_POINT ( 'NONE',  ( -55.14069116334859189, 5.401725095812784261, -9.794129604158680367E-15 ) ) ;
#19024 = EDGE_CURVE ( 'NONE', #24258, #31942, #29135, .T. ) ;
#19025 = AXIS2_PLACEMENT_3D ( 'NONE', #5597, #31558, #41373 ) ;
#19026 = CARTESIAN_POINT ( 'NONE',  ( -4.765692302950382597, 117.6625622553268471, 0.9423543906840938789 ) ) ;
#19027 = CARTESIAN_POINT ( 'NONE',  ( 17.92612601409326345, 146.8415343102147972, 2.296925525151568781 ) ) ;
#19028 = CYLINDRICAL_SURFACE ( 'NONE', #23982, 9.048749999999998295 ) ;
#19029 = EDGE_CURVE ( 'NONE', #18166, #15388, #18439, .T. ) ;
#19030 = CARTESIAN_POINT ( 'NONE',  ( -0.1328416520900886078, 24.48205809745167372, 4.627450821846854190 ) ) ;
#19031 = CARTESIAN_POINT ( 'NONE',  ( 11.90976107009709395, 151.9662372315928280, 0.6611612027286484228 ) ) ;
#19032 = CARTESIAN_POINT ( 'NONE',  ( -30.28638171898572651, 70.19821000523995735, -1.524000000000007571 ) ) ;
#19034 = VERTEX_POINT ( 'NONE', #29783 ) ;
#19033 = CARTESIAN_POINT ( 'NONE',  ( -47.11704014324647005, 20.18577099567724886, -5.127035723291441194 ) ) ;
#19035 = CARTESIAN_POINT ( 'NONE',  ( -0.02983097934279877947, 117.3993836135855418, 1.492864285909964561 ) ) ;
#19036 = CARTESIAN_POINT ( 'NONE',  ( -8.313969523394650452, 67.96940778435646280, 1.524000000000002908 ) ) ;
#19037 = CARTESIAN_POINT ( 'NONE',  ( -51.06915940311598234, 14.53650747930048581, 4.673419795157606416 ) ) ;
#19038 = CARTESIAN_POINT ( 'NONE',  ( -8.504453550875423318, 119.0083879741271602, -1.280283385220987835 ) ) ;
#19039 = LINE ( 'NONE', #28431, #21484 ) ;
#19040 = CARTESIAN_POINT ( 'NONE',  ( -54.80060171144386771, 10.20856468236482684, 2.175828276708562825 ) ) ;
#19041 = EDGE_CURVE ( 'NONE', #38830, #17268, #40938, .T. ) ;
#19042 = CARTESIAN_POINT ( 'NONE',  ( -23.07880092997899979, 149.8841935741895384, -0.1310273949726223075 ) ) ;
#19043 = EDGE_LOOP ( 'NONE', ( #34089, #34401, #9856, #39993 ) ) ;
#19044 = CARTESIAN_POINT ( 'NONE',  ( -52.80069327121181288, 17.37962920081948681, -0.7126778406583914593 ) ) ;
#19045 = CARTESIAN_POINT ( 'NONE',  ( -7.831385197639477269, 122.3498825523410716, -0.6732435565748877693 ) ) ;
#19046 = CARTESIAN_POINT ( 'NONE',  ( 4.828460766595028097, 117.4062652275384693, -1.009527310354734642 ) ) ;
#19047 = ORIENTED_EDGE ( 'NONE', *, *, #21855, .F. ) ;
#19048 = CARTESIAN_POINT ( 'NONE',  ( 0.7744055587462789214, 115.7029695782703982, -1.727565141520491121 ) ) ;
#19049 = CARTESIAN_POINT ( 'NONE',  ( -3.737471135337945949, 121.0798372856833538, -0.1416028149587413298 ) ) ;
#19050 = CARTESIAN_POINT ( 'NONE',  ( 5.906500239725072987, -12.19293670846725774, 0.5532178544325924152 ) ) ;
#19051 = CARTESIAN_POINT ( 'NONE',  ( -9.669117252159470155, 157.4977751962898083, 1.392273965589622575 ) ) ;
#19052 = CARTESIAN_POINT ( 'NONE',  ( 4.880629475852391153, 56.51998046905271877, -4.886937129244065758 ) ) ;
#19053 = CARTESIAN_POINT ( 'NONE',  ( 13.39999158873808405, 156.9487217736090940, 0.4592210153261411798 ) ) ;
#19054 = CARTESIAN_POINT ( 'NONE',  ( 8.677412068956916968, 123.6667082555040480, 0.3039716813630899406 ) ) ;
#19055 = CARTESIAN_POINT ( 'NONE',  ( 4.825602063014114762, 118.5266822147775940, -0.7769288410131838241 ) ) ;
#19056 = CARTESIAN_POINT ( 'NONE',  ( 0.3789452347801735566, 6.767153838948093636, 0.8990310622920915096 ) ) ;
#19057 = CARTESIAN_POINT ( 'NONE',  ( -16.84361796505737630, 155.2300590059875844, -0.4756075834919731293 ) ) ;
#19058 = DIRECTION ( 'NONE',  ( -1.000000000000000000, 0.000000000000000000, 0.000000000000000000 ) ) ;
#19059 = DIRECTION ( 'NONE',  ( -0.7071067811865480168, -0.7071067811865470176, 8.659560562354937789E-17 ) ) ;
#19060 = VERTEX_POINT ( 'NONE', #6781 ) ;
#19061 = CARTESIAN_POINT ( 'NONE',  ( -5.622202078731264763, 117.6368178314116477, 0.7310929967662477269 ) ) ;
#19063 = EDGE_CURVE ( 'NONE', #24401, #21265, #34130, .T. ) ;
#19062 = ORIENTED_EDGE ( 'NONE', *, *, #1463, .F. ) ;
#19064 = CARTESIAN_POINT ( 'NONE',  ( -58.31778746384443224, -0.1819811653371645743, -0.2882286546613240796 ) ) ;
#19065 = CARTESIAN_POINT ( 'NONE',  ( 5.008743879648425157, 158.5910778905036977, 1.550406713891092414 ) ) ;
#19066 = CARTESIAN_POINT ( 'NONE',  ( 19.92238394974707205, 148.9191654756151024, -1.700261758071553775 ) ) ;
#19067 = CARTESIAN_POINT ( 'NONE',  ( -2.798479926918381544, 16.31753791307728818, -7.953355231451358698 ) ) ;
#19068 = CARTESIAN_POINT ( 'NONE',  ( -6.844670616442416922, 117.9658002137636856, -0.9618333202595320541 ) ) ;
#19069 = CARTESIAN_POINT ( 'NONE',  ( 4.745547297112636898, 117.9479177059493082, -0.6406879345116325286 ) ) ;
#19070 = CARTESIAN_POINT ( 'NONE',  ( 11.74288454345096788, 118.7273140689154616, 0.2346507796901761422 ) ) ;
#19071 = EDGE_CURVE ( 'NONE', #37655, #2940, #35549, .T. ) ;
#19072 = CARTESIAN_POINT ( 'NONE',  ( -7.047330174099129430, 122.0696255612902519, -0.06645725506650262959 ) ) ;
#19073 = CARTESIAN_POINT ( 'NONE',  ( -19.20800265940886931, 147.1635184732690220, -2.509201515169785957 ) ) ;
#19074 = ADVANCED_FACE ( 'NONE', ( #28927 ), #9347, .T. ) ;
#19075 = CARTESIAN_POINT ( 'NONE',  ( 2.394017677299879576, -15.71294128685811486, 5.613897423981592638 ) ) ;
#19076 = SHAPE_REPRESENTATION ( 'Center Spindle', ( #3275 ), #21588 ) ;
#19077 = DIRECTION ( 'NONE',  ( -5.206863593109713661E-17, 1.000000000000000000, -1.077750396879097183E-30 ) ) ;
#19078 = CONICAL_SURFACE ( 'NONE', #14298, 13.46199999999999619, 0.7853981633974482790 ) ;
#19079 = ADVANCED_FACE ( 'NONE', ( #26159 ), #15727, .F. ) ;
#19080 = CARTESIAN_POINT ( 'NONE',  ( -42.34481381083929818, 23.19759442052183473, -1.554397948409621755 ) ) ;
#19081 = EDGE_LOOP ( 'NONE', ( #35520, #28213, #37680, #25724, #27923 ) ) ;
#19082 = B_SPLINE_SURFACE_WITH_KNOTS ( 'NONE', 3, 3, ( 
 ( #31810, #41409, #25422, #28404, #22610, #13044, #3268, #19222, #12216, #38423, #2438, #25620, #22818, #15606, #32233, #5844, #3064, #41837, #38630, #9643, #22195, #19011, #16227, #9433, #35426, #28611, #6253, #39043, #41620, #6457, #38210, #42040, #22402, #35224 ),
 ( #6049, #12632, #9850, #76, #26034, #32015, #21992, #16021, #35856, #6669, #31601, #15401, #35023, #2854, #15815, #29022, #12836, #25824, #38832, #29449, #503, #16443, #10689, #1123, #20472, #7302, #288, #13475, #32647, #13682, #10897, #6877, #20261, #36063 ),
 ( #23669, #23242, #23032, #13891, #33288, #36276, #19849, #26463, #16655, #17294, #7511, #20058, #4329, #30283, #39255, #36688, #29872, #33499, #14094, #32863, #29662, #39467, #3909, #27093, #3694, #40101, #10062, #3483, #10270, #23886, #7097, #19632, #4118, #33077 ),
 ( #36904, #36481, #39892, #16871, #13261, #26245, #711, #26674, #26883, #39682, #10484, #17078, #23454, #30079, #917, #40932, #18120, #14293, #11316, #11740, #24942, #24727, #11951, #30698, #37730, #21513, #41145, #7722, #21307, #30915, #17496, #37514, #14502, #31125 ),
 ( #5373, #8554, #24304, #34337, #15133, #20687, #27303, #1548, #40318, #27517, #1961, #11111, #17698, #14922, #33712, #24100, #33917, #40525, #37310, #21101, #18328, #5165, #27926, #34548, #8339, #31330, #30493, #2175, #17911, #28137, #4533, #1335, #37108, #7927 ),
 ( #20895, #4746, #8126, #34125, #4952, #1754, #14713, #27717, #40726, #11523, #24507, #41361, #34970, #25774, #38371, #9386, #9186, #41987, #15971, #22142, #22562, #35173, #3013, #28969, #41572, #12164, #32180, #22350, #12381, #25158, #18749, #5792, #35592, #38782 ),
 ( #5582, #6203, #28771, #38159, #19174, #16177, #31758, #18961, #29180, #6409, #9592, #8974, #31543, #31968, #19379, #32384, #3215, #27, #12785, #2389, #18540, #41782, #12991, #37941, #12581, #8766, #2600, #21726, #34750, #15347, #5999, #28352, #21941, #15560 ),
 ( #35374, #28563, #2806, #25367, #25570, #15767, #38575, #39202, #13423, #10642, #33028, #10011, #7044, #7255, #16608, #17029, #22983, #26621, #35803, #36010, #20215, #6824, #39630, #23622, #30028, #29616, #10435, #33450, #17241, #3428, #19793, #32594, #32813, #36436 ),
 ( #13631, #30236, #20011, #36642, #452, #26411, #38994, #16822, #39846, #39416, #10218, #1075, #9803, #4279, #20423, #3644, #13841, #23188, #36223, #13215, #16393, #662, #29399, #26197, #4070, #33241, #3857, #23406, #868, #6616, #25986, #29824, #7464, #22770 ),
 ( #19584, #26839, #238, #41041, #11851, #18222, #20633, #28032, #35080, #36856, #21620, #40056, #17446, #11634, #2497, #15032, #28248, #24837, #18652, #34861, #37832, #41467, #8659, #21833, #5693, #31223, #30445, #8870, #41252, #2067, #1289, #37627, #24619, #12275 ),
 ( #31658, #23835, #25047, #5474, #14247, #38051, #5901, #8451, #34646, #18862, #25265, #15460, #27254, #7674, #18434, #28461, #38268, #9085, #22051, #31866, #33661, #4486, #31441, #14044, #27048, #2284, #10849, #21409, #40270, #34436, #5271, #15247, #12058, #25482 ),
 ( #29516, #38477, #9296, #35920, #13109, #22257, #6311, #6730, #19914, #19697, #6946, #25683, #32716, #16509, #36129, #2706, #16296, #25887, #12487, #32500, #9495, #26101, #42105, #39107, #41894, #19491, #19284, #41679, #35706, #6516, #32291, #3120, #28669, #9911 ) ),
 .UNSPECIFIED., .F., .F., .F.,
 ( 4, 1, 1, 1, 1, 1, 3, 4 ),
 ( 4, 1, 1, 1, 1, 1, 1, 1, 1, 1, 1, 1, 1, 1, 1, 1, 1, 1, 1, 2, 1, 1, 1, 1, 1, 1, 1, 1, 1, 1, 4 ),
 ( 0.000000000000000000, 0.1666666666666666574, 0.2500000000000000000, 0.5000000000000000000, 0.5555555555555555802, 0.7500000000000000000, 1.000000000000000000, 1.010000000000000009 ),
 ( 0.000000000000000000, 0.02126250000000000015, 0.04252500000000000030, 0.06378749999999999698, 0.08505000000000000060, 0.1063125000000000042, 0.1275749999999999940, 0.1488374999999999837, 0.1701000000000000012, 0.1913624999999999909, 0.2126250000000000084, 0.2338874999999999704, 0.2551500000000000434, 0.2764124999999999499, 0.2870437499999999864, 0.2976749999999999674, 0.3083062500000000039, 0.3189375000000000404, 0.3295687499999999659, 0.3402000000000000024, 0.4226750000000000229, 0.5051499999999999879, 0.5876249999999998419, 0.6700999999999999179, 0.7525749999999999940, 0.7938125000000000320, 0.8350499999999999590, 0.8762874999999994419, 0.9175249999999994799, 0.9587624999999999620, 1.000000000000000000 ),
 .UNSPECIFIED. ) ;
#19083 = CARTESIAN_POINT ( 'NONE',  ( 10.15136974315531049, 155.5514087735115822, 2.139549497352468244 ) ) ;
#19084 = CARTESIAN_POINT ( 'NONE',  ( -5.177913976931287188, 56.99702125087951288, 5.372100000000003206 ) ) ;
#19085 = CIRCLE ( 'NONE', #6180, 0.2539999999999997260 ) ;
#19086 = DIRECTION ( 'NONE',  ( 0.7517731442105912709, -0.6594218222380281436, 8.537024980200781389E-16 ) ) ;
#19087 = CARTESIAN_POINT ( 'NONE',  ( -2.121281617407082987, 114.8832439220486350, 1.889083087725355048 ) ) ;
#19088 = CARTESIAN_POINT ( 'NONE',  ( -7.610815090270081740, 30.95102479468643963, -3.615626113024899002 ) ) ;
#19089 = CARTESIAN_POINT ( 'NONE',  ( 15.52857178871868093, 148.0963874134046705, 1.155438959258077380 ) ) ;
#19090 = CARTESIAN_POINT ( 'NONE',  ( 17.93297959639523143, 125.1504969321615164, -0.5028613125471299572 ) ) ;
#19091 = CARTESIAN_POINT ( 'NONE',  ( -4.345705637489792217, 70.43763872253876457, -1.523999999999994026 ) ) ;
#19092 = CARTESIAN_POINT ( 'NONE',  ( -17.08598887363762131, 83.79821757228496892, -1.524000000000002908 ) ) ;
#19093 = CARTESIAN_POINT ( 'NONE',  ( -22.98549031890228989, 150.1594536303649932, -0.4336790679505425072 ) ) ;
#19094 = ORIENTED_EDGE ( 'NONE', *, *, #27961, .F. ) ;
#19095 = CARTESIAN_POINT ( 'NONE',  ( -6.324598044711755129, 120.0162699490936120, -1.207732045962844669 ) ) ;
#19096 = DIRECTION ( 'NONE',  ( -0.8745520943968251304, 0.4849315768086532863, -5.424246918827961050E-16 ) ) ;
#19097 = CARTESIAN_POINT ( 'NONE',  ( -6.479751845157381673, 121.6679077367135591, -0.4493306481243477535 ) ) ;
#19098 = CARTESIAN_POINT ( 'NONE',  ( -30.59449053042481736, 55.40488188693900895, 1.523999999999993582 ) ) ;
#19099 = CIRCLE ( 'NONE', #3475, 0.5080000000000002292 ) ;
#19100 = CARTESIAN_POINT ( 'NONE',  ( 15.19604463793433169, 156.0859089222169587, 0.3036531364422415669 ) ) ;
#19101 = EDGE_LOOP ( 'NONE', ( #10686, #36520, #26672, #1225 ) ) ;
#19102 = CARTESIAN_POINT ( 'NONE',  ( -3.234384296441582762, 11.31316835407710819, -3.315160845070126427 ) ) ;
#19103 = CARTESIAN_POINT ( 'NONE',  ( -29.20589784622301011, 64.40785669711239336, 1.523999999999849253 ) ) ;
#19104 = CARTESIAN_POINT ( 'NONE',  ( -4.976922239355512367, 117.4076159968771833, 0.8840036975013897402 ) ) ;
#19105 = CARTESIAN_POINT ( 'NONE',  ( 0.9670297670242945509, 105.9617104547169788, 5.250135314356312755 ) ) ;
#19106 = ADVANCED_FACE ( 'NONE', ( #16350 ), #22727, .T. ) ;
#19107 = DIRECTION ( 'NONE',  ( -5.188838149069471174E-16, 1.699382548006136313E-16, 1.000000000000000000 ) ) ;
#19108 = CARTESIAN_POINT ( 'NONE',  ( -7.959258266637833756, 121.8607301277289565, 0.7063002939533309377 ) ) ;
#19109 = CARTESIAN_POINT ( 'NONE',  ( 4.309711357183296343, 3.151582320728117725, 1.677628897243969464 ) ) ;
#19110 = EDGE_CURVE ( 'NONE', #296, #19469, #21165, .T. ) ;
#19111 = CARTESIAN_POINT ( 'NONE',  ( 22.50377699857059000, 149.0203452686010337, 1.755643737887156997 ) ) ;
#19112 = DIRECTION ( 'NONE',  ( -0.9998004120163609398, -4.016384292689130894E-17, -0.01997839162482749689 ) ) ;
#19114 = CARTESIAN_POINT ( 'NONE',  ( 2.188165212810265103, 117.9909145081919917, -0.6446704472730118152 ) ) ;
#19113 = LINE ( 'NONE', #35743, #4595 ) ;
#19115 = VECTOR ( 'NONE', #16622, 1000.000000000000000 ) ;
#19116 = CARTESIAN_POINT ( 'NONE',  ( 4.428293322310913993, 12.87204911218450576, 1.319288874004734158 ) ) ;
#19117 = CARTESIAN_POINT ( 'NONE',  ( -15.29070941918909199, 121.1074504348956964, -0.9956366180447245862 ) ) ;
#19118 = EDGE_LOOP ( 'NONE', ( #39349, #3062, #22674, #4845, #9751, #19145, #33371, #30913 ) ) ;
#19119 = CARTESIAN_POINT ( 'NONE',  ( -15.52187087609533478, 147.8629129908177049, 0.2796426011346636042 ) ) ;
#19120 = ADVANCED_FACE ( 'NONE', ( #12949 ), #38949, .T. ) ;
#19121 = CARTESIAN_POINT ( 'NONE',  ( 4.196136289373067818, -14.93657984310306475, 5.004071965215434403 ) ) ;
#19122 = CARTESIAN_POINT ( 'NONE',  ( -23.91048590848665611, 81.84235438443283783, -1.270000000000006235 ) ) ;
#19123 = EDGE_CURVE ( 'NONE', #19747, #5873, #4655, .T. ) ;
#19124 = CARTESIAN_POINT ( 'NONE',  ( -4.604761013128439551, 118.0233142930135557, -0.8446000906974990841 ) ) ;
#19125 = CARTESIAN_POINT ( 'NONE',  ( 1.617373050801646839, 120.9968702744464366, 0.03231896268895514263 ) ) ;
#19126 = EDGE_LOOP ( 'NONE', ( #22993, #31122, #24416, #13839 ) ) ;
#19127 = CARTESIAN_POINT ( 'NONE',  ( 19.78444808418223033, 147.9128418260961837, 2.517891032746079283 ) ) ;
#19128 = DIRECTION ( 'NONE',  ( -0.000000000000000000, 0.000000000000000000, -1.000000000000000000 ) ) ;
#19129 = CARTESIAN_POINT ( 'NONE',  ( 10.18105065676961729, 125.9743313966586129, 0.2034416216762106322 ) ) ;
#19130 = EDGE_CURVE ( 'NONE', #26452, #19060, #32758, .T. ) ;
#19131 = AXIS2_PLACEMENT_3D ( 'NONE', #31545, #8128, #21103 ) ;
#19132 = CARTESIAN_POINT ( 'NONE',  ( -15.10519797802286845, 121.1899582252741112, 0.5359826722732081716 ) ) ;
#19133 = B_SPLINE_CURVE_WITH_KNOTS ( 'NONE', 3,
 ( #31003, #28020, #11838, #8021 ),
 .UNSPECIFIED., .F., .F.,
 ( 4, 4 ),
 ( 0.000000000000000000, 1.000000000000000000 ),
 .UNSPECIFIED. ) ;
#19134 = CARTESIAN_POINT ( 'NONE',  ( 4.853781638280933564, 117.4081357529187528, -0.9972794204146671060 ) ) ;
#19135 = CARTESIAN_POINT ( 'NONE',  ( 22.92015980622311844, 150.1344166263168347, 0.006220127847215254323 ) ) ;
#19136 = CARTESIAN_POINT ( 'NONE',  ( -14.24929227862422820, 61.25037559889041461, 5.016500000000000625 ) ) ;
#19137 = VECTOR ( 'NONE', #7631, 1000.000000000000114 ) ;
#19138 = CARTESIAN_POINT ( 'NONE',  ( -52.51450000281151631, 11.69565325325087102, 4.043231167555472183 ) ) ;
#19139 = CARTESIAN_POINT ( 'NONE',  ( -46.94769949131580233, 25.36820868695422604, 1.370102228390891685 ) ) ;
#19140 = CARTESIAN_POINT ( 'NONE',  ( -41.05189575270519242, 23.09451173561980042, 1.269999999999989582 ) ) ;
#19141 = CARTESIAN_POINT ( 'NONE',  ( -46.31144060707497090, 24.05480373873685451, 2.308638262703916588 ) ) ;
#19142 = DIRECTION ( 'NONE',  ( 5.188838149069472160E-16, -1.699382548006136559E-16, -1.000000000000000000 ) ) ;
#19143 = CARTESIAN_POINT ( 'NONE',  ( -4.606047465314773603, 118.0409777277905334, 0.6500082233937537479 ) ) ;
#19144 = ORIENTED_EDGE ( 'NONE', *, *, #34150, .T. ) ;
#19145 = ORIENTED_EDGE ( 'NONE', *, *, #23354, .T. ) ;
#19146 = CARTESIAN_POINT ( 'NONE',  ( -5.177913976931295181, 71.67999986514566046, 5.372100000000000541 ) ) ;
#19147 = CARTESIAN_POINT ( 'NONE',  ( 5.979754242620736626, 119.1689217970666732, -1.027035715780954428 ) ) ;
#19148 = CARTESIAN_POINT ( 'NONE',  ( -1.370820134808223623, 106.2483430537416638, -5.168860673143087503 ) ) ;
#19149 = CARTESIAN_POINT ( 'NONE',  ( 4.710630312300388312, 117.8980792669073310, 0.9560384519295030969 ) ) ;
#19150 = AXIS2_PLACEMENT_3D ( 'NONE', #17109, #18149, #41603 ) ;
#19151 = CARTESIAN_POINT ( 'NONE',  ( 2.671714809844681238, -14.97371442308345380, 4.574436322856921144 ) ) ;
#19152 = CARTESIAN_POINT ( 'NONE',  ( -9.472608709197698929, 123.5188755717998816, -0.9573233835003830405 ) ) ;
#19153 = CARTESIAN_POINT ( 'NONE',  ( -3.782657323308230790, 115.7032134869121052, -1.604837383391216177 ) ) ;
#19154 = CARTESIAN_POINT ( 'NONE',  ( -2.307087371449152435, 107.0582400219110468, 4.722921399226381212 ) ) ;
#19155 = DIRECTION ( 'NONE',  ( 0.1715592850456333363, 0.1224830539174543431, -0.9775302108976914317 ) ) ;
#19156 = CARTESIAN_POINT ( 'NONE',  ( 6.697645968159008589, 121.2318545172250737, -0.07433936815196268144 ) ) ;
#19157 = CARTESIAN_POINT ( 'NONE',  ( 0.008945177887895646232, 119.9096241394016715, -0.4476532798976758376 ) ) ;
#19158 = FILL_AREA_STYLE ('',( #2792 ) ) ;
#19159 = CARTESIAN_POINT ( 'NONE',  ( 0.4584169952490399491, 38.71425902074634706, 1.375259010134687765 ) ) ;
#19160 = CARTESIAN_POINT ( 'NONE',  ( -3.014526234809750793, 115.7029722856716631, 1.552890539658475566 ) ) ;
#19161 = CARTESIAN_POINT ( 'NONE',  ( 2.862861873098513144, -10.07698056833738143, -3.640125809621839625 ) ) ;
#19163 = ORIENTED_EDGE ( 'NONE', *, *, #33484, .F. ) ;
#19162 = CARTESIAN_POINT ( 'NONE',  ( 1.362313394648025699, 159.5452856091935132, 0.5382632954014164861 ) ) ;
#19164 = CARTESIAN_POINT ( 'NONE',  ( -0.7308287095922618715, 104.6144662015455964, -4.780214960664815216 ) ) ;
#19165 = CARTESIAN_POINT ( 'NONE',  ( 3.526206095277399033, -15.04645431008844270, 1.792912095860496269 ) ) ;
#19166 = CARTESIAN_POINT ( 'NONE',  ( -11.12579521122948734, 121.4866960210745503, 1.254162869557706284 ) ) ;
#19167 = AXIS2_PLACEMENT_3D ( 'NONE', #11920, #8943, #5764 ) ;
#19168 = CARTESIAN_POINT ( 'NONE',  ( -0.9635192623308774795, 7.475506455475952272, -0.1398073520734665620 ) ) ;
#19169 = TOROIDAL_SURFACE ( 'NONE', #6944, 0.3809999999999999498, 0.2540000000000000036 ) ;
#19170 = CARTESIAN_POINT ( 'NONE',  ( 0.9727671068909850005, -1.206248505109467795, 0.1081409728948927729 ) ) ;
#19171 = ORIENTED_EDGE ( 'NONE', *, *, #9933, .F. ) ;
#19172 = ORIENTED_EDGE ( 'NONE', *, *, #2814, .F. ) ;
#19173 = CARTESIAN_POINT ( 'NONE',  ( -41.05189575270522795, 23.09451173561975779, 1.171222222222216613 ) ) ;
#19174 = CARTESIAN_POINT ( 'NONE',  ( 5.572611807913179227, 123.3023672762779910, 0.1864456790743030112 ) ) ;
#19175 = DIRECTION ( 'NONE',  ( 0.000000000000000000, 0.000000000000000000, 1.000000000000000000 ) ) ;
#19176 = CARTESIAN_POINT ( 'NONE',  ( -14.98735845036259917, 139.3652335140928074, 0.8263902896301494883 ) ) ;
#19177 = CARTESIAN_POINT ( 'NONE',  ( 10.92199999999999704, 57.14999999999999858, -4.381499999999999950 ) ) ;
#19178 = CARTESIAN_POINT ( 'NONE',  ( 3.826441825042426359, -13.78667705120290066, 4.058770776067232688 ) ) ;
#19179 = CARTESIAN_POINT ( 'NONE',  ( 11.33340168069282861, 123.5700555580090594, -1.145074488444943306 ) ) ;
#19180 = CARTESIAN_POINT ( 'NONE',  ( 0.01147819631900381596, 118.5605975114896609, -0.5744158801423951966 ) ) ;
#19181 = DIRECTION ( 'NONE',  ( -0.8745520943968235761, 0.4849315768086558398, -4.268512490100410909E-16 ) ) ;
#19182 = EDGE_CURVE ( 'NONE', #27127, #25568, #38858, .T. ) ;
#19183 = CARTESIAN_POINT ( 'NONE',  ( 8.133233755128500775, 120.8101225051349701, 1.375441441843951340 ) ) ;
#19184 = CARTESIAN_POINT ( 'NONE',  ( -5.848753628616515599, 31.48281334387809238, 0.7289013152532436424 ) ) ;
#19185 = CARTESIAN_POINT ( 'NONE',  ( 0.6667004703451558933, 156.3175253132196190, -0.2457982560305634334 ) ) ;
#19186 = ORIENTED_EDGE ( 'NONE', *, *, #12125, .T. ) ;
#19187 = FACE_OUTER_BOUND ( 'NONE', #24499, .T. ) ;
#19188 = DIRECTION ( 'NONE',  ( 0.7071067811865436870, 8.659560562354886020E-17, -0.7071067811865513475 ) ) ;
#19189 = CARTESIAN_POINT ( 'NONE',  ( 6.905624999999943725, 85.80437499999999318, 0.000000000000000000 ) ) ;
#19190 = CARTESIAN_POINT ( 'NONE',  ( 9.696059495791431004, 123.7664141286412871, 0.9760873372638446677 ) ) ;
#19191 = DIRECTION ( 'NONE',  ( -0.8745520943968243532, 0.4849315768086546741, -5.271987356194192020E-16 ) ) ;
#19192 = CARTESIAN_POINT ( 'NONE',  ( 23.35954322469556033, 148.8716009884483071, 0.3896314068422420118 ) ) ;
#19193 = CARTESIAN_POINT ( 'NONE',  ( -6.697645968159137375, 121.2318545172250737, 0.07433936815196282022 ) ) ;
#19194 = CIRCLE ( 'NONE', #4274, 6.350000000000004974 ) ;
#19195 = FACE_OUTER_BOUND ( 'NONE', #35715, .T. ) ;
#19196 = CARTESIAN_POINT ( 'NONE',  ( 1.172031118611134874E-15, 12.17394877578616885, 0.000000000000000000 ) ) ;
#19197 = CARTESIAN_POINT ( 'NONE',  ( -3.999880774356848523, 33.21692059697370070, 1.336717509662867398 ) ) ;
#19198 = CARTESIAN_POINT ( 'NONE',  ( 5.843718602766560188, 118.4234969239897453, 1.100938688348692240 ) ) ;
#19199 = CARTESIAN_POINT ( 'NONE',  ( -6.116428202004375869, -11.74185255526443505, -5.788024375304219760 ) ) ;
#19200 = CARTESIAN_POINT ( 'NONE',  ( 2.183490310512786525, 116.7443332818461670, -0.4098265381987980516 ) ) ;
#19201 = CARTESIAN_POINT ( 'NONE',  ( 0.03040743767353545901, 116.4813942609868178, -1.521712522323299677 ) ) ;
#19202 = DIRECTION ( 'NONE',  ( -0.000000000000000000, -0.000000000000000000, -1.000000000000000000 ) ) ;
#19203 = CARTESIAN_POINT ( 'NONE',  ( 4.337287324166744895, 111.8944019378196515, -2.742125067219324919 ) ) ;
#19204 = CARTESIAN_POINT ( 'NONE',  ( 0.1093955723348968428, 105.1224543976622243, 5.344227820326648448 ) ) ;
#19205 = CARTESIAN_POINT ( 'NONE',  ( -4.544942180623752215, 12.81246518813932589, 0.8472608254572608910 ) ) ;
#19206 = CYLINDRICAL_SURFACE ( 'NONE', #29349, 16.60960244842765832 ) ;
#19207 = DIRECTION ( 'NONE',  ( 0.8745520943968235761, -0.4849315768086558398, 4.268512490100410909E-16 ) ) ;
#19208 = CARTESIAN_POINT ( 'NONE',  ( 3.187349844189338199, -14.38168857376666310, 3.261415970826748278 ) ) ;
#19209 = CARTESIAN_POINT ( 'NONE',  ( 2.271240278323836126, 124.1308405194309188, -0.008591128553798579870 ) ) ;
#19210 = CARTESIAN_POINT ( 'NONE',  ( -13.22272649419669932, 119.7880570645780978, 0.3832108753485274355 ) ) ;
#19211 = ORIENTED_EDGE ( 'NONE', *, *, #26871, .T. ) ;
#19212 = DIRECTION ( 'NONE',  ( -5.188838149069471174E-16, 1.699382548006136313E-16, 1.000000000000000000 ) ) ;
#19213 = ORIENTED_EDGE ( 'NONE', *, *, #16135, .F. ) ;
#19214 = CARTESIAN_POINT ( 'NONE',  ( -41.60680704300455801, 22.55277366187442212, -1.574601807768128303 ) ) ;
#19215 = CARTESIAN_POINT ( 'NONE',  ( 3.555926573287145231, -15.62149673449747489, 5.135790484437000814 ) ) ;
#19216 = CARTESIAN_POINT ( 'NONE',  ( -20.34707623724171199, 149.4216517587604756, 1.615871423115795347 ) ) ;
#19217 = CARTESIAN_POINT ( 'NONE',  ( 0.01887972822138636597, 159.3676309965788960, -0.9448188026860500077 ) ) ;
#19218 = CARTESIAN_POINT ( 'NONE',  ( 4.634220987317881679, -1.855718946426311078, -0.01876340930339078644 ) ) ;
#19219 = CARTESIAN_POINT ( 'NONE',  ( -57.50370530912426403, 2.128377494375849555, -1.812018770838218718 ) ) ;
#19220 = ORIENTED_EDGE ( 'NONE', *, *, #21380, .T. ) ;
#19221 = CARTESIAN_POINT ( 'NONE',  ( -57.16742739522069883, 2.298121588034024221, -1.685181603006209450 ) ) ;
#19222 = CARTESIAN_POINT ( 'NONE',  ( -0.003708075274190775900, 123.1683257372384901, 0.1855672496570263952 ) ) ;
#19223 = DIRECTION ( 'NONE',  ( 0.000000000000000000, 0.000000000000000000, 1.000000000000000000 ) ) ;
#19224 = CARTESIAN_POINT ( 'NONE',  ( -17.12300761254207870, 147.7912591418244403, 1.363423146152764165 ) ) ;
#19225 = DIRECTION ( 'NONE',  ( 0.9998004120163608288, 0.000000000000000000, 0.01997839162482749342 ) ) ;
#19226 = CARTESIAN_POINT ( 'NONE',  ( 2.416701088390823760, 119.2205458019918751, -0.6800916218662635959 ) ) ;
#19227 = CARTESIAN_POINT ( 'NONE',  ( -13.26090510203115969, 121.6721647909590303, -1.681263517196597723 ) ) ;
#19228 = CARTESIAN_POINT ( 'NONE',  ( -6.604684614741059612, 78.82897922428260529, 3.487443616724451356 ) ) ;
#19229 = AXIS2_PLACEMENT_3D ( 'NONE', #40915, #8536, #21496 ) ;
#19230 = ORIENTED_EDGE ( 'NONE', *, *, #14365, .F. ) ;
#19231 = CARTESIAN_POINT ( 'NONE',  ( 4.473451502231345245, 118.1283369050730130, -0.5456401070386401875 ) ) ;
#19232 = CARTESIAN_POINT ( 'NONE',  ( 14.68012063964721214, 139.2174805014774392, -0.5696158742132092501 ) ) ;
#19233 = EDGE_LOOP ( 'NONE', ( #40659, #28221, #16056, #18024, #4398, #39535, #25294, #1327 ) ) ;
#19234 = CARTESIAN_POINT ( 'NONE',  ( -0.8355136867052901373, 157.0053619834820324, -1.416332280276762834 ) ) ;
#19235 = CARTESIAN_POINT ( 'NONE',  ( 3.526206095277399033, -15.04645431008844270, 1.792912095860496269 ) ) ;
#19236 = CARTESIAN_POINT ( 'NONE',  ( -4.065972646788793554, 118.2429491485452928, -0.3080848862740693250 ) ) ;
#19237 = AXIS2_PLACEMENT_3D ( 'NONE', #5712, #25066, #15048 ) ;
#19238 = CARTESIAN_POINT ( 'NONE',  ( -56.88731995051697510, 2.378615435641926013, -1.029510524999914353E-14 ) ) ;
#19239 = VECTOR ( 'NONE', #39811, 1000.000000000000000 ) ;
#19240 = CARTESIAN_POINT ( 'NONE',  ( -4.888505472423630316, 117.6743111526193388, 0.8475594030621235175 ) ) ;
#19241 = CARTESIAN_POINT ( 'NONE',  ( 12.49704818634931414, 126.0212559692275249, 1.705261654849119068 ) ) ;
#19242 = PLANE ( 'NONE',  #15130 ) ;
#19243 = CARTESIAN_POINT ( 'NONE',  ( -4.563195415240126174, 21.88328375387019165, -0.7336086519975816289 ) ) ;
#19244 = CARTESIAN_POINT ( 'NONE',  ( 3.706155879761894756, 121.0264708767875561, 0.2234555574396433764 ) ) ;
#19245 = CARTESIAN_POINT ( 'NONE',  ( -17.31476582418722643, 62.07284264934779827, 1.269999999999998908 ) ) ;
#19246 = CARTESIAN_POINT ( 'NONE',  ( -48.77973395026506864, 17.81645205181620639, -4.684626272830477056 ) ) ;
#19247 = CARTESIAN_POINT ( 'NONE',  ( -6.573280687130626123E-14, 88.99346620154574339, 1.699031322814114629E-29 ) ) ;
#19248 = DIRECTION ( 'NONE',  ( -5.188838149069472160E-16, 1.699382548006136559E-16, 1.000000000000000000 ) ) ;
#19249 = CARTESIAN_POINT ( 'NONE',  ( -49.53393612610801711, 17.02900530345541696, 5.020798260677888258 ) ) ;
#19250 = CARTESIAN_POINT ( 'NONE',  ( -24.24369025645185260, 82.02711331519694227, 1.523999999999992916 ) ) ;
#19251 = CIRCLE ( 'NONE', #30814, 0.2540000000000038338 ) ;
#19252 = DIRECTION ( 'NONE',  ( -1.000000000000000000, -6.353134868986659519E-16, 0.000000000000000000 ) ) ;
#19253 = CARTESIAN_POINT ( 'NONE',  ( -5.871452009091403745, 88.73331249999999670, -5.016499999999999737 ) ) ;
#19254 = CARTESIAN_POINT ( 'NONE',  ( -56.22979136716762838, 7.596919248368375399, 0.4408371032392935929 ) ) ;
#19255 = CARTESIAN_POINT ( 'NONE',  ( -1.860994725976048425, 116.5907236856068181, 0.1449800026146565723 ) ) ;
#19256 = B_SPLINE_CURVE_WITH_KNOTS ( 'NONE', 3,
 ( #29102, #36148, #6533, #35509 ),
 .UNSPECIFIED., .F., .F.,
 ( 4, 4 ),
 ( 0.5009815572441199683, 1.000000000000000000 ),
 .UNSPECIFIED. ) ;
#19257 = ORIENTED_EDGE ( 'NONE', *, *, #11328, .T. ) ;
#19258 = CARTESIAN_POINT ( 'NONE',  ( -53.73190450750161773, 11.39902669490613896, -3.613030284815582860 ) ) ;
#19259 = CARTESIAN_POINT ( 'NONE',  ( 7.840780172454366870, 122.3995516869274383, -0.3066307168558741747 ) ) ;
#19260 = EDGE_LOOP ( 'NONE', ( #4828, #4950, #32175, #8862 ) ) ;
#19261 = CARTESIAN_POINT ( 'NONE',  ( 1.330693927565623991, 115.7029491485453576, -1.688181875448171665 ) ) ;
#19262 = CARTESIAN_POINT ( 'NONE',  ( -14.19780223135882835, 138.9094276006951247, -0.4095818057664819545 ) ) ;
#19263 = CARTESIAN_POINT ( 'NONE',  ( 6.287662417442902552, -13.15673151805442309, 0.9153646538742283845 ) ) ;
#19264 = CARTESIAN_POINT ( 'NONE',  ( -3.087569247026613617, 117.8293475852256904, 0.6612947004247919924 ) ) ;
#19265 = CARTESIAN_POINT ( 'NONE',  ( -5.924740142096584172, 65.21691166894066782, -1.523999999999994026 ) ) ;
#19266 = CIRCLE ( 'NONE', #33580, 18.32410244842765934 ) ;
#19267 = CARTESIAN_POINT ( 'NONE',  ( 5.799544261406283319, 116.9771394561422539, 0.2896453145609861890 ) ) ;
#19268 = CARTESIAN_POINT ( 'NONE',  ( 11.75192402136879366, 130.2587789749062210, 0.3484658256491862116 ) ) ;
#19269 = CARTESIAN_POINT ( 'NONE',  ( 4.855010706775262364, 115.6909491485453145, -1.281361498472391336 ) ) ;
#19270 = CARTESIAN_POINT ( 'NONE',  ( 0.4504873307288463358, 16.48674109716143477, 0.8651787211232140340 ) ) ;
#19271 = CARTESIAN_POINT ( 'NONE',  ( -20.36427691206304402, 129.0035756037533758, -0.5974333909176803292 ) ) ;
#19272 = CARTESIAN_POINT ( 'NONE',  ( -36.65473259702432784, 28.27472347546385123, -1.524000000000003574 ) ) ;
#19273 = CYLINDRICAL_SURFACE ( 'NONE', #39065, 18.32410244842765934 ) ;
#19274 = EDGE_LOOP ( 'NONE', ( #32381, #1019 ) ) ;
#19275 = CARTESIAN_POINT ( 'NONE',  ( -5.594955721643887436, 117.4948600716806908, 0.6777700223702270987 ) ) ;
#19276 = ORIENTED_EDGE ( 'NONE', *, *, #13059, .F. ) ;
#19277 = CARTESIAN_POINT ( 'NONE',  ( -10.38331224698210420, 56.51499999999998636, 4.381499999999999950 ) ) ;
#19278 = CARTESIAN_POINT ( 'NONE',  ( 19.06843068773014238, 131.8899703912256314, 2.039348754248471174 ) ) ;
#19279 = CARTESIAN_POINT ( 'NONE',  ( 11.46709954559036859, 121.1873859956591843, -1.221572053168039185 ) ) ;
#19280 = CARTESIAN_POINT ( 'NONE',  ( 3.006797519324799772, 15.24566924451032435, -7.865828698519952589 ) ) ;
#19281 = CARTESIAN_POINT ( 'NONE',  ( -1.253347288035753460, 159.2526592949493534, -1.130111582746273768 ) ) ;
#19282 = CARTESIAN_POINT ( 'NONE',  ( 4.739872878304939974, 117.9513957112883276, -0.6506048652930741527 ) ) ;
#19283 = EDGE_CURVE ( 'NONE', #11900, #2737, #34438, .T. ) ;
#19284 = CARTESIAN_POINT ( 'NONE',  ( 3.430439322123106649, 108.6576027043044377, 4.130303871225995849 ) ) ;
#19285 = EDGE_CURVE ( 'NONE', #39868, #15268, #10393, .T. ) ;
#19286 = CARTESIAN_POINT ( 'NONE',  ( -15.72781737677524738, 145.6903699455376113, -0.2627434299976844634 ) ) ;
#19287 = CARTESIAN_POINT ( 'NONE',  ( -19.09005709338569545, 148.2829752965438956, -2.500029303593213292 ) ) ;
#19288 = CARTESIAN_POINT ( 'NONE',  ( 5.933841582263978509, -14.80544765534526341, -0.2634432552157287555 ) ) ;
#19289 = CIRCLE ( 'NONE', #5721, 14.91798719394653716 ) ;
#19290 = DIRECTION ( 'NONE',  ( -0.8745520943968235761, 0.4849315768086558398, -5.691349986800547879E-16 ) ) ;
#19291 = CARTESIAN_POINT ( 'NONE',  ( -47.65206802627297833, 20.46304711373551299, -5.210715034831075343 ) ) ;
#19292 = VERTEX_POINT ( 'NONE', #27006 ) ;
#19293 = CARTESIAN_POINT ( 'NONE',  ( 18.29412156995171301, 148.6295804641074483, 2.431306780064794726 ) ) ;
#19294 = CARTESIAN_POINT ( 'NONE',  ( -15.38000172824470368, 147.8312228276848543, -0.3073290369001835387 ) ) ;
#19295 = CARTESIAN_POINT ( 'NONE',  ( -5.433597316833275848, 122.7706071131974994, 0.004560450986766876290 ) ) ;
#19296 = CARTESIAN_POINT ( 'NONE',  ( -5.416678580886389760, 20.69493382693234196, -6.515560366292809213 ) ) ;
#19297 = CARTESIAN_POINT ( 'NONE',  ( 14.64564643111550879, 139.2174805014774392, 1.155614491733866211 ) ) ;
#19298 = CARTESIAN_POINT ( 'NONE',  ( 19.54046365593621815, 128.7319734376252143, -0.5398260955622251611 ) ) ;
#19299 = FACE_OUTER_BOUND ( 'NONE', #4743, .T. ) ;
#19300 = VECTOR ( 'NONE', #19346, 1000.000000000000000 ) ;
#19301 = DIRECTION ( 'NONE',  ( -0.3256999990547775337, -0.9454731675810359448, 0.000000000000000000 ) ) ;
#19302 = EDGE_CURVE ( 'NONE', #22885, #26876, #13799, .T. ) ;
#19303 = CARTESIAN_POINT ( 'NONE',  ( -13.43845804798116106, 156.9141898299356512, -0.2685323735513600041 ) ) ;
#19304 = ORIENTED_EDGE ( 'NONE', *, *, #35773, .T. ) ;
#19305 = CARTESIAN_POINT ( 'NONE',  ( 6.326077193401762777, 119.9160889050335186, -0.9682899027979984252 ) ) ;
#19306 = CARTESIAN_POINT ( 'NONE',  ( 6.088215427201158825, -14.09263546912463028, 1.889225179162022927 ) ) ;
#19307 = VECTOR ( 'NONE', #132, 999.9999999999998863 ) ;
#19308 = CARTESIAN_POINT ( 'NONE',  ( -15.71402047398562019, 147.5983985311728759, -1.037567014598419490 ) ) ;
#19309 = CARTESIAN_POINT ( 'NONE',  ( 1.960603841440088146, -15.05276691075377293, 5.730201639535507319 ) ) ;
#19310 = CARTESIAN_POINT ( 'NONE',  ( 6.059261036834405978, 56.98375738874752727, -5.016499999999998849 ) ) ;
#19311 = CARTESIAN_POINT ( 'NONE',  ( 15.54780490071025056, 120.7212560704218589, 0.3275748350740995130 ) ) ;
#19312 = ORIENTED_EDGE ( 'NONE', *, *, #29504, .T. ) ;
#19313 = CARTESIAN_POINT ( 'NONE',  ( 2.267534764145236803, 6.115564135048844108, 4.037922524061999141 ) ) ;
#19314 = CARTESIAN_POINT ( 'NONE',  ( -14.91134437181082717, 120.3281135998953459, -0.2979641475761142244 ) ) ;
#19315 = CARTESIAN_POINT ( 'NONE',  ( -4.854889821517595294, 117.4070850134769728, 0.9981808394738391765 ) ) ;
#19316 = CARTESIAN_POINT ( 'NONE',  ( -4.345705637489792217, 70.43763872253877878, 1.270000000000005125 ) ) ;
#19317 = LINE ( 'NONE', #28286, #38469 ) ;
#19318 = CARTESIAN_POINT ( 'NONE',  ( -7.851952014490078291, 122.3505504179107390, 0.3628578151170098742 ) ) ;
#19319 =( BOUNDED_SURFACE ( )  B_SPLINE_SURFACE ( 2, 3, ( 
 ( #36917, #7942, #26692, #23682, #935, #1139, #11125, #29885, #13905, #16670, #7524, #36702, #24112, #26478, #26895, #20701, #30507, #14305, #1348, #7735, #39482, #13492, #20485, #37120, #33726, #10288, #14106, #17509, #17308, #13698, #27317, #29676, #16884, #23258, #3712, #30296, #40331, #36292, #7112, #23900, #40117, #20071, #17091, #23468, #10910, #39909, #33093, #33512, #519, #10703 ),
 ( #7315, #39699, #4550, #10498, #20274, #4132, #30094, #4762, #11965, #40537, #11333, #21321, #34140, #34349, #8142, #24321, #30713, #18133, #8567, #21529, #15149, #21114, #4967, #1564, #1768, #17714, #24958, #2403, #14939, #31138, #17925, #11754, #1977, #18556, #40742, #20911, #37959, #25175, #24742, #14521, #27531, #15362, #27941, #30930, #14729, #5180, #40948, #37744, #34561, #28369 ),
 ( #38176, #27731, #5388, #18343, #31349, #41376, #11539, #2192, #37327, #28154, #41160, #12182, #24522, #8784, #21742, #31561, #33933, #37528, #34768, #8353, #5601, #12798, #29413, #13006, #28580, #19394, #35817, #22575, #31983, #19600, #5808, #22157, #31774, #253, #35606, #6633, #2615, #15575, #40, #32400, #41588, #12598, #25999, #26213, #39008, #13230, #2821, #9818, #22784, #8990 ) ),
 .UNSPECIFIED., .F., .F., .T. ) 
 B_SPLINE_SURFACE_WITH_KNOTS ( ( 3, 3 ),
 ( 4, 2, 2, 2, 2, 2, 2, 2, 2, 2, 2, 2, 2, 2, 2, 2, 2, 2, 2, 2, 2, 2, 2, 2, 4 ),
 ( 0.000000000000000000, 1.000000000000000000 ),
 ( 0.000000000000000000, 0.001458241944942368154, 0.002916483889884736308, 0.005832967779769472616, 0.01166593555953894523, 0.01458241944942368154, 0.01749890333930841785, 0.01895714528425078427, 0.02041538722919315416, 0.02114450820166433737, 0.02150906868789993071, 0.02187362917413552404, 0.02223818966037111738, 0.02260275014660670725, 0.02296731063284229712, 0.02305845075440119546, 0.02310402081518064463, 0.02312680584557037095, 0.02313250210316779992, 0.02313819836076523237, 0.02314959087596009379, 0.02319516093673954296, 0.02324073099751899213, 0.02328630105829844130, 0.02333187111907789046 ),
 .UNSPECIFIED. ) 
 GEOMETRIC_REPRESENTATION_ITEM ( )  RATIONAL_B_SPLINE_SURFACE ( (
 ( 1.000000000000000000, 1.000000000000000000, 1.000000000000000000, 1.000000000000000000, 1.000000000000000000, 1.000000000000000000, 1.000000000000000000, 1.000000000000000000, 1.000000000000000000, 1.000000000000000000, 1.000000000000000000, 1.000000000000000000, 1.000000000000000000, 1.000000000000000000, 1.000000000000000000, 1.000000000000000000, 1.000000000000000000, 1.000000000000000000, 1.000000000000000000, 1.000000000000000000, 1.000000000000000000, 1.000000000000000000, 1.000000000000000000, 1.000000000000000000, 1.000000000000000000, 1.000000000000000000, 1.000000000000000000, 1.000000000000000000, 1.000000000000000000, 1.000000000000000000, 1.000000000000000000, 1.000000000000000000, 1.000000000000000000, 1.000000000000000000, 1.000000000000000000, 1.000000000000000000, 1.000000000000000000, 1.000000000000000000, 1.000000000000000000, 1.000000000000000000, 1.000000000000000000, 1.000000000000000000, 1.000000000000000000, 1.000000000000000000, 1.000000000000000000, 1.000000000000000000, 1.000000000000000000, 1.000000000000000000, 1.000000000000000000, 1.000000000000000000),
 ( 0.9987193938133573923, 0.9996013059079669194, 0.9991963860900630046, 0.9949866313569200038, 0.9909603791773133885, 0.9774858857087078690, 0.9654485462739429424, 0.9208787474569170017, 0.8807605768912754041, 0.8373543814104991156, 0.8249666374385254963, 0.8044008243459336294, 0.7962249832271174332, 0.7861950991335926453, 0.7832680976431367625, 0.7777782220875287811, 0.7752303374714799578, 0.7716286403903510616, 0.7703172242827316385, 0.7685261186011436152, 0.7673635575496201566, 0.7657163664523159996, 0.7656514573011637959, 0.7645255059892569482, 0.7630494482540092216, 0.7607147317280203991, 0.7600215756489282493, 0.7585094466894809484, 0.7575231611504058549, 0.7546848085681980844, 0.7541407386780549782, 0.7516848864288520060, 0.7509064819841395622, 0.7462986158548496896, 0.7479156148892531775, 0.7339777749611771096, 0.7233604987256092578, 0.7138238211873346728, 0.7102391262371019476, 0.6994720207875538831, 0.6929862625710326851, 0.6601362149681273550, 0.6323867238837976856, 0.5714353381031282986, 0.5388352690740847439, 0.4817946329374578895, 0.4578268140822101540, 0.4260966422725533942, 0.4180307774937941923, 0.4190531958282215919),
 ( 1.000000000000000000, 1.000000000000000000, 1.000000000000000000, 1.000000000000000000, 1.000000000000000000, 1.000000000000000000, 1.000000000000000000, 1.000000000000000000, 1.000000000000000000, 1.000000000000000000, 1.000000000000000000, 1.000000000000000000, 1.000000000000000000, 1.000000000000000000, 1.000000000000000000, 1.000000000000000000, 1.000000000000000000, 1.000000000000000000, 1.000000000000000000, 1.000000000000000000, 1.000000000000000000, 1.000000000000000000, 1.000000000000000000, 1.000000000000000000, 1.000000000000000000, 1.000000000000000000, 1.000000000000000000, 1.000000000000000000, 1.000000000000000000, 1.000000000000000000, 1.000000000000000000, 1.000000000000000000, 1.000000000000000000, 1.000000000000000000, 1.000000000000000000, 1.000000000000000000, 1.000000000000000000, 1.000000000000000000, 1.000000000000000000, 1.000000000000000000, 1.000000000000000000, 1.000000000000000000, 1.000000000000000000, 1.000000000000000000, 1.000000000000000000, 1.000000000000000000, 1.000000000000000000, 1.000000000000000000, 1.000000000000000000, 1.000000000000000000) ) ) 
 REPRESENTATION_ITEM ( '' )  SURFACE ( )  );
#19320 = CARTESIAN_POINT ( 'NONE',  ( -4.623654898565560778, 8.549082320728111029, 0.09932813335659773646 ) ) ;
#19321 = CARTESIAN_POINT ( 'NONE',  ( 3.104962560943341554, 159.3365417412370562, 0.8543937160244111650 ) ) ;
#19322 = CARTESIAN_POINT ( 'NONE',  ( 15.64207015331054862, 147.2204672151589193, 0.3125657877211908686 ) ) ;
#19324 = CARTESIAN_POINT ( 'NONE',  ( 5.883034912960730445, 118.4234969239897453, -0.8666102449821462272 ) ) ;
#19323 = CARTESIAN_POINT ( 'NONE',  ( 4.781543117820231004, 56.51500000000001478, 4.872198453344559255 ) ) ;
#19325 = CARTESIAN_POINT ( 'NONE',  ( 3.900846188197024667, 12.44727460162280863, 2.488979119290085862 ) ) ;
#19326 = CARTESIAN_POINT ( 'NONE',  ( -15.06876432237292995, 120.9194639129320734, -0.9861043747356995626 ) ) ;
#19327 = EDGE_LOOP ( 'NONE', ( #26474, #1762, #7822, #34706 ) ) ;
#19328 = CARTESIAN_POINT ( 'NONE',  ( -4.537977675602711258, 121.1059516323014549, 0.1178196913276178259 ) ) ;
#19329 = CARTESIAN_POINT ( 'NONE',  ( 2.850627862023833892, -15.32561772411503220, 5.765353718581858189 ) ) ;
#19330 = CARTESIAN_POINT ( 'NONE',  ( -3.590790587123838709E-14, 56.51998046905274009, 0.000000000000000000 ) ) ;
#19331 = ADVANCED_FACE ( 'NONE', ( #14207 ), #33620, .F. ) ;
#19332 = ORIENTED_EDGE ( 'NONE', *, *, #25820, .F. ) ;
#19333 = CARTESIAN_POINT ( 'NONE',  ( 10.99314024304344883, 156.0189320485970086, 2.156370349642059203 ) ) ;
#19334 = CARTESIAN_POINT ( 'NONE',  ( 5.137966006445064515, 56.84472104120882108, 5.330653870689094020 ) ) ;
#19335 = CARTESIAN_POINT ( 'NONE',  ( -12.21488373879589240, 71.11999999999999034, 4.381499999999999950 ) ) ;
#19336 = CARTESIAN_POINT ( 'NONE',  ( -1.363555988950395870, 159.4956652290339605, 0.6451735917158238909 ) ) ;
#19337 = CARTESIAN_POINT ( 'NONE',  ( 4.931598085382976393, 117.4109156735239452, -0.9380226465277491377 ) ) ;
#19338 = CARTESIAN_POINT ( 'NONE',  ( 9.739177221546302832, 118.0756159837034716, -0.1634508798788866235 ) ) ;
#19339 = EDGE_CURVE ( 'NONE', #15671, #2842, #17150, .T. ) ;
#19340 = DIRECTION ( 'NONE',  ( 1.000000000000000000, -5.463695987328526437E-16, 0.000000000000000000 ) ) ;
#19341 = CARTESIAN_POINT ( 'NONE',  ( -48.82359235824656452, 18.05626978637514313, 5.103416509772343623 ) ) ;
#19342 = CARTESIAN_POINT ( 'NONE',  ( -46.95726096424718321, 25.94444535518948669, 0.08936005021614831789 ) ) ;
#19343 = FACE_OUTER_BOUND ( 'NONE', #25628, .T. ) ;
#19344 = VERTEX_POINT ( 'NONE', #1037 ) ;
#19345 = CARTESIAN_POINT ( 'NONE',  ( -44.55074271434504851, 21.27721161058206789, 3.389857510897057224 ) ) ;
#19346 = DIRECTION ( 'NONE',  ( -0.7071067811865436870, 0.000000000000000000, -0.7071067811865513475 ) ) ;
#19347 = CARTESIAN_POINT ( 'NONE',  ( -4.587462187188385165, 118.0383919587454642, 0.6669115617459517864 ) ) ;
#19348 = DIRECTION ( 'NONE',  ( 0.000000000000000000, 0.000000000000000000, 1.000000000000000000 ) ) ;
#19349 = VERTEX_POINT ( 'NONE', #4027 ) ;
#19350 = ORIENTED_EDGE ( 'NONE', *, *, #8135, .F. ) ;
#19351 = DIRECTION ( 'NONE',  ( -0.5810519254489896479, 0.8138664877804110409, 0.000000000000000000 ) ) ;
#19352 = EDGE_CURVE ( 'NONE', #31634, #25703, #36602, .T. ) ;
#19353 = CARTESIAN_POINT ( 'NONE',  ( 8.406963674677495391, 119.7153034306578974, -1.094654629815129177 ) ) ;
#19354 = CARTESIAN_POINT ( 'NONE',  ( -5.433204070470928571, 117.5340897209903517, -0.8253704096831885328 ) ) ;
#19355 = CARTESIAN_POINT ( 'NONE',  ( 4.767144615469286251, 117.8468057660086430, 0.9623966903202456624 ) ) ;
#19356 = CARTESIAN_POINT ( 'NONE',  ( -58.83227707057486811, -0.08366279997995551554, -1.529465441686574059E-14 ) ) ;
#19357 = CARTESIAN_POINT ( 'NONE',  ( -9.932629385191992455, 123.7598584631124794, -1.097969866555963403 ) ) ;
#19358 = CARTESIAN_POINT ( 'NONE',  ( -3.014963585057483630, 115.7029491485453576, -1.667984629301600075 ) ) ;
#19359 = EDGE_CURVE ( 'NONE', #20685, #38830, #4192, .T. ) ;
#19360 = CARTESIAN_POINT ( 'NONE',  ( -16.60960244842765832, 1.470586496075005742E-15, 0.000000000000000000 ) ) ;
#19361 = CARTESIAN_POINT ( 'NONE',  ( 14.94465077092626970, 61.74681991364688827, 5.072843609925764774 ) ) ;
#19362 = CARTESIAN_POINT ( 'NONE',  ( 7.669306984062364663, 124.7206709383052043, 0.1533317827557520718 ) ) ;
#19363 = CARTESIAN_POINT ( 'NONE',  ( -16.94372847238233248, 146.2370505443881257, -1.929411111270964652 ) ) ;
#19364 = CARTESIAN_POINT ( 'NONE',  ( -0.0002734175339917587714, 159.6054662015457382, 0.01368293144939993107 ) ) ;
#19365 = CARTESIAN_POINT ( 'NONE',  ( -3.646844371775973315, 115.7029492783617854, 1.479374498987925168 ) ) ;
#19366 = CARTESIAN_POINT ( 'NONE',  ( 1.961646697876492373, -0.1315482170498871728, -4.191205975169975950 ) ) ;
#19368 = ORIENTED_EDGE ( 'NONE', *, *, #33617, .T. ) ;
#19367 = CARTESIAN_POINT ( 'NONE',  ( 16.63860074592936300, 155.2617138006751532, 0.9902706816744292206 ) ) ;
#19369 = CARTESIAN_POINT ( 'NONE',  ( -19.64403260974359355, 72.50569198072959409, -1.524000000000002242 ) ) ;
#19370 = CARTESIAN_POINT ( 'NONE',  ( 3.057239904206551895, -15.51127639645041789, 4.278020201805971645 ) ) ;
#19371 = CARTESIAN_POINT ( 'NONE',  ( -19.17469122182637875, 148.2829752965438956, 1.735408567215429576 ) ) ;
#19372 = CARTESIAN_POINT ( 'NONE',  ( -0.01718310852247704676, 5.323846764136113130, -0.9747645957998940514 ) ) ;
#19373 = CARTESIAN_POINT ( 'NONE',  ( -21.37844900359480960, 132.5159896776619917, -0.8378797052005129142 ) ) ;
#19374 = CARTESIAN_POINT ( 'NONE',  ( -0.5978751570792395498, 11.96162690172616294, -0.7744233872902203109 ) ) ;
#19375 = EDGE_LOOP ( 'NONE', ( #37165, #40522, #27086, #21784 ) ) ;
#19376 = VERTEX_POINT ( 'NONE', #37024 ) ;
#19377 = CARTESIAN_POINT ( 'NONE',  ( -43.98989719630797168, 21.38545485255711398, 2.905481552205958717 ) ) ;
#19378 = EDGE_CURVE ( 'NONE', #3203, #21896, #5544, .T. ) ;
#19379 = CARTESIAN_POINT ( 'NONE',  ( 4.183818394377241567, 118.4033805524614849, 0.7412457532797814830 ) ) ;
#19380 = DIRECTION ( 'NONE',  ( 1.000000000000000000, 0.000000000000000000, 0.000000000000000000 ) ) ;
#19381 = CIRCLE ( 'NONE', #3783, 0.2540000000000012248 ) ;
#19382 = CARTESIAN_POINT ( 'NONE',  ( -6.515494676152068010, 155.4519854478747902, 0.9200225795255462247 ) ) ;
#19383 = CARTESIAN_POINT ( 'NONE',  ( 3.354142537596241702, -14.24820561377959649, 4.738596845331590757 ) ) ;
#19384 = CARTESIAN_POINT ( 'NONE',  ( 17.98452544307424006, 146.6345634702618952, -1.580200905155534574 ) ) ;
#19385 = CARTESIAN_POINT ( 'NONE',  ( -2.522816026436837333, 158.1729697732556588, -1.709197703933636125 ) ) ;
#19386 = CARTESIAN_POINT ( 'NONE',  ( -17.14499999999999957, 71.11999999999999034, -1.904999999999999583 ) ) ;
#19387 = CARTESIAN_POINT ( 'NONE',  ( 8.682895647160147945, 118.1675475142423437, 0.9202857585879714586 ) ) ;
#19388 = CARTESIAN_POINT ( 'NONE',  ( -0.08015702708839873847, 38.63184331614436218, 0.5155861021556068513 ) ) ;
#19389 = CARTESIAN_POINT ( 'NONE',  ( 15.81463230642810025, 145.9351319680867221, -0.01551611691150889434 ) ) ;
#19390 = VERTEX_POINT ( 'NONE', #13591 ) ;
#19391 = DIRECTION ( 'NONE',  ( -0.8745520943968235761, 0.4849315768086558398, -4.268512490100410909E-16 ) ) ;
#19392 = DIRECTION ( 'NONE',  ( 5.188838149069472160E-16, -1.699382548006136559E-16, -1.000000000000000000 ) ) ;
#19393 = EDGE_CURVE ( 'NONE', #2940, #23452, #17198, .T. ) ;
#19394 = CARTESIAN_POINT ( 'NONE',  ( -58.36601048454566154, 0.2708230323985594268, 0.9148880203688037893 ) ) ;
#19395 = EDGE_CURVE ( 'NONE', #3974, #34427, #35413, .T. ) ;
#19396 = CARTESIAN_POINT ( 'NONE',  ( -0.01596947694136538129, 156.4635559983122448, 0.7991779281049289363 ) ) ;
#19397 = DIRECTION ( 'NONE',  ( -0.9998004120163609398, 0.000000000000000000, -0.01997839162482749689 ) ) ;
#19398 = CARTESIAN_POINT ( 'NONE',  ( 4.735783051744282268, 116.7698466342620378, 0.01422048256815234418 ) ) ;
#19399 = CARTESIAN_POINT ( 'NONE',  ( -2.686051902181577855, 107.2142675576569530, 4.629644704627760454 ) ) ;
#19400 = FACE_OUTER_BOUND ( 'NONE', #36599, .T. ) ;
#19401 = CARTESIAN_POINT ( 'NONE',  ( 4.611808778022512989, -11.57686662695173929, 0.3579861242195471194 ) ) ;
#19402 = CARTESIAN_POINT ( 'NONE',  ( -3.469629447173708137, 31.73985764285065869, 0.6454790148241180692 ) ) ;
#19403 = CARTESIAN_POINT ( 'NONE',  ( 20.60480707444001069, 141.5323519391372997, 2.354057365763566168 ) ) ;
#19404 = VECTOR ( 'NONE', #25554, 1000.000000000000114 ) ;
#19405 = CARTESIAN_POINT ( 'NONE',  ( -3.182929088426432074, 26.46582164074821009, -3.363547984189534379 ) ) ;
#19406 = CARTESIAN_POINT ( 'NONE',  ( 3.771486885279011325, -13.69470344665998773, -7.544622693077620568 ) ) ;
#19407 = CARTESIAN_POINT ( 'NONE',  ( 8.741995348237278307, 118.0171073936068069, -0.4338951289030384406 ) ) ;
#19408 = CARTESIAN_POINT ( 'NONE',  ( 0.06390210066009133216, 106.1446358501009826, -5.228158908302722452 ) ) ;
#19409 = CARTESIAN_POINT ( 'NONE',  ( -5.152689475313444234, 116.8412042432202185, -0.1029630068797482562 ) ) ;
#19410 = CARTESIAN_POINT ( 'NONE',  ( 0.4328132676559295899, 105.9956125065441199, -5.278019706336061212 ) ) ;
#19411 = CARTESIAN_POINT ( 'NONE',  ( -2.419178179742970336, 105.1243363418205234, 4.754978004784589096 ) ) ;
#19412 = CARTESIAN_POINT ( 'NONE',  ( 4.377640660406503237, 26.40621510375495973, 1.544744264128281364 ) ) ;
#19413 = EDGE_CURVE ( 'NONE', #2737, #6467, #28314, .T. ) ;
#19414 = CARTESIAN_POINT ( 'NONE',  ( -47.00787117332040310, 24.49876931072293829, -2.333946431867834015 ) ) ;
#19415 = PLANE ( 'NONE',  #12402 ) ;
#19416 = CARTESIAN_POINT ( 'NONE',  ( 2.769760999665409340, -14.92388480464812872, 4.423285184949336646 ) ) ;
#19417 = CARTESIAN_POINT ( 'NONE',  ( 2.656358736808067000, 121.0686911241271702, -0.2846299364715210722 ) ) ;
#19418 = CARTESIAN_POINT ( 'NONE',  ( -0.3417028577848571502, 116.8490449975401617, 0.2775575361029122279 ) ) ;
#19419 = VERTEX_POINT ( 'NONE', #5077 ) ;
#19420 = CARTESIAN_POINT ( 'NONE',  ( -5.309060684617390516E-14, 83.56599999999998829, 0.000000000000000000 ) ) ;
#19421 = ORIENTED_EDGE ( 'NONE', *, *, #22219, .F. ) ;
#19422 = CARTESIAN_POINT ( 'NONE',  ( -6.642949970123351200, 30.31777535218072117, -0.3443277341910152556 ) ) ;
#19423 = CARTESIAN_POINT ( 'NONE',  ( 5.933841582263978509, -14.80544765534526341, -0.2634432552157287555 ) ) ;
#19424 = CARTESIAN_POINT ( 'NONE',  ( -13.46871114105396039, 122.4565580348552913, 1.263039180185647314 ) ) ;
#19425 = CARTESIAN_POINT ( 'NONE',  ( 5.259787267153561707, 158.8115599018184412, -1.116423854902495849 ) ) ;
#19426 = CARTESIAN_POINT ( 'NONE',  ( 4.364008504204949013, 7.202613900313124873, 1.580794030135405537 ) ) ;
#19427 = CARTESIAN_POINT ( 'NONE',  ( -58.01740762695335718, 1.024996124235854955, -1.342718164770963840 ) ) ;
#19428 = ORIENTED_EDGE ( 'NONE', *, *, #28421, .F. ) ;
#19429 = CARTESIAN_POINT ( 'NONE',  ( -51.89660998226970889, 12.88425699701367577, -4.274492870977415038 ) ) ;
#19430 = CARTESIAN_POINT ( 'NONE',  ( -14.60500000000000043, 71.11999999999999034, -1.904999999999999583 ) ) ;
#19431 = CARTESIAN_POINT ( 'NONE',  ( 4.973583767373020770, 117.3966162183443203, 0.9753880922370259388 ) ) ;
#19432 = B_SPLINE_SURFACE_WITH_KNOTS ( 'NONE', 5, 3, ( 
 ( #6697, #532, #32895, #29480 ),
 ( #13074, #13505, #38862, #112 ),
 ( #9673, #26065, #322, #26493 ),
 ( #13713, #10304, #39284, #33316 ),
 ( #39075, #9877, #39498, #39713 ),
 ( #35674, #29265, #22847, #35887 ),
 ( #3515, #13289, #26707, #26274 ),
 ( #10089, #4146, #23063, #10514 ) ),
 .UNSPECIFIED., .F., .F., .F.,
 ( 6, 2, 6 ),
 ( 4, 4 ),
 ( 0.000000000000000000, 0.5000000000000000000, 1.000000000000000000 ),
 ( -0.002373312499999994350, 0.03277393749999998884 ),
 .UNSPECIFIED. ) ;
#19433 = CARTESIAN_POINT ( 'NONE',  ( -3.633016119382598941, 156.6183338678525558, 1.377765736259032758 ) ) ;
#19434 = CARTESIAN_POINT ( 'NONE',  ( 5.041094711636397996, 117.2685085068581827, 0.6814997454729904147 ) ) ;
#19435 = CARTESIAN_POINT ( 'NONE',  ( 7.522503210159232623, 120.3045338523282197, -1.038419263833407324 ) ) ;
#19436 = CARTESIAN_POINT ( 'NONE',  ( -19.59170213216434320, 150.6586468064772646, -2.354958926090490845 ) ) ;
#19437 = CARTESIAN_POINT ( 'NONE',  ( -57.00508801794419611, 2.691366720778187727, -1.977812201481553567 ) ) ;
#19438 = EDGE_LOOP ( 'NONE', ( #5833, #32444, #32657, #4911, #38520, #33190, #28553, #13902, #14595 ) ) ;
#19439 = CARTESIAN_POINT ( 'NONE',  ( 4.485924072207432722, 118.1136089101166533, -0.5726866988169239114 ) ) ;
#19440 = CARTESIAN_POINT ( 'NONE',  ( 13.98505335951042916, 150.2679186505038160, -0.6609695396245743870 ) ) ;
#19441 = AXIS2_PLACEMENT_3D ( 'NONE', #17590, #1846, #2055 ) ;
#19442 = ORIENTED_EDGE ( 'NONE', *, *, #27160, .T. ) ;
#19443 = CARTESIAN_POINT ( 'NONE',  ( -17.39571694528383361, 144.3974720067888313, -2.245075470287479114 ) ) ;
#19444 = CARTESIAN_POINT ( 'NONE',  ( 2.617865251411226613, -15.35234423845867369, 4.678879665404411803 ) ) ;
#19445 = FACE_OUTER_BOUND ( 'NONE', #41399, .T. ) ;
#19446 = CARTESIAN_POINT ( 'NONE',  ( 18.35410564743290962, 77.35382415001784295, -5.392902600000141433 ) ) ;
#19447 = CARTESIAN_POINT ( 'NONE',  ( -4.847551152455588763, 117.7642220418352679, 0.8118171574421505499 ) ) ;
#19448 = CARTESIAN_POINT ( 'NONE',  ( 1.387234972287218593, 119.7856413326322667, 0.5781392410077789146 ) ) ;
#19449 = CARTESIAN_POINT ( 'NONE',  ( -19.68500000000000227, 71.11999999999999034, 5.016499999999999737 ) ) ;
#19450 = CARTESIAN_POINT ( 'NONE',  ( 3.979181138743986601, 26.09377549647152961, 2.406711837290479661 ) ) ;
#19451 = CARTESIAN_POINT ( 'NONE',  ( 10.32597032162030892, 126.0505730134521230, 0.3842079712423250859 ) ) ;
#19452 = LINE ( 'NONE', #9665, #41935 ) ;
#19453 = CARTESIAN_POINT ( 'NONE',  ( -46.25688858429103334, 20.73875112231585760, -4.700046123029353318 ) ) ;
#19454 = CARTESIAN_POINT ( 'NONE',  ( -6.426369768295692736E-14, 159.6054662015457382, 1.032716915552223178E-16 ) ) ;
#19455 = CARTESIAN_POINT ( 'NONE',  ( -18.35410564743290607, 77.35382415001784295, 5.016499999999999737 ) ) ;
#19456 = LINE ( 'NONE', #6695, #39744 ) ;
#19457 = CARTESIAN_POINT ( 'NONE',  ( -3.745035802202505265E-14, 57.78499999999999659, -1.904999999999999805 ) ) ;
#19458 = FACE_OUTER_BOUND ( 'NONE', #1849, .T. ) ;
#19459 = DIRECTION ( 'NONE',  ( -0.9998004120163609398, 0.000000000000000000, -0.01997839162482749689 ) ) ;
#19460 = CARTESIAN_POINT ( 'NONE',  ( -55.52324119379100864, 8.418761648454426094, 1.955819887484142372 ) ) ;
#19461 = VECTOR ( 'NONE', #21928, 1000.000000000000000 ) ;
#19462 = CARTESIAN_POINT ( 'NONE',  ( -57.07867440696631434, 2.606095844753547830, 1.988717289889800677 ) ) ;
#19463 = CARTESIAN_POINT ( 'NONE',  ( -1.843513859164668034, 116.5452236745340429, 0.1029321673164913797 ) ) ;
#19464 = CIRCLE ( 'NONE', #8599, 0.6350000000000014522 ) ;
#19465 = ORIENTED_EDGE ( 'NONE', *, *, #18922, .F. ) ;
#19466 = CARTESIAN_POINT ( 'NONE',  ( -50.45326722236683281, 19.63324548489221044, -2.269669894115913689 ) ) ;
#19467 = CIRCLE ( 'NONE', #24916, 0.3809999999999984510 ) ;
#19468 = CARTESIAN_POINT ( 'NONE',  ( 6.986329010373957260, 121.9533422367003510, 0.08619055661058230844 ) ) ;
#19469 = VERTEX_POINT ( 'NONE', #15471 ) ;
#19470 = CARTESIAN_POINT ( 'NONE',  ( 1.423520143629432910, 115.7027630957402238, -1.681658721634869513 ) ) ;
#19471 = CARTESIAN_POINT ( 'NONE',  ( -2.816370844846016297, 121.0122979933374978, -0.1218616300372572514 ) ) ;
#19472 = CARTESIAN_POINT ( 'NONE',  ( 6.101987814473650573, -12.39306998090061640, 0.4902605208062851827 ) ) ;
#19473 = CARTESIAN_POINT ( 'NONE',  ( -20.25200034474484667, 150.8812763393641490, 1.391365372170581649 ) ) ;
#19474 = CARTESIAN_POINT ( 'NONE',  ( 10.92199999999999704, 55.98894877578618434, 4.336808689942017736E-15 ) ) ;
#19475 = CARTESIAN_POINT ( 'NONE',  ( 23.06561215160514422, 149.8841935741895384, 0.7910477959972080919 ) ) ;
#19476 = CARTESIAN_POINT ( 'NONE',  ( 8.911975660322296378, 123.9583942952993993, 0.2665811367707756063 ) ) ;
#19477 = CARTESIAN_POINT ( 'NONE',  ( -8.438477507926629428, 69.62414081991882142, 1.524000000000003130 ) ) ;
#19478 = CARTESIAN_POINT ( 'NONE',  ( 0.6244633603679663469, 9.902617207799803367, -0.7572168304597820532 ) ) ;
#19479 = CARTESIAN_POINT ( 'NONE',  ( -23.40831777029536198, 146.8136392739129974, -0.6999192077533367140 ) ) ;
#19480 = CARTESIAN_POINT ( 'NONE',  ( -28.42835727709238114, 77.69497285144578314, 1.269999999999991358 ) ) ;
#19481 = EDGE_LOOP ( 'NONE', ( #13268, #14499, #5129, #36881 ) ) ;
#19482 = CARTESIAN_POINT ( 'NONE',  ( 5.707320923441908889, 118.0767569068514717, 1.090126761366801533 ) ) ;
#19483 = ORIENTED_EDGE ( 'NONE', *, *, #22386, .T. ) ;
#19484 = CARTESIAN_POINT ( 'NONE',  ( -58.35647611463063100, -0.2636741081728710134, -0.1439816294147371889 ) ) ;
#19485 = CARTESIAN_POINT ( 'NONE',  ( 21.49578583461345005, 148.6087350971780836, 2.244132633923697551 ) ) ;
#19486 = CARTESIAN_POINT ( 'NONE',  ( 12.07139305262844076, 121.8643784861682065, -1.276542069712922389 ) ) ;
#19487 = CARTESIAN_POINT ( 'NONE',  ( -0.4136891606132181431, 9.424461778640809584, 0.8817368238460310259 ) ) ;
#19488 = CARTESIAN_POINT ( 'NONE',  ( 1.824569540066833584, 15.47196788996624583, -8.237246883284143451 ) ) ;
#19489 = CARTESIAN_POINT ( 'NONE',  ( -13.41577631804585202, 120.9245410081625209, -1.450210030139598594 ) ) ;
#19490 = CARTESIAN_POINT ( 'NONE',  ( 4.685061364228054082, 117.8874929293646119, -0.8143947462202356657 ) ) ;
#19491 = CARTESIAN_POINT ( 'NONE',  ( 3.930440796539790060, 109.7948460773305897, 3.685213129881072636 ) ) ;
#19492 = CARTESIAN_POINT ( 'NONE',  ( -15.21929369751766714, 143.4245298570049840, -0.2523546585945006249 ) ) ;
#19493 = VERTEX_POINT ( 'NONE', #21217 ) ;
#19494 = CARTESIAN_POINT ( 'NONE',  ( -18.63140056563947411, 147.4429432625130119, -2.446051816127021716 ) ) ;
#19495 = CARTESIAN_POINT ( 'NONE',  ( 5.949011718796170634, -14.81501284647598915, 0.9937821824230966827 ) ) ;
#19496 = LINE ( 'NONE', #3124, #38075 ) ;
#19497 = CARTESIAN_POINT ( 'NONE',  ( -46.20552558087364758, 24.41938074005533466, -2.020549794458512682 ) ) ;
#19499 = EDGE_LOOP ( 'NONE', ( #32150, #28490, #7042, #26234 ) ) ;
#19498 = VECTOR ( 'NONE', #7531, 1000.000000000000227 ) ;
#19500 = CARTESIAN_POINT ( 'NONE',  ( 2.214684683099545470, 157.4004113605966211, 1.675081295071568332 ) ) ;
#19501 = CARTESIAN_POINT ( 'NONE',  ( 4.560443946511397506, -11.68866997254031936, 0.6947937310338139216 ) ) ;
#19502 = CARTESIAN_POINT ( 'NONE',  ( -11.58677707360137532, 17.14500000000000313, 4.474811398758258285 ) ) ;
#19503 = CARTESIAN_POINT ( 'NONE',  ( -4.298926901474686701, 118.7880935209305591, 0.4986311761637902684 ) ) ;
#19504 = CARTESIAN_POINT ( 'NONE',  ( 8.358864306157585133, 27.05150166619590379, -1.223686670289468870 ) ) ;
#19505 = CARTESIAN_POINT ( 'NONE',  ( 9.165636745951982078, 123.6526633469202920, 0.6866826908162830811 ) ) ;
#19506 = CARTESIAN_POINT ( 'NONE',  ( 22.64859486804662581, 149.7032342875954498, -0.6240689893612099137 ) ) ;
#19507 = DIRECTION ( 'NONE',  ( -0.8745520943968249084, 0.4849315768086536194, -5.575199987069925217E-16 ) ) ;
#19509 = AXIS2_PLACEMENT_3D ( 'NONE', #924, #36695, #26889 ) ;
#19508 = DIRECTION ( 'NONE',  ( 0.9454731675810332803, -0.3256999990547855828, 8.537024980200802097E-16 ) ) ;
#19510 = AXIS2_PLACEMENT_3D ( 'NONE', #18851, #131, #13096 ) ;
#19511 = CARTESIAN_POINT ( 'NONE',  ( -0.0002511744761480867835, 116.4254662015457171, 0.01256979787922183657 ) ) ;
#19512 = VERTEX_POINT ( 'NONE', #11431 ) ;
#19513 = CARTESIAN_POINT ( 'NONE',  ( 6.591391745114316691, 120.5237581640276687, -0.8625721502728334045 ) ) ;
#19514 = CARTESIAN_POINT ( 'NONE',  ( 22.83540780336915432, 150.4058779721138421, 0.4563057931615321361 ) ) ;
#19515 = VECTOR ( 'NONE', #9717, 1000.000000000000000 ) ;
#19516 = CARTESIAN_POINT ( 'NONE',  ( -15.98475566209953058, 146.3393691146323761, -1.048177900600803403 ) ) ;
#19517 = CARTESIAN_POINT ( 'NONE',  ( 3.745401017337624872, -13.88268793655436717, 4.204469449000409753 ) ) ;
#19518 = CARTESIAN_POINT ( 'NONE',  ( -5.135293214769152570, 116.9399052598554221, 0.1794300269087395205 ) ) ;
#19519 = CARTESIAN_POINT ( 'NONE',  ( 8.216553068272158811, 117.5004391570743394, 0.1790601237764438691 ) ) ;
#19520 = ORIENTED_EDGE ( 'NONE', *, *, #40789, .F. ) ;
#19521 = CARTESIAN_POINT ( 'NONE',  ( -1.544744425833544099, 4.816215111148435923, 4.377641278133862279 ) ) ;
#19522 = CARTESIAN_POINT ( 'NONE',  ( 3.559183564918581677, 105.1232307390661731, 3.986110174556340979 ) ) ;
#19523 = CARTESIAN_POINT ( 'NONE',  ( -4.923390193968213424, 117.4088236311152542, 0.9490106074932443958 ) ) ;
#19524 = CARTESIAN_POINT ( 'NONE',  ( -4.792324638262704717, 56.51998046905272588, -4.972049999962482758 ) ) ;
#19525 = AXIS2_PLACEMENT_3D ( 'NONE', #13021, #12815, #12612 ) ;
#19526 = CARTESIAN_POINT ( 'NONE',  ( 7.831006910361074880, 122.3515375996227590, 0.6751902815995498575 ) ) ;
#19527 = CARTESIAN_POINT ( 'NONE',  ( -4.137704358559117779, 17.39492794009094823, -2.099109474953318788 ) ) ;
#19528 = CARTESIAN_POINT ( 'NONE',  ( 22.07768208608584359, 150.1365687424457178, 1.739787554465966890 ) ) ;
#19529 = DIRECTION ( 'NONE',  ( -0.8745520943968235761, 0.4849315768086558398, -4.268512490100410909E-16 ) ) ;
#19531 = CARTESIAN_POINT ( 'NONE',  ( 14.84976704640051182, 123.2524255416106342, -1.171266444394655881 ) ) ;
#19530 = CARTESIAN_POINT ( 'NONE',  ( -3.009276887026423264, 44.28946620154572855, 1.210121013456480377 ) ) ;
#19532 = CARTESIAN_POINT ( 'NONE',  ( 0.1277143096572389558, 15.67076514537015974, -4.628409624684062251 ) ) ;
#19533 = CARTESIAN_POINT ( 'NONE',  ( -22.71262516694562805, 146.4845460041848355, -1.645735859231715503 ) ) ;
#19534 = VERTEX_POINT ( 'NONE', #1869 ) ;
#19535 = CARTESIAN_POINT ( 'NONE',  ( -0.006534791579925431325, 156.3267223255430167, 0.3270276925529296275 ) ) ;
#19536 = CARTESIAN_POINT ( 'NONE',  ( 3.428369065731536658, -15.18705194980916851, 5.515041984116586526 ) ) ;
#19537 = DIRECTION ( 'NONE',  ( -0.01731298258488073519, 0.9998501190848635423, -1.788962107505278613E-16 ) ) ;
#19538 = AXIS2_PLACEMENT_3D ( 'NONE', #10163, #32756, #810 ) ;
#19539 = ORIENTED_EDGE ( 'NONE', *, *, #34244, .T. ) ;
#19540 = CARTESIAN_POINT ( 'NONE',  ( -0.01147819631913260877, 118.8623374019222894, 0.5744158801423951966 ) ) ;
#19541 = CARTESIAN_POINT ( 'NONE',  ( -17.14499999999998892, 57.14999999999997726, -4.381499999999999950 ) ) ;
#19542 = CARTESIAN_POINT ( 'NONE',  ( -22.74864191258943080, 148.7873826295267747, 0.7277888646341180712 ) ) ;
#19543 = CARTESIAN_POINT ( 'NONE',  ( 22.40468623258662362, 137.0915487549672491, -0.1281257692620773048 ) ) ;
#19544 = CARTESIAN_POINT ( 'NONE',  ( -5.706393392168954470, 56.51500000000000057, -5.041882957346543570 ) ) ;
#19545 = CARTESIAN_POINT ( 'NONE',  ( -46.72105977771763463, 25.94162485481863456, 1.365922269189760563 ) ) ;
#19546 = CARTESIAN_POINT ( 'NONE',  ( -46.93527007713159804, 25.91000514300129254, 0.2210822239326031835 ) ) ;
#19547 = CARTESIAN_POINT ( 'NONE',  ( 2.049043543842966386, -15.30400295934178345, 5.355738895901667185 ) ) ;
#19548 = CARTESIAN_POINT ( 'NONE',  ( -44.36446822842629700, 21.81554158013422651, 2.896954608336737014 ) ) ;
#19549 = FACE_BOUND ( 'NONE', #9590, .T. ) ;
#19550 = EDGE_CURVE ( 'NONE', #18840, #39307, #28673, .T. ) ;
#19551 = CARTESIAN_POINT ( 'NONE',  ( -4.585060147380330520, 118.0136138934147993, 0.7023266209943478389 ) ) ;
#19552 = CARTESIAN_POINT ( 'NONE',  ( -58.31320831016853390, -0.1895118959954616988, -0.07592354283883193111 ) ) ;
#19553 = ORIENTED_EDGE ( 'NONE', *, *, #2912, .T. ) ;
#19554 = ORIENTED_EDGE ( 'NONE', *, *, #8720, .F. ) ;
#19555 = CARTESIAN_POINT ( 'NONE',  ( 0.03523692298770234738, 115.6909491485452435, -1.763399716047880039 ) ) ;
#19556 =( BOUNDED_CURVE ( )  B_SPLINE_CURVE ( 3, ( #7784, #36344, #17351, #563 ),
 .UNSPECIFIED., .F., .T. ) 
 B_SPLINE_CURVE_WITH_KNOTS ( ( 4, 4 ),
 ( 3.141592653589793116, 4.712388980384689674 ),
 .UNSPECIFIED. ) 
 CURVE ( )  GEOMETRIC_REPRESENTATION_ITEM ( )  RATIONAL_B_SPLINE_CURVE ( ( 1.000000000000000000, 0.8047378541243649375, 0.8047378541243649375, 1.000000000000000000 ) ) 
 REPRESENTATION_ITEM ( '' )  );
#19557 = CARTESIAN_POINT ( 'NONE',  ( 3.544058460572470093, 118.6794394583634329, -0.7947981566704515055 ) ) ;
#19558 = CARTESIAN_POINT ( 'NONE',  ( -4.730021378956903000, 112.7831754354443348, -2.563638443952895418 ) ) ;
#19559 = CARTESIAN_POINT ( 'NONE',  ( 4.696638897187899175, 117.9693123291577024, 0.8144611834090730307 ) ) ;
#19560 = DIRECTION ( 'NONE',  ( -0.9998004120163609398, 0.000000000000000000, -0.01997839162482749342 ) ) ;
#19561 = CARTESIAN_POINT ( 'NONE',  ( -14.05504870572974419, 134.4521314832425389, -1.517394082013088674 ) ) ;
#19562 =( GEOMETRIC_REPRESENTATION_CONTEXT ( 3 ) GLOBAL_UNCERTAINTY_ASSIGNED_CONTEXT ( ( #32100 ) ) GLOBAL_UNIT_ASSIGNED_CONTEXT ( ( #40319, #11317, #33713 ) ) REPRESENTATION_CONTEXT ( 'NONE', 'WORKASPACE' ) );
#19563 = CARTESIAN_POINT ( 'NONE',  ( -3.999779825473023465, 115.7036092819612350, -1.581685738513307626 ) ) ;
#19564 = CARTESIAN_POINT ( 'NONE',  ( -23.21760062652228385, 78.26400813401573942, 1.269999999999993801 ) ) ;
#19565 = DIRECTION ( 'NONE',  ( 0.9816537812491090698, 0.1906721105965065721, 4.769617732184476148E-16 ) ) ;
#19566 = CARTESIAN_POINT ( 'NONE',  ( 3.568456891169458078, 108.6786390861269922, -3.983803253449686110 ) ) ;
#19567 = CARTESIAN_POINT ( 'NONE',  ( -5.014048726638253406, 156.2174774745075183, -1.508183953414442335 ) ) ;
#19568 = ADVANCED_FACE ( 'NONE', ( #2078 ), #18446, .T. ) ;
#19569 = CARTESIAN_POINT ( 'NONE',  ( -13.85159022459153633, 16.59642619247576789, -5.016499999999999737 ) ) ;
#19570 = CARTESIAN_POINT ( 'NONE',  ( -0.02399864187742892577, 159.1630378086529731, 1.200990174154242585 ) ) ;
#19571 = CARTESIAN_POINT ( 'NONE',  ( 5.460438898883120729, 56.51499999999997215, -4.448267477574868956 ) ) ;
#19572 = CARTESIAN_POINT ( 'NONE',  ( -8.439845240644384461, 123.3184153607739404, -0.08348901510681934479 ) ) ;
#19573 = CARTESIAN_POINT ( 'NONE',  ( 1.968029828064305153, -3.592386099649644837, 4.203610184747879508 ) ) ;
#19575 = ORIENTED_EDGE ( 'NONE', *, *, #21909, .T. ) ;
#19574 = CARTESIAN_POINT ( 'NONE',  ( 14.40286820143207969, 120.3907653763288579, 0.8772178161575925337 ) ) ;
#19576 = CARTESIAN_POINT ( 'NONE',  ( -5.078986093043186045, 85.18346620154574111, -0.1014902294541237954 ) ) ;
#19577 = CARTESIAN_POINT ( 'NONE',  ( 3.879201355988149746, -15.32975156973215292, 1.565980057466964670 ) ) ;
#19578 = CARTESIAN_POINT ( 'NONE',  ( -12.22472920326803525, 122.9664497093790629, 1.310580005724927499 ) ) ;
#19579 = CARTESIAN_POINT ( 'NONE',  ( 0.7251766580790658390, 11.37246313919491314, 0.6538263676454795226 ) ) ;
#19580 = CARTESIAN_POINT ( 'NONE',  ( -22.32005725002931484, 150.7328461917231550, -1.166919501784766666 ) ) ;
#19581 = CARTESIAN_POINT ( 'NONE',  ( 0.9253733321238560849, 8.064964547470342637, 0.3089666344597190029 ) ) ;
#19582 = ORIENTED_EDGE ( 'NONE', *, *, #31623, .F. ) ;
#19583 = CARTESIAN_POINT ( 'NONE',  ( -47.34044527953909665, 17.31523404052589399, 1.593293138114921792 ) ) ;
#19584 = CARTESIAN_POINT ( 'NONE',  ( 7.643874070029819556, 124.9344662015457317, 0.1527427953284561934 ) ) ;
#19585 = CARTESIAN_POINT ( 'NONE',  ( 0.000000000000000000, 0.000000000000000000, 0.000000000000000000 ) ) ;
#19586 = CARTESIAN_POINT ( 'NONE',  ( -0.7132078119428603147, 156.3865044363621450, 0.5782112914057383479 ) ) ;
#19587 = CARTESIAN_POINT ( 'NONE',  ( 3.951736590037845609, -12.73914099834651203, 2.215835717905272784 ) ) ;
#19588 = CARTESIAN_POINT ( 'NONE',  ( 9.926448497735728793, 122.5082557396031291, -1.019319756893169115 ) ) ;
#19589 = CARTESIAN_POINT ( 'NONE',  ( -19.26131898708122137, 149.3473233412102275, -2.496341295301664154 ) ) ;
#19590 = CARTESIAN_POINT ( 'NONE',  ( -6.194847070882102180, 64.72978607931611350, 1.270000000000006013 ) ) ;
#19591 = FACE_OUTER_BOUND ( 'NONE', #13528, .T. ) ;
#19592 = CARTESIAN_POINT ( 'NONE',  ( -5.477793340596218918, 31.72728063616241201, 0.5271671279843670455 ) ) ;
#19593 = ADVANCED_FACE ( 'NONE', ( #34245 ), #28475, .T. ) ;
#19594 = CARTESIAN_POINT ( 'NONE',  ( 8.132787923797314633, 122.8458379852381910, -0.04721391815988586205 ) ) ;
#19595 = ORIENTED_EDGE ( 'NONE', *, *, #35747, .T. ) ;
#19596 = CARTESIAN_POINT ( 'NONE',  ( 0.4875792343844080889, 105.8266127453845229, 5.318343663435395996 ) ) ;
#19597 = ADVANCED_FACE ( 'NONE', ( #1667 ), #41479, .F. ) ;
#19598 = FACE_OUTER_BOUND ( 'NONE', #38991, .T. ) ;
#19599 = EDGE_CURVE ( 'NONE', #2172, #1729, #31867, .T. ) ;
#19600 = CARTESIAN_POINT ( 'NONE',  ( -58.59897934080984783, -0.2308949485120836975, 0.4634499375557190048 ) ) ;
#19601 = FACE_OUTER_BOUND ( 'NONE', #38840, .T. ) ;
#19602 = CARTESIAN_POINT ( 'NONE',  ( 16.84917212821870436, 155.2300590059875844, 0.1976545469556810486 ) ) ;
#19603 = CARTESIAN_POINT ( 'NONE',  ( -5.362262919127019245, 116.9387654363850260, 0.7435593652664854725 ) ) ;
#19604 = CARTESIAN_POINT ( 'NONE',  ( -4.855449335888874174, 115.6909491485452719, 1.281272725539412294 ) ) ;
#19605 = CARTESIAN_POINT ( 'NONE',  ( 4.114294302962228755, -10.72644468530807416, -2.136776772127288559 ) ) ;
#19606 = CARTESIAN_POINT ( 'NONE',  ( -4.370579818869743782, 31.84755045023585751, 0.2525336677614991032 ) ) ;
#19607 = CARTESIAN_POINT ( 'NONE',  ( 1.153229101628888476, 158.8088198215516229, 1.472604719115123029 ) ) ;
#19608 = CARTESIAN_POINT ( 'NONE',  ( 3.547999066118234346, 14.38381850277834317, -2.990331240093012877 ) ) ;
#19609 = CARTESIAN_POINT ( 'NONE',  ( -3.468545696377880461, 29.88095345675903403, -7.690089085670218871 ) ) ;
#19610 = CARTESIAN_POINT ( 'NONE',  ( 8.739301385803836197, 118.0314441295146679, -0.4462037359528160940 ) ) ;
#19611 = CARTESIAN_POINT ( 'NONE',  ( -0.5453179846285600707, 107.9696733310005214, -4.488644025489748834 ) ) ;
#19612 = CIRCLE ( 'NONE', #34602, 6.985000000000000320 ) ;
#19613 = CARTESIAN_POINT ( 'NONE',  ( -11.53797084252497207, 82.58007221317646440, -1.269999999999999796 ) ) ;
#19614 = CARTESIAN_POINT ( 'NONE',  ( -2.188542869591966866, 104.6144662015456959, 4.302051086437162830 ) ) ;
#19615 = CARTESIAN_POINT ( 'NONE',  ( -1.287880193524239658, 20.15907059199006923, -4.440276399826991849 ) ) ;
#19616 = CARTESIAN_POINT ( 'NONE',  ( -46.95911617132933458, 24.98948415085536823, -1.986615011824472088 ) ) ;
#19617 = CYLINDRICAL_SURFACE ( 'NONE', #18490, 13.46199999999999442 ) ;
#19618 = CARTESIAN_POINT ( 'NONE',  ( 2.858040400949144022, -14.78363303536489681, 4.300485631455113200 ) ) ;
#19619 = CARTESIAN_POINT ( 'NONE',  ( 2.994815693583348537, 122.7580772961051707, -0.09506955764664386244 ) ) ;
#19620 = CARTESIAN_POINT ( 'NONE',  ( -9.680782865131792647, 118.1749183431956425, 0.3159967629729718008 ) ) ;
#19621 = EDGE_LOOP ( 'NONE', ( #408, #28008, #39738, #2399, #2844 ) ) ;
#19622 = DIRECTION ( 'NONE',  ( -1.000000000000000000, 0.000000000000000000, -9.769962616701377556E-15 ) ) ;
#19623 = ORIENTED_EDGE ( 'NONE', *, *, #22899, .F. ) ;
#19624 = CARTESIAN_POINT ( 'NONE',  ( 16.60960244842765832, -1.680552189788819435E-15, 2.034089647357696937E-15 ) ) ;
#19625 = CARTESIAN_POINT ( 'NONE',  ( 5.114706464973534317, -15.35711304900182128, 3.188446684335360271 ) ) ;
#19626 = CARTESIAN_POINT ( 'NONE',  ( -2.272333812996736757, 118.4336326928681729, 0.6977090181727383378 ) ) ;
#19627 = CARTESIAN_POINT ( 'NONE',  ( 21.87215423617511334, 148.4185114426368841, -1.275166548224078822 ) ) ;
#19628 = CARTESIAN_POINT ( 'NONE',  ( 4.574821423538755205, -2.080616851812391310, 0.6590154617212384824 ) ) ;
#19629 = CARTESIAN_POINT ( 'NONE',  ( -58.52079444616499870, -0.06495539389881313519, -0.6452041206688503561 ) ) ;
#19630 = EDGE_CURVE ( 'NONE', #40413, #20535, #3512, .T. ) ;
#19631 = ORIENTED_EDGE ( 'NONE', *, *, #5496, .T. ) ;
#19632 = CARTESIAN_POINT ( 'NONE',  ( 0.02009831008142323738, 106.6745790697264056, 5.014625686322316866 ) ) ;
#19633 =( LENGTH_UNIT ( ) NAMED_UNIT ( * ) SI_UNIT ( .MILLI., .METRE. ) );
#19634 = CARTESIAN_POINT ( 'NONE',  ( -11.98504388954668087, 126.0992317015783328, 1.027991910846090207 ) ) ;
#19635 = CARTESIAN_POINT ( 'NONE',  ( -6.573280687130626123E-14, 88.99346620154574339, 1.699031322814114629E-29 ) ) ;
#19636 = AXIS2_PLACEMENT_3D ( 'NONE', #19247, #9462, #38235 ) ;
#19637 = ADVANCED_FACE ( 'NONE', ( #22063 ), #20473, .F. ) ;
#19638 = CARTESIAN_POINT ( 'NONE',  ( 8.477251816686347752, 120.7201681212196291, -1.097727670418841450 ) ) ;
#19639 = CIRCLE ( 'NONE', #20302, 0.5080000000000010063 ) ;
#19640 = CARTESIAN_POINT ( 'NONE',  ( -6.881618033700713788, 158.0090104422344268, -1.782742279240755456 ) ) ;
#19641 = CARTESIAN_POINT ( 'NONE',  ( -58.73801720703743001, -0.4998429216807459552, -0.2437502737749605297 ) ) ;
#19642 = ORIENTED_EDGE ( 'NONE', *, *, #2183, .T. ) ;
#19643 = CARTESIAN_POINT ( 'NONE',  ( 4.505706913051673368, 118.1291065022491154, -0.5122133236055396166 ) ) ;
#19644 = CARTESIAN_POINT ( 'NONE',  ( 1.542034982439605795, 120.6610732671444595, -0.2472410911860530025 ) ) ;
#19645 = ORIENTED_EDGE ( 'NONE', *, *, #25329, .F. ) ;
#19646 = CARTESIAN_POINT ( 'NONE',  ( -4.277613954752526482, 119.9149831030956932, -0.8793409099722718780 ) ) ;
#19647 = CARTESIAN_POINT ( 'NONE',  ( 3.848634119772940565, -15.36481979860233871, 1.996958912074897396 ) ) ;
#19648 = FACE_OUTER_BOUND ( 'NONE', #1217, .T. ) ;
#19649 = EDGE_CURVE ( 'NONE', #17215, #26023, #40247, .T. ) ;
#19650 = CARTESIAN_POINT ( 'NONE',  ( -41.41491986784954804, 22.70581808553406233, -6.121743196690467558E-15 ) ) ;
#19651 = CARTESIAN_POINT ( 'NONE',  ( -4.820374670814820739, 117.7660393779071057, 0.8433105318405139661 ) ) ;
#19652 = CARTESIAN_POINT ( 'NONE',  ( 10.79589323670136736, 123.3109526380878833, 1.504350731661494134 ) ) ;
#19653 = CARTESIAN_POINT ( 'NONE',  ( -2.742835824903626207, 31.05151501484152732, 0.8589415642670262807 ) ) ;
#19654 = EDGE_CURVE ( 'NONE', #31005, #14016, #2138, .T. ) ;
#19655 = CARTESIAN_POINT ( 'NONE',  ( 4.300553167417687561, 27.50566818391071422, -1.719522505244270860 ) ) ;
#19656 = CARTESIAN_POINT ( 'NONE',  ( 8.534567384671277068, 123.3353292868209365, 0.2519373819028137285 ) ) ;
#19657 = AXIS2_PLACEMENT_3D ( 'NONE', #25555, #31530, #21927 ) ;
#19659 = VERTEX_POINT ( 'NONE', #34871 ) ;
#19658 = CARTESIAN_POINT ( 'NONE',  ( -45.58494389689084869, 18.10922195552001313, -7.361215080689235889E-15 ) ) ;
#19660 = VECTOR ( 'NONE', #25551, 1000.000000000000000 ) ;
#19661 = CARTESIAN_POINT ( 'NONE',  ( 5.564123858037556936, 116.7166602743764514, -0.04122317672195889571 ) ) ;
#19662 = CARTESIAN_POINT ( 'NONE',  ( -17.14499999999999957, 71.11999999999999034, 5.016499999999999737 ) ) ;
#19663 = CARTESIAN_POINT ( 'NONE',  ( -46.75016890987451035, 25.87258681965687757, -1.401816643053204414 ) ) ;
#19664 = CARTESIAN_POINT ( 'NONE',  ( -36.98328822617348521, 27.82293856516311692, 1.523999999999995580 ) ) ;
#19665 = FACE_OUTER_BOUND ( 'NONE', #2343, .T. ) ;
#19666 = FACE_OUTER_BOUND ( 'NONE', #39504, .T. ) ;
#19667 = DIRECTION ( 'NONE',  ( 0.01997839162482749689, 1.040247600000945640E-18, -0.9998004120163610509 ) ) ;
#19668 = DIRECTION ( 'NONE',  ( 0.6825627711659328911, 0.7308269722843309113, 2.299753143848213649E-16 ) ) ;
#19669 = CARTESIAN_POINT ( 'NONE',  ( -54.68578128245503223, 13.03233524004687638, -1.048863621890573067E-14 ) ) ;
#19670 = CARTESIAN_POINT ( 'NONE',  ( -57.50953982388014651, 1.662011999372992044, 1.631050346940570384 ) ) ;
#19671 = CARTESIAN_POINT ( 'NONE',  ( -5.719359222665208797, 159.1232349745254453, 0.1048325176007954412 ) ) ;
#19672 = ORIENTED_EDGE ( 'NONE', *, *, #8114, .T. ) ;
#19673 = CARTESIAN_POINT ( 'NONE',  ( -50.58128808078254934, 18.64259194233895656, -3.042287330737940110 ) ) ;
#19674 = CARTESIAN_POINT ( 'NONE',  ( -6.052889781086392418, 121.4336901549234113, -0.1296568525282296436 ) ) ;
#19675 = EDGE_LOOP ( 'NONE', ( #3438, #12530, #20853, #7964 ) ) ;
#19676 = CARTESIAN_POINT ( 'NONE',  ( 3.566795953268722563, 115.7029539211179667, -1.489760979346105518 ) ) ;
#19677 = CARTESIAN_POINT ( 'NONE',  ( -9.190025975546058490, 124.2403664864748549, -0.2180328680397457530 ) ) ;
#19678 = CARTESIAN_POINT ( 'NONE',  ( 2.294645149923727701, -15.44887909491890454, 5.922367448919703570 ) ) ;
#19679 = CARTESIAN_POINT ( 'NONE',  ( -16.31190729917925708, 125.3309463260932830, 1.192360770973151851 ) ) ;
#19680 = CARTESIAN_POINT ( 'NONE',  ( 5.153324091224940950, 56.51694919289779051, -4.640537933338372945 ) ) ;
#19681 = CARTESIAN_POINT ( 'NONE',  ( 13.50792085693134048, 119.6474162840860771, 0.5731308571144442254 ) ) ;
#19682 = DIRECTION ( 'NONE',  ( -4.017660918040594346E-17, 1.000000000000000000, 2.376309959284834438E-19 ) ) ;
#19683 = CARTESIAN_POINT ( 'NONE',  ( 5.267996062361754994, 115.6909491485453145, -0.8700017381306309749 ) ) ;
#19684 = CARTESIAN_POINT ( 'NONE',  ( -0.9401033786448180773, 4.191251494893229790, 0.2723526238743522732 ) ) ;
#19685 = CARTESIAN_POINT ( 'NONE',  ( -16.23049043870597075, 121.3954344197762083, -0.4305223454732413080 ) ) ;
#19686 = CARTESIAN_POINT ( 'NONE',  ( -48.10788822079490501, 19.08060971762839486, -5.220410434069243877 ) ) ;
#19687 = DIRECTION ( 'NONE',  ( 9.627370216492862708E-17, 1.000000000000000000, -0.000000000000000000 ) ) ;
#19688 = CARTESIAN_POINT ( 'NONE',  ( 2.553816101320873333, 116.8400682929857481, 0.5498680602850822829 ) ) ;
#19689 = ORIENTED_EDGE ( 'NONE', *, *, #26485, .F. ) ;
#19690 = CARTESIAN_POINT ( 'NONE',  ( -17.20821608673157144, 140.2562023718666353, 1.644530994948828928 ) ) ;
#19691 = CARTESIAN_POINT ( 'NONE',  ( -58.37015987205347045, -0.2922188715788874291, -0.003179148003318876120 ) ) ;
#19692 = CARTESIAN_POINT ( 'NONE',  ( 21.44537552191012608, 145.9698620541949765, 2.253500464710097795 ) ) ;
#19693 = CARTESIAN_POINT ( 'NONE',  ( 0.4598942929538996638, 118.4074432378348689, -0.5883637925338033314 ) ) ;
#19694 = CARTESIAN_POINT ( 'NONE',  ( 0.4369565669422456611, 1.205365006982008547, 0.8739355888918843851 ) ) ;
#19695 = CARTESIAN_POINT ( 'NONE',  ( -16.77501307560222799, 125.2521365416322254, -1.703383479906432685 ) ) ;
#19696 = CARTESIAN_POINT ( 'NONE',  ( 4.742695500909063000, 117.8453989086928004, -0.8301742325441545667 ) ) ;
#19697 = CARTESIAN_POINT ( 'NONE',  ( 6.329649118423095189, 120.0627515544778134, 0.4542292512502630886 ) ) ;
#19698 = AXIS2_PLACEMENT_3D ( 'NONE', #7369, #20538, #39965 ) ;
#19699 = CARTESIAN_POINT ( 'NONE',  ( 10.18692116311725648, 123.6566696788710686, -0.8138387218406052392 ) ) ;
#19700 = CARTESIAN_POINT ( 'NONE',  ( -9.108749339472550943, 153.9337724597031070, -0.1375672075132167438 ) ) ;
#19701 = VERTEX_POINT ( 'NONE', #5704 ) ;
#19702 = CARTESIAN_POINT ( 'NONE',  ( -14.41820472940927900, 152.7616507467334372, -2.289036833064873822 ) ) ;
#19703 = ADVANCED_FACE ( 'NONE', ( #18662 ), #36171, .T. ) ;
#19705 = CARTESIAN_POINT ( 'NONE',  ( 5.825557336981400880, -14.92341722037543406, 1.564612827344095569 ) ) ;
#19704 = CIRCLE ( 'NONE', #13575, 0.5080000000000002292 ) ;
#19706 = CARTESIAN_POINT ( 'NONE',  ( -4.769585057922912874, 31.49133049583777932, -0.6989730246579993755 ) ) ;
#19707 = EDGE_CURVE ( 'NONE', #37417, #10059, #29314, .T. ) ;
#19708 = CARTESIAN_POINT ( 'NONE',  ( -48.59875010875282442, 18.41211343146811785, -5.165832069028398088 ) ) ;
#19709 = ORIENTED_EDGE ( 'NONE', *, *, #13629, .T. ) ;
#19710 = CARTESIAN_POINT ( 'NONE',  ( 14.47078677760122467, 128.5519869857110393, 2.060874889273090815 ) ) ;
#19711 = CARTESIAN_POINT ( 'NONE',  ( 0.2924095564367995559, 116.4254662015451913, 0.005843038833677049321 ) ) ;
#19712 = CARTESIAN_POINT ( 'NONE',  ( -3.568793996894023657, 120.2162445758188056, 0.3416935720284705602 ) ) ;
#19713 = CARTESIAN_POINT ( 'NONE',  ( 8.348643983786249834, 26.63118458923209175, 1.112826146890550483 ) ) ;
#19714 = CARTESIAN_POINT ( 'NONE',  ( 1.635131992100914200, 156.2910218135955631, 0.4893959945316868065 ) ) ;
#19715 = CARTESIAN_POINT ( 'NONE',  ( 21.45272375726293035, 151.3201912522522719, -0.6338752469853822236 ) ) ;
#19716 = CYLINDRICAL_SURFACE ( 'NONE', #12442, 9.048749999999998295 ) ;
#19717 = CARTESIAN_POINT ( 'NONE',  ( -6.583861033951825950E-14, 91.02546620154572565, 1.480257718193877056E-29 ) ) ;
#19718 = TOROIDAL_SURFACE ( 'NONE', #7501, 5.080000000000005400, 0.5080000000000000071 ) ;
#19719 = CARTESIAN_POINT ( 'NONE',  ( -22.83607019214389666, 150.4065277667444036, -0.4307393832409497914 ) ) ;
#19720 = ORIENTED_EDGE ( 'NONE', *, *, #27160, .F. ) ;
#19721 = CARTESIAN_POINT ( 'NONE',  ( 8.032207078087980179, 121.5191168587267185, -0.8512761726684724417 ) ) ;
#19722 = CARTESIAN_POINT ( 'NONE',  ( 2.081416901521091933, -15.50639809317535089, 5.943648939154567934 ) ) ;
#19723 = CARTESIAN_POINT ( 'NONE',  ( -1.635131992101042986, 156.2910218135955631, -0.4893959945316865845 ) ) ;
#19724 = CARTESIAN_POINT ( 'NONE',  ( 4.304563788583176454, -12.55325912034982494, 2.095985231258857162 ) ) ;
#19725 = CARTESIAN_POINT ( 'NONE',  ( 23.29144772315967771, 149.3526176766912101, 0.4654185560736371352 ) ) ;
#19726 = ORIENTED_EDGE ( 'NONE', *, *, #1086, .T. ) ;
#19727 = CARTESIAN_POINT ( 'NONE',  ( 2.801506786573456420, 9.139157206818806500, -3.684590140147142368 ) ) ;
#19728 = CARTESIAN_POINT ( 'NONE',  ( 4.623799210569877083, 105.1214572271058785, 2.682504979537780443 ) ) ;
#19729 = CARTESIAN_POINT ( 'NONE',  ( -4.801687489738192482, 117.4019780203432646, 1.015655943361054581 ) ) ;
#19730 = CARTESIAN_POINT ( 'NONE',  ( 1.332716859069107315E-15, 13.84300000000000352, 0.000000000000000000 ) ) ;
#19731 = CARTESIAN_POINT ( 'NONE',  ( 5.918055438912293909, 120.3534538399959786, 1.025969926474026517 ) ) ;
#19732 = CARTESIAN_POINT ( 'NONE',  ( 0.1277143096572389558, 15.67076514537015974, -4.628409624684062251 ) ) ;
#19733 = CARTESIAN_POINT ( 'NONE',  ( 4.843103592331835294, 117.3073154462328063, 0.6875571908837337931 ) ) ;
#19734 = CARTESIAN_POINT ( 'NONE',  ( -48.99983924688925185, 17.84334367881515604, -5.121602422839403701 ) ) ;
#19736 = CARTESIAN_POINT ( 'NONE',  ( 18.63828149932687595, 131.8045874826418071, -1.403896228398082036 ) ) ;
#19735 = FACE_OUTER_BOUND ( 'NONE', #5743, .T. ) ;
#19737 = CARTESIAN_POINT ( 'NONE',  ( 3.490194016315742331, 12.22236127277748174, 3.029891289224248219 ) ) ;
#19738 = CARTESIAN_POINT ( 'NONE',  ( -14.11323155926173456, 120.5239346615589540, -1.094216903015625020 ) ) ;
#19739 = AXIS2_PLACEMENT_3D ( 'NONE', #23826, #1281, #24040 ) ;
#19740 = VERTEX_POINT ( 'NONE', #41904 ) ;
#19741 = B_SPLINE_CURVE_WITH_KNOTS ( 'NONE', 3,
 ( #20442, #11288, #1519, #20653 ),
 .UNSPECIFIED., .F., .F.,
 ( 4, 4 ),
 ( 0.000000000000000000, 0.5643836377221602696 ),
 .UNSPECIFIED. ) ;
#19742 = CARTESIAN_POINT ( 'NONE',  ( -15.80820582674417274, 146.9282941555416073, 0.1367419433413215590 ) ) ;
#19743 = CARTESIAN_POINT ( 'NONE',  ( 6.341500637990160172, -13.03620802017263536, 0.6512942508830525945 ) ) ;
#19744 = TOROIDAL_SURFACE ( 'NONE', #44, 0.3809999999999993947, 0.2540000000000000036 ) ;
#19745 = DIRECTION ( 'NONE',  ( 5.188838149069472160E-16, -1.699382548006136559E-16, -1.000000000000000000 ) ) ;
#19746 = EDGE_CURVE ( 'NONE', #28439, #4652, #35293, .T. ) ;
#19747 = VERTEX_POINT ( 'NONE', #19502 ) ;
#19748 = CARTESIAN_POINT ( 'NONE',  ( 16.71878049915325448, 131.5287050380659082, 2.312093064668929721 ) ) ;
#19749 = CARTESIAN_POINT ( 'NONE',  ( 4.897655256226133069, 56.53910281269273241, 5.081330806033577119 ) ) ;
#19750 = DIRECTION ( 'NONE',  ( -0.9998004120163608288, 0.000000000000000000, -0.01997839162482750383 ) ) ;
#19751 = CARTESIAN_POINT ( 'NONE',  ( -22.27630879610708803, 150.1947564971097222, 0.7286472789443333431 ) ) ;
#19752 = CARTESIAN_POINT ( 'NONE',  ( 1.824569540066833584, 15.47196788996624583, -8.237246883284143451 ) ) ;
#19753 = CARTESIAN_POINT ( 'NONE',  ( 23.08840689075971753, 149.5685596498530288, -0.1330139495868549737 ) ) ;
#19754 = CARTESIAN_POINT ( 'NONE',  ( -5.941785709847915875, 56.51500000000976343, -5.016499812912763367 ) ) ;
#19755 = CARTESIAN_POINT ( 'NONE',  ( -18.35410564743290607, 77.35382415001784295, -5.016499999999999737 ) ) ;
#19756 = CARTESIAN_POINT ( 'NONE',  ( -47.16890147375944764, 22.20336809214633433, 4.187060126831872786 ) ) ;
#19757 = VECTOR ( 'NONE', #3321, 1000.000000000000114 ) ;
#19758 = CARTESIAN_POINT ( 'NONE',  ( 2.209012367505132080, -15.11364764369361957, 5.670533105609369073 ) ) ;
#19759 = CARTESIAN_POINT ( 'NONE',  ( -54.47970570282438274, 8.083255770631444292, 3.476097746275891076 ) ) ;
#19760 = CARTESIAN_POINT ( 'NONE',  ( -5.078986093043185157, 75.78546620154573077, -0.1014902294541231847 ) ) ;
#19761 = CARTESIAN_POINT ( 'NONE',  ( -4.473658520889312484, 118.1283618854176893, 0.5455511291602485047 ) ) ;
#19762 = CARTESIAN_POINT ( 'NONE',  ( -58.37241122568489970, -0.2962816677228030660, -1.024972700666444124E-14 ) ) ;
#19763 = B_SPLINE_SURFACE_WITH_KNOTS ( 'NONE', 3, 3, ( 
 ( #28769, #41781, #19173, #18539, #32179, #15346, #25157, #12784, #38158 ),
 ( #3011, #15970, #5372, #7254, #3856, #38993, #6823, #35801, #6408 ),
 ( #20010, #33240, #23405, #29179, #22769, #6615, #3427, #39845, #7043 ),
 ( #16392, #29398, #33027, #13214, #26838, #237, #20214, #19792, #26196 ),
 ( #19377, #17028, #867, #4069, #16176, #32383, #13630, #32812, #39201 ),
 ( #36009, #10009, #22982, #26620, #661, #36435, #26, #23187, #3643 ),
 ( #16607, #29615, #36222, #451, #32593, #12990, #13422, #26410, #25985 ),
 ( #39415, #13840, #10217, #30027, #16821, #19583, #22561, #10434, #29823 ),
 ( #39629, #35591, #3214, #9802, #1708, #40678, #23834, #34288, #30444 ),
 ( #21054, #27047, #8288, #30235, #36641, #20843, #1498, #33868, #24254 ),
 ( #40055, #40269, #4698, #17862, #34080, #17652, #11065, #1074, #30862 ),
 ( #30654, #20632, #14043, #17445, #24048, #10848, #33449, #14246, #1911 ),
 ( #11470, #37063, #7673, #21258, #24459, #7880, #1288, #27253, #36855 ),
 ( #14455, #14662, #37464, #33660, #5116, #27467, #40477, #4907, #4485 ),
 ( #11269, #7463, #37262, #8081, #27667, #18069, #31071, #14873, #27875 ),
 ( #10641, #23621, #20422, #4278, #17240, #12324, #31706, #21885, #25312 ),
 ( #11686, #34491, #41726, #38317, #8920, #5527, #34913, #9136, #8712 ),
 ( #28510, #41518, #12531, #21674, #18696, #5744, #31490, #12111, #41094 ),
 ( #37681, #15082, #2755, #8503, #11901, #18484, #2548, #40884, #18909 ),
 ( #28083, #41306, #24890, #21460, #37887, #22095, #15712, #35122, #18275 ),
 ( #34698, #2335, #24672, #5949, #15509, #15294, #28299, #31920, #25101 ),
 ( #28715, #5322, #31276, #38104, #2119, #37182, #23965, #14170, #27586 ),
 ( #17989, #28001, #30986, #36984, #7803, #4414, #14791, #2037, #37387 ),
 ( #30776, #33996, #20765, #40595, #10982, #37594, #4826, #14581, #5238 ),
 ( #20552, #33790, #34204, #18193, #8420, #1211, #4618, #17573, #30577 ),
 ( #21176, #20975, #1416, #14372, #5031, #27383, #41010, #40393, #21378 ),
 ( #11187, #34404, #33581, #31194, #15002, #11818, #30362, #17371, #27794 ),
 ( #24171, #27174, #8004, #17778, #1626, #40802, #11603, #36773, #40187 ),
 ( #11395, #24381, #8204, #1827, #24587, #7590, #34831, #15216, #31627 ) ),
 .UNSPECIFIED., .F., .F., .F.,
 ( 4, 1, 1, 1, 1, 1, 1, 2, 1, 1, 1, 1, 1, 1, 1, 1, 1, 1, 1, 1, 1, 1, 1, 1, 1, 4 ),
 ( 4, 1, 1, 1, 1, 1, 4 ),
 ( 0.000000000000000000, 0.03307066603948304734, 0.06614133207896609468, 0.09921199811844919059, 0.1653533301974152714, 0.1984239962368983812, 0.2314946622763813522, 0.2645653283158643787, 0.3105299952961229071, 0.3564946622763812689, 0.4024593292566397418, 0.4484239962368982702, 0.5403533301974150493, 0.6322826641579321061, 0.7242119981184491628, 0.7701766650987074136, 0.8161413320789658865, 0.8850883325493537068, 0.8965794992944182695, 0.9080706660394826102, 0.9195618327845473949, 0.9310529995296121797, 0.9425441662746769644, 0.9540353330197415271, 0.9770176665098706525, 1.000000000000000000 ),
 ( 0.000000000000000000, 0.2500000000000000000, 0.4444444444444445308, 0.5000000000000000000, 0.7500000000000000000, 0.8333333333333333703, 1.000000000000000000 ),
 .UNSPECIFIED. ) ;
#19764 = ORIENTED_EDGE ( 'NONE', *, *, #30849, .F. ) ;
#19765 = ORIENTED_EDGE ( 'NONE', *, *, #15940, .T. ) ;
#19766 = CARTESIAN_POINT ( 'NONE',  ( -1.565525540593865950, 118.7629491485440099, -1.245867024842673532 ) ) ;
#19767 = CARTESIAN_POINT ( 'NONE',  ( 6.175143553146828168, 119.5953855062382871, -1.005919626096980490 ) ) ;
#19768 = CARTESIAN_POINT ( 'NONE',  ( -6.465481721428130157, 120.6581566633936404, -0.3941859656685692270 ) ) ;
#19770 = CARTESIAN_POINT ( 'NONE',  ( 4.512464582872506291, 118.1196997639598862, 0.6561311196536673274 ) ) ;
#19769 = AXIS2_PLACEMENT_3D ( 'NONE', #40895, #15307, #2766 ) ;
#19771 = CARTESIAN_POINT ( 'NONE',  ( -46.67763236942723637, 26.04755295256607539, -0.6632588273528947642 ) ) ;
#19772 = CARTESIAN_POINT ( 'NONE',  ( -10.02582114772209287, 123.8737202207250618, -1.106617482833785804 ) ) ;
#19773 = DIRECTION ( 'NONE',  ( -6.829619984160660610E-15, 0.000000000000000000, -1.000000000000000000 ) ) ;
#19774 = DIRECTION ( 'NONE',  ( -0.8745520943968241312, 0.4849315768086548406, -5.691349986800536046E-16 ) ) ;
#19775 = CARTESIAN_POINT ( 'NONE',  ( 7.304536785993802184, 123.0387167848234355, 0.07720001398428681660 ) ) ;
#19776 = CARTESIAN_POINT ( 'NONE',  ( -15.81386139960078197, 149.2064892436030163, -1.885719434888957657 ) ) ;
#19777 =( LENGTH_UNIT ( ) NAMED_UNIT ( * ) SI_UNIT ( .MILLI., .METRE. ) );
#19778 = CARTESIAN_POINT ( 'NONE',  ( -0.0005468344959711694646, 156.3034662015456604, 0.02736583427618486872 ) ) ;
#19779 = CARTESIAN_POINT ( 'NONE',  ( 7.966529119766866174, 121.8269078720123701, -0.7202784793015850617 ) ) ;
#19780 = CARTESIAN_POINT ( 'NONE',  ( -7.045758995674062497, 122.0730845715159063, -0.06312930854005696646 ) ) ;
#19781 = EDGE_CURVE ( 'NONE', #20726, #10933, #7180, .T. ) ;
#19782 = CARTESIAN_POINT ( 'NONE',  ( 4.219463811995017188, -1.205994944679912306, -1.932895124392335573 ) ) ;
#19783 = CARTESIAN_POINT ( 'NONE',  ( 15.01050271945730863, 120.7699597703182945, 0.9001124940000719832 ) ) ;
#19784 = CARTESIAN_POINT ( 'NONE',  ( 5.586884702347362897, 130.0144662015457300, 0.1116392523995368424 ) ) ;
#19785 = CARTESIAN_POINT ( 'NONE',  ( 1.871808270187516943, -15.45276866356297418, 5.379583495939216142 ) ) ;
#19786 = CARTESIAN_POINT ( 'NONE',  ( -0.5002616235673846834, 119.0154928070276412, 0.5875571981567379032 ) ) ;
#19787 = CARTESIAN_POINT ( 'NONE',  ( -0.8879284396340286767, 8.347861319067646946, 0.4041202799994399464 ) ) ;
#19788 = CARTESIAN_POINT ( 'NONE',  ( -1.889792677999466486, 116.7132768022172797, -0.3078404110637329993 ) ) ;
#19789 = CARTESIAN_POINT ( 'NONE',  ( 0.8148283262528154269, -11.57344599616632763, 0.5628321559398594687 ) ) ;
#19790 = ORIENTED_EDGE ( 'NONE', *, *, #25853, .T. ) ;
#19791 = EDGE_CURVE ( 'NONE', #37473, #10724, #8937, .T. ) ;
#19792 = CARTESIAN_POINT ( 'NONE',  ( -43.13073682054399427, 20.84535665847942454, 0.1327613832363976898 ) ) ;
#19793 = CARTESIAN_POINT ( 'NONE',  ( 1.237704251691374546, 106.3840144300045409, 5.116357776886615305 ) ) ;
#19794 = CARTESIAN_POINT ( 'NONE',  ( 0.000000000000000000, 0.000000000000000000, 0.000000000000000000 ) ) ;
#19795 = CARTESIAN_POINT ( 'NONE',  ( -14.11809548624358435, 150.3034377993741657, 0.8008162161465686157 ) ) ;
#19796 = CARTESIAN_POINT ( 'NONE',  ( 4.273959209556542405, -12.80518358089995168, 2.504334382443756724 ) ) ;
#19797 = CARTESIAN_POINT ( 'NONE',  ( 2.082154424532988379, 156.9412006218898057, -1.407003841209468531 ) ) ;
#19798 = CARTESIAN_POINT ( 'NONE',  ( -9.988019213705189969, 120.6268241347409855, -1.591717657363032723 ) ) ;
#19799 = DIRECTION ( 'NONE',  ( 0.000000000000000000, 0.000000000000000000, 1.000000000000000000 ) ) ;
#19800 = AXIS2_PLACEMENT_3D ( 'NONE', #31760, #2603, #6206 ) ;
#19801 = EDGE_CURVE ( 'NONE', #40534, #5419, #39328, .T. ) ;
#19802 = CARTESIAN_POINT ( 'NONE',  ( 1.854781166956293248, -15.20994639552496253, 5.427130820981656001 ) ) ;
#19803 = CARTESIAN_POINT ( 'NONE',  ( -0.02863553844924360964, 38.94824868342700341, -0.3880333552236577277 ) ) ;
#19804 = CARTESIAN_POINT ( 'NONE',  ( 15.79043079689192552, 145.9231181611787918, 0.08479106802855336522 ) ) ;
#19805 = ORIENTED_EDGE ( 'NONE', *, *, #40737, .F. ) ;
#19806 = CARTESIAN_POINT ( 'NONE',  ( -6.135835944515187101, 77.40800365160224317, -1.523999999999996247 ) ) ;
#19807 = DIRECTION ( 'NONE',  ( -4.017660918040594346E-17, 1.000000000000000000, 2.376309959284834438E-19 ) ) ;
#19808 = AXIS2_PLACEMENT_3D ( 'NONE', #28680, #6743, #10135 ) ;
#19809 = CARTESIAN_POINT ( 'NONE',  ( 11.04921058900168873, 56.51500000000000057, -4.436160551868584712 ) ) ;
#19810 = CARTESIAN_POINT ( 'NONE',  ( -5.028575548160166164, 117.3993840946898075, 0.6249845981789815541 ) ) ;
#19811 = EDGE_CURVE ( 'NONE', #37552, #15033, #3562, .T. ) ;
#19812 = CARTESIAN_POINT ( 'NONE',  ( 17.22554230343049397, 122.7389118244895769, 0.2345756144184562297 ) ) ;
#19813 = CARTESIAN_POINT ( 'NONE',  ( -0.3655860903869697087, 105.8811906981200934, 5.329044222542315801 ) ) ;
#19814 = AXIS2_PLACEMENT_3D ( 'NONE', #26495, #8891, #25071 ) ;
#19815 = CARTESIAN_POINT ( 'NONE',  ( -4.758926732810884630, 118.7629491485454309, 0.8043858395770803194 ) ) ;
#19816 = DIRECTION ( 'NONE',  ( -5.188838149069471174E-16, 1.699382548006136313E-16, 1.000000000000000000 ) ) ;
#19817 = CARTESIAN_POINT ( 'NONE',  ( -3.688991022714105839, 31.45506795701765412, -0.1149108006718590896 ) ) ;
#19818 = CARTESIAN_POINT ( 'NONE',  ( 21.10215338253914297, 147.9292434580435724, 2.361242315759021437 ) ) ;
#19819 = CARTESIAN_POINT ( 'NONE',  ( -1.792273654952471595, 16.32048121479114045, -4.264856162967389785 ) ) ;
#19820 = CARTESIAN_POINT ( 'NONE',  ( -6.340062920055459017, 30.52953040661039807, -5.581008500864042432 ) ) ;
#19821 = CARTESIAN_POINT ( 'NONE',  ( -8.714206658535026406, 118.0327614349573366, -0.7961205384438058141 ) ) ;
#19822 = CARTESIAN_POINT ( 'NONE',  ( -0.7330347863451183166, 118.7604188656930120, -0.9075975635256806617 ) ) ;
#19823 = CARTESIAN_POINT ( 'NONE',  ( -27.88833342972739615, 78.11058938209563962, -1.524000000000007571 ) ) ;
#19824 = TOROIDAL_SURFACE ( 'NONE', #41633, 17.68910244842765778, 0.6350000000000000089 ) ;
#19825 = FACE_OUTER_BOUND ( 'NONE', #39004, .T. ) ;
#19826 = CARTESIAN_POINT ( 'NONE',  ( -1.280342683972266693, 105.1232991681604858, 5.188841635131638874 ) ) ;
#19827 = VECTOR ( 'NONE', #26496, 1000.000000000000227 ) ;
#19828 = CARTESIAN_POINT ( 'NONE',  ( -1.178223178616622402, 14.53665720681882689, 4.476207649055042204 ) ) ;
#19829 = CARTESIAN_POINT ( 'NONE',  ( 4.784930192204152277, 117.3993836135881708, 1.202631631483913832 ) ) ;
#19830 = DIRECTION ( 'NONE',  ( -1.000000000000000000, 9.563967653961371147E-17, 0.000000000000000000 ) ) ;
#19831 = CARTESIAN_POINT ( 'NONE',  ( 1.826496821415126037, -15.21410320048187437, 5.439012564009855666 ) ) ;
#19832 = EDGE_CURVE ( 'NONE', #22759, #30779, #38201, .T. ) ;
#19833 = CARTESIAN_POINT ( 'NONE',  ( 1.604275531929067578, 118.9836165220538504, -0.7112099450351575536 ) ) ;
#19834 = CIRCLE ( 'NONE', #3551, 0.2539999999999998925 ) ;
#19835 = CARTESIAN_POINT ( 'NONE',  ( -13.14342457437329159, 119.8381915656929380, 0.4562891928474253067 ) ) ;
#19836 = CYLINDRICAL_SURFACE ( 'NONE', #10826, 0.2539999999999967839 ) ;
#19837 = VERTEX_POINT ( 'NONE', #23107 ) ;
#19838 = LINE ( 'NONE', #32426, #27059 ) ;
#19839 = VERTEX_POINT ( 'NONE', #6120 ) ;
#19840 = LINE ( 'NONE', #16219, #2253 ) ;
#19841 = CARTESIAN_POINT ( 'NONE',  ( 3.255875469058810978, -15.74984210207193414, 5.086368125509904026 ) ) ;
#19842 = CARTESIAN_POINT ( 'NONE',  ( -20.17730036299085938, 147.7236477000422497, 1.702857440531004407 ) ) ;
#19843 = CARTESIAN_POINT ( 'NONE',  ( 4.934953413367771269, 117.8999350694477926, -0.7268823312289467431 ) ) ;
#19844 = EDGE_CURVE ( 'NONE', #11444, #11585, #9605, .T. ) ;
#19845 = CARTESIAN_POINT ( 'NONE',  ( 0.9647673288271847447, 27.50405299253531410, 0.1566625405351598777 ) ) ;
#19846 = CARTESIAN_POINT ( 'NONE',  ( -58.64513978733522492, -0.3133698122888631810, -0.3358519082774775733 ) ) ;
#19847 = ORIENTED_EDGE ( 'NONE', *, *, #42058, .F. ) ;
#19848 = CARTESIAN_POINT ( 'NONE',  ( -4.848458278871826010, 117.4106395692391516, -1.171953005487281096 ) ) ;
#19849 = CARTESIAN_POINT ( 'NONE',  ( 0.9570916872344990001, 123.2612876230388395, 0.1732974146428332418 ) ) ;
#19850 = CARTESIAN_POINT ( 'NONE',  ( 4.961775220622199889, 117.4031003928707548, 1.033713290510416716 ) ) ;
#19851 = CARTESIAN_POINT ( 'NONE',  ( -12.98740932513253554, 152.2092440956282076, 1.257387005612584874 ) ) ;
#19852 = CARTESIAN_POINT ( 'NONE',  ( -4.962228733194765873, 117.4031047975369404, -1.033509257472498444 ) ) ;
#19853 = CARTESIAN_POINT ( 'NONE',  ( 11.64084037886360257, 123.0696236843973281, -1.242201319703144069 ) ) ;
#19854 = CARTESIAN_POINT ( 'NONE',  ( -4.023942337083176390, 118.1249481555716301, -0.9214969356372303411 ) ) ;
#19855 = CARTESIAN_POINT ( 'NONE',  ( -58.24002838079472610, 0.001074765447070524793, -0.6562585879479864159 ) ) ;
#19856 = ORIENTED_EDGE ( 'NONE', *, *, #4596, .T. ) ;
#19857 = CARTESIAN_POINT ( 'NONE',  ( 4.464715371412748546, 118.1580834965288318, -0.4253963240309212024 ) ) ;
#19858 = CARTESIAN_POINT ( 'NONE',  ( 8.002172173406759015, 154.6030710842251494, -0.4507127070663226043 ) ) ;
#19859 = ORIENTED_EDGE ( 'NONE', *, *, #852, .F. ) ;
#19860 = CARTESIAN_POINT ( 'NONE',  ( -12.10021064141429292, 153.5325627063460843, -2.025425248842403825 ) ) ;
#19861 = CARTESIAN_POINT ( 'NONE',  ( 3.411744169395244164, -14.91921274028452871, 2.011823270444000666 ) ) ;
#19862 = CARTESIAN_POINT ( 'NONE',  ( -5.145869062083050061, 105.1220833959279730, -1.445893102178412715 ) ) ;
#19863 = AXIS2_PLACEMENT_3D ( 'NONE', #18150, #33531, #4782 ) ;
#19864 = DIRECTION ( 'NONE',  ( -9.627370216492862708E-17, -1.000000000000000000, 0.000000000000000000 ) ) ;
#19865 = EDGE_CURVE ( 'NONE', #12920, #38620, #32300, .T. ) ;
#19866 = CARTESIAN_POINT ( 'NONE',  ( -3.254339884055971854, 0.1279812147911008058, 3.287934741457726684 ) ) ;
#19867 = CARTESIAN_POINT ( 'NONE',  ( 10.41670863957350512, 122.9580799906392343, 1.467069541016857048 ) ) ;
#19868 = CARTESIAN_POINT ( 'NONE',  ( -2.394634909045491700, 30.36160847033138310, 1.723844942078720521 ) ) ;
#19869 = CARTESIAN_POINT ( 'NONE',  ( 4.622858883031034871, 26.85595184169372374, 0.2084198311932836112 ) ) ;
#19870 = CARTESIAN_POINT ( 'NONE',  ( 9.185235947232817111, 124.1858035287836231, 0.2689572614166577114 ) ) ;
#19871 = CARTESIAN_POINT ( 'NONE',  ( -4.026309595109284878, 109.3894556192956173, 3.506482798589841465 ) ) ;
#19872 = CIRCLE ( 'NONE', #12418, 3.683000000000001162 ) ;
#19873 = EDGE_CURVE ( 'NONE', #10519, #34270, #17769, .T. ) ;
#19874 = CARTESIAN_POINT ( 'NONE',  ( -51.26804087848103819, 14.04722136430348201, -4.535752393750718703 ) ) ;
#19875 = CARTESIAN_POINT ( 'NONE',  ( -14.60500000000000043, 71.11999999999999034, -5.016499999999999737 ) ) ;
#19876 = CARTESIAN_POINT ( 'NONE',  ( 13.85159022459153988, 16.51000000000000156, 5.016499999999999737 ) ) ;
#19877 = CARTESIAN_POINT ( 'NONE',  ( -46.63124922200988465, 26.12666050884489977, -1.285908859455852316 ) ) ;
#19878 = CARTESIAN_POINT ( 'NONE',  ( -29.16381924947294024, 66.91553870234344004, -1.270000000000006013 ) ) ;
#19879 = DIRECTION ( 'NONE',  ( -0.01997839162482737546, -1.040247600000940825E-18, 0.9998004120163610509 ) ) ;
#19880 = DIRECTION ( 'NONE',  ( 0.1469470846586743706, 9.335746474409589170E-17, -0.9891443546370348727 ) ) ;
#19881 = CARTESIAN_POINT ( 'NONE',  ( -4.074955089416341991, 118.2429491485453354, 0.1454234154749719787 ) ) ;
#19882 = DIRECTION ( 'NONE',  ( 0.2290273297124658103, -0.9734199927291290466, 2.580167833703409551E-15 ) ) ;
#19883 = CARTESIAN_POINT ( 'NONE',  ( -57.38748718130355542, 3.645894598607590797, 1.236217348619458090 ) ) ;
#19884 = CARTESIAN_POINT ( 'NONE',  ( -57.36719850051837000, 1.975114663830185302, 1.756955940785651871 ) ) ;
#19885 = CARTESIAN_POINT ( 'NONE',  ( -2.784667331447816974, 116.5968896900294709, 0.09290643507641029031 ) ) ;
#19886 = ORIENTED_EDGE ( 'NONE', *, *, #1448, .T. ) ;
#19887 = CARTESIAN_POINT ( 'NONE',  ( -52.19327494808134560, 16.79818233314609444, -2.080405417473095930 ) ) ;
#19888 = CARTESIAN_POINT ( 'NONE',  ( -7.789722586531418358, 122.5884748538522047, -0.3097450211583079316 ) ) ;
#19889 = EDGE_CURVE ( 'NONE', #16174, #30132, #26637, .T. ) ;
#19890 = ORIENTED_EDGE ( 'NONE', *, *, #34191, .F. ) ;
#19891 = CARTESIAN_POINT ( 'NONE',  ( -17.14500000000466784, 71.11999999999886768, 1.523999999999998689 ) ) ;
#19892 = CARTESIAN_POINT ( 'NONE',  ( -5.974701571114539256, 155.3719879121972838, -0.2191910023528569340 ) ) ;
#19893 = CARTESIAN_POINT ( 'NONE',  ( 6.387155697962850986, -12.89254730397265725, 0.3290856906432634288 ) ) ;
#19894 = CARTESIAN_POINT ( 'NONE',  ( -2.167900391131186044, 117.8876587302075194, 0.6265904732959522994 ) ) ;
#19895 = CARTESIAN_POINT ( 'NONE',  ( -4.598301960400187127, 22.30806413504685537, 0.5496829067130363233 ) ) ;
#19896 = CARTESIAN_POINT ( 'NONE',  ( 8.021187395864771474, 158.6806155330135084, 0.3964977924059487346 ) ) ;
#19897 = EDGE_CURVE ( 'NONE', #17342, #34427, #38698, .T. ) ;
#19898 = CARTESIAN_POINT ( 'NONE',  ( 9.420913146467203347, 124.7671794033526851, 0.3269489669365729934 ) ) ;
#19899 = CARTESIAN_POINT ( 'NONE',  ( 4.847733185841858194, 115.6909491485453145, -1.282834277461510908 ) ) ;
#19900 = CARTESIAN_POINT ( 'NONE',  ( 0.5139362334885246852, 0.5165572279304807557, -0.8313783143454911428 ) ) ;
#19901 = CARTESIAN_POINT ( 'NONE',  ( -23.34743456777632531, 142.7586093370927074, -0.6964168797349270523 ) ) ;
#19902 = CARTESIAN_POINT ( 'NONE',  ( 5.305748947172212127, 57.14999999999999858, -5.247078976224250013 ) ) ;
#19903 = DIRECTION ( 'NONE',  ( 0.000000000000000000, 0.000000000000000000, 1.000000000000000000 ) ) ;
#19904 = ORIENTED_EDGE ( 'NONE', *, *, #39123, .T. ) ;
#19905 = CARTESIAN_POINT ( 'NONE',  ( -2.274883502654467815, 116.3490410268270665, 0.1699064989630479361 ) ) ;
#19906 = ORIENTED_EDGE ( 'NONE', *, *, #14373, .T. ) ;
#19907 = CARTESIAN_POINT ( 'NONE',  ( -15.87040186760635407, 150.9007765090757971, 1.629155861667390903 ) ) ;
#19908 = CARTESIAN_POINT ( 'NONE',  ( -57.92645925829798159, 0.6640176851100348943, -0.9534638877764777254 ) ) ;
#19909 = CARTESIAN_POINT ( 'NONE',  ( 9.146501239663530569, 119.1751624949753534, 1.313831160619747473 ) ) ;
#19910 = CARTESIAN_POINT ( 'NONE',  ( 19.88689915616616233, 147.6055923437354238, -1.726923636697636377 ) ) ;
#19911 = CARTESIAN_POINT ( 'NONE',  ( -0.2316695588195925026, 0.1309245165040176240, 0.9467938775014126396 ) ) ;
#19912 = CARTESIAN_POINT ( 'NONE',  ( -21.80375291804149285, 148.4185114426368841, -2.147915116047498962 ) ) ;
#19913 = CARTESIAN_POINT ( 'NONE',  ( 4.667063153570271794, 118.0255431904385404, -0.5722037917038420574 ) ) ;
#19914 = CARTESIAN_POINT ( 'NONE',  ( 6.530233653228945556, 120.6338824379019172, 0.3959831657380196712 ) ) ;
#19915 = VECTOR ( 'NONE', #23796, 1000.000000000000000 ) ;
#19916 = CARTESIAN_POINT ( 'NONE',  ( 17.03225580939797013, 146.4457527449227143, -1.249628170391535509 ) ) ;
#19917 = CARTESIAN_POINT ( 'NONE',  ( -8.041889123127157646, 122.8518031662551948, -0.1606960833125205546 ) ) ;
#19918 = ORIENTED_EDGE ( 'NONE', *, *, #86, .T. ) ;
#19919 = CARTESIAN_POINT ( 'NONE',  ( -11.93340282868953750, 123.0912118827050108, -1.763528850166467210 ) ) ;
#19920 = CARTESIAN_POINT ( 'NONE',  ( 5.059117473032719303, -15.50674158137822722, 2.046454293345789655 ) ) ;
#19921 = CARTESIAN_POINT ( 'NONE',  ( -10.18297664959815663, 77.66688486464208552, 1.524000000000001354 ) ) ;
#19922 = CARTESIAN_POINT ( 'NONE',  ( -4.596595486785018281, 117.9777161510301227, -0.9190962615854699758 ) ) ;
#19923 = CARTESIAN_POINT ( 'NONE',  ( -47.35944255389382107, 21.37623662739424191, -4.722871667523179440 ) ) ;
#19924 = CARTESIAN_POINT ( 'NONE',  ( 4.145420271487251895, 118.2391365653420650, 0.3994957887817748299 ) ) ;
#19925 = CARTESIAN_POINT ( 'NONE',  ( 0.9182646862278995847, 157.4778559999684830, 1.599919928990593210 ) ) ;
#19926 = CARTESIAN_POINT ( 'NONE',  ( -0.01249116623180958861, 38.87185441664305330, -1.227828225846576693 ) ) ;
#19927 = CIRCLE ( 'NONE', #28100, 0.2539999999999966729 ) ;
#19928 = CARTESIAN_POINT ( 'NONE',  ( 15.19604463793433169, 156.0859089222169587, 0.3036531364422415669 ) ) ;
#19929 = VECTOR ( 'NONE', #23396, 1000.000000000000000 ) ;
#19930 = CARTESIAN_POINT ( 'NONE',  ( -0.3027292972884025324, 105.9597790263619146, 5.298406829468305546 ) ) ;
#19931 = CARTESIAN_POINT ( 'NONE',  ( -8.379105243356219646, 21.88232641057985361, -0.8402904295462267914 ) ) ;
#19932 = CARTESIAN_POINT ( 'NONE',  ( 13.78138926674702525, 150.2278160098252329, 0.9796190600867308307 ) ) ;
#19933 = EDGE_CURVE ( 'NONE', #40718, #30484, #42114, .T. ) ;
#19934 = CARTESIAN_POINT ( 'NONE',  ( 1.373401713467732543, 159.5224216140176168, -0.5650407700211931283 ) ) ;
#19935 = CYLINDRICAL_SURFACE ( 'NONE', #28764, 0.6350000000000014522 ) ;
#19936 = CARTESIAN_POINT ( 'NONE',  ( -58.36937220204561072, -0.2906615202371656270, 0.02563298686227328746 ) ) ;
#19937 = CIRCLE ( 'NONE', #4972, 0.3809999999999977849 ) ;
#19938 = CARTESIAN_POINT ( 'NONE',  ( -16.30362368704351539, 121.4145675751456253, -0.3085868453551564583 ) ) ;
#19939 = VERTEX_POINT ( 'NONE', #39119 ) ;
#19940 = CARTESIAN_POINT ( 'NONE',  ( -7.964318472288553608, 121.6586585215090679, -1.114152107595608676 ) ) ;
#19941 = CARTESIAN_POINT ( 'NONE',  ( 6.373744154335938994, -13.69897431215970052, 0.7397752478428293310 ) ) ;
#19942 = CARTESIAN_POINT ( 'NONE',  ( -7.868938471672525026, 154.6027768716304820, -0.5345728592648680833 ) ) ;
#19943 = CARTESIAN_POINT ( 'NONE',  ( 2.810721824165392846, -14.60963343767143741, 5.218503737131710452 ) ) ;
#19944 = CARTESIAN_POINT ( 'NONE',  ( -14.20701772348855130, 121.1589565784038456, 0.8306491748466006131 ) ) ;
#19945 = CARTESIAN_POINT ( 'NONE',  ( -41.26650596300343921, 23.23696532716408925, 1.523999999999985366 ) ) ;
#19946 = CARTESIAN_POINT ( 'NONE',  ( 13.67522198567651515, 119.6429072192227494, 0.3220992662749119217 ) ) ;
#19947 = EDGE_CURVE ( 'NONE', #21011, #15945, #21662, .T. ) ;
#19948 = ORIENTED_EDGE ( 'NONE', *, *, #10800, .F. ) ;
#19949 = CARTESIAN_POINT ( 'NONE',  ( 4.114294302962228755, -10.72644468530807416, -2.136776772127288559 ) ) ;
#19950 = CARTESIAN_POINT ( 'NONE',  ( 4.033169965737029017, 105.1222026749920246, 3.507333144493335109 ) ) ;
#19951 = CARTESIAN_POINT ( 'NONE',  ( 14.80692295515832058, 78.04183178746350791, 5.016499999999999737 ) ) ;
#19952 = DIRECTION ( 'NONE',  ( -1.000000000000000000, 9.627370216492861475E-17, 0.000000000000000000 ) ) ;
#19953 = CARTESIAN_POINT ( 'NONE',  ( 8.178139910812117108, 120.5865972341469359, 1.415288944234376345 ) ) ;
#19954 = CARTESIAN_POINT ( 'NONE',  ( 4.382351430540762927, 4.226039240006542741, -1.512498627010908647 ) ) ;
#19955 = CARTESIAN_POINT ( 'NONE',  ( 17.71751426720048173, 153.9999837190418930, 1.728000864493653976 ) ) ;
#19956 = CARTESIAN_POINT ( 'NONE',  ( -6.631541954483209765E-14, 98.39146620154573952, -1.863789202389766375E-18 ) ) ;
#19957 = CARTESIAN_POINT ( 'NONE',  ( 19.75353020121325187, 136.1149058410947532, -1.478659091479562759 ) ) ;
#19958 = AXIS2_PLACEMENT_3D ( 'NONE', #16802, #25755, #19773 ) ;
#19959 = CARTESIAN_POINT ( 'NONE',  ( -2.651420880294951488, 7.049774601622781134, -3.792306073587544901 ) ) ;
#19960 = CARTESIAN_POINT ( 'NONE',  ( -0.9938236163261908729, 116.9791385580615781, -0.3849800449318573348 ) ) ;
#19961 = VERTEX_POINT ( 'NONE', #32089 ) ;
#19962 = CYLINDRICAL_SURFACE ( 'NONE', #14358, 0.6349999999999966782 ) ;
#19963 = AXIS2_PLACEMENT_3D ( 'NONE', #9919, #34866, #18867 ) ;
#19964 = CARTESIAN_POINT ( 'NONE',  ( -9.835128631862042781, 124.8790005272986861, 0.1409026022053574689 ) ) ;
#19965 = CARTESIAN_POINT ( 'NONE',  ( 3.036109343602874322, -15.28514977651167150, 5.695352409590039855 ) ) ;
#19966 = DIRECTION ( 'NONE',  ( 0.9454731675810359448, -0.3256999990547780333, 5.459396135145339171E-16 ) ) ;
#19967 = AXIS2_PLACEMENT_3D ( 'NONE', #5295, #8892, #34885 ) ;
#19968 = CARTESIAN_POINT ( 'NONE',  ( 3.198224922426783579, -14.19254063666773291, 2.189163805996276579 ) ) ;
#19969 = ORIENTED_EDGE ( 'NONE', *, *, #433, .T. ) ;
#19970 = CARTESIAN_POINT ( 'NONE',  ( 17.77132669990250236, 135.5811125208551857, 2.431814553008901481 ) ) ;
#19971 = DIRECTION ( 'NONE',  ( 0.7071067811865473507, -0.7071067811865477948, 0.000000000000000000 ) ) ;
#19972 = CIRCLE ( 'NONE', #9104, 0.2539999999999991709 ) ;
#19973 = CARTESIAN_POINT ( 'NONE',  ( 7.869802931801260115, 122.7053923345152953, 0.1572573916674578076 ) ) ;
#19974 = CARTESIAN_POINT ( 'NONE',  ( -9.582280438405419432, 118.3624989119526418, 0.5072503739029416980 ) ) ;
#19975 = CARTESIAN_POINT ( 'NONE',  ( 6.480130183504051011, 21.94006803110874415, 5.378050974841823262 ) ) ;
#19976 = CARTESIAN_POINT ( 'NONE',  ( 3.247806582136902431, 159.4494809562368971, -0.3030341850868439324 ) ) ;
#19977 = CARTESIAN_POINT ( 'NONE',  ( -5.706393392231406736, 57.14999999999999147, -5.041882957777242602 ) ) ;
#19978 = AXIS2_PLACEMENT_3D ( 'NONE', #9279, #22237, #35265 ) ;
#19979 = CARTESIAN_POINT ( 'NONE',  ( -46.72764730961441160, 25.92641697299453440, 1.373594020054483167 ) ) ;
#19980 = CARTESIAN_POINT ( 'NONE',  ( -48.34142060212426628, 20.97662605846759831, 3.847193496378342736 ) ) ;
#19981 = CARTESIAN_POINT ( 'NONE',  ( -4.937777651546055857, 117.4065511353899041, -1.082295458227385154 ) ) ;
#19982 = CARTESIAN_POINT ( 'NONE',  ( -54.77668461537430034, 8.146287316968315650, 3.518595155146524434 ) ) ;
#19983 = CARTESIAN_POINT ( 'NONE',  ( -58.69929992858412504, -0.3146504455105202935, 0.2902061446857141513 ) ) ;
#19984 = CARTESIAN_POINT ( 'NONE',  ( -4.402139039590816871, 118.1614230090776800, 0.4936525752913482057 ) ) ;
#19985 = CARTESIAN_POINT ( 'NONE',  ( -5.299459906814613319, 78.93540349268876355, -5.255323016343699472 ) ) ;
#19986 = ORIENTED_EDGE ( 'NONE', *, *, #2083, .F. ) ;
#19987 = CARTESIAN_POINT ( 'NONE',  ( -43.87210973174860129, 22.05421410453335795, 2.454571855453426377 ) ) ;
#19988 = CARTESIAN_POINT ( 'NONE',  ( 3.904474273848753008, 119.0221123855851033, -0.7730353223355832526 ) ) ;
#19989 = CARTESIAN_POINT ( 'NONE',  ( -6.266908424742289263, 120.0898888515776264, -0.4521870875522996380 ) ) ;
#19990 = CARTESIAN_POINT ( 'NONE',  ( 4.516265718371130333, 118.0894310158977021, 0.7770291299768713467 ) ) ;
#19991 = CARTESIAN_POINT ( 'NONE',  ( -15.03094698176529853, 148.9283877096812034, -1.255086756411655902 ) ) ;
#19992 = CIRCLE ( 'NONE', #25451, 0.8889999999999984581 ) ;
#19993 = DIRECTION ( 'NONE',  ( 1.000000000000000000, 0.000000000000000000, -3.414809992080326065E-16 ) ) ;
#19994 = CARTESIAN_POINT ( 'NONE',  ( 1.586608521452973486, 106.2379067940291293, -5.113598281387616851 ) ) ;
#19995 = CARTESIAN_POINT ( 'NONE',  ( -17.21112184089944463, 146.3482411845097886, -2.056990446313781362 ) ) ;
#19996 = DIRECTION ( 'NONE',  ( -0.9998004120163610509, -4.016384292689131511E-17, -0.01997839162482749689 ) ) ;
#19997 = LINE ( 'NONE', #16808, #24434 ) ;
#19998 = CARTESIAN_POINT ( 'NONE',  ( 8.614520148390900189, 118.6763556054874158, -0.8198081090887602285 ) ) ;
#19999 = CARTESIAN_POINT ( 'NONE',  ( -14.67652612023663039, 148.8571924874472074, -0.2271985726276186113 ) ) ;
#20000 = CARTESIAN_POINT ( 'NONE',  ( -4.399545650080316506, 2.442302885307133131, -1.471791394725966873 ) ) ;
#20001 = CARTESIAN_POINT ( 'NONE',  ( 13.14908049612667185, 156.9583929045107595, 0.9825115876436357754 ) ) ;
#20002 = CARTESIAN_POINT ( 'NONE',  ( -6.451606698686837575E-14, 65.62546620154573418, 4.217636114931141265E-29 ) ) ;
#20003 = CARTESIAN_POINT ( 'NONE',  ( 3.118150858982619233, -14.63350761981947734, -0.02509704758125085033 ) ) ;
#20004 = CIRCLE ( 'NONE', #25462, 0.3810000000000015041 ) ;
#20005 = CARTESIAN_POINT ( 'NONE',  ( -18.96108613168469503, 147.8663216482595146, 1.723626476717959433 ) ) ;
#20006 = CARTESIAN_POINT ( 'NONE',  ( -0.08600706866453224075, 15.02498995931601122, -0.9728917428382349852 ) ) ;
#20007 = CARTESIAN_POINT ( 'NONE',  ( -18.42221188220390360, 125.1790410860780298, -0.8413473246917883008 ) ) ;
#20008 = CARTESIAN_POINT ( 'NONE',  ( -0.4650136207426652235, -7.476398416381191403, -0.8572754866018892361 ) ) ;
#20009 = ORIENTED_EDGE ( 'NONE', *, *, #32940, .F. ) ;
#20010 = CARTESIAN_POINT ( 'NONE',  ( -41.87797633265722652, 22.30863410810708558, 1.617563149257729815 ) ) ;
#20011 = CARTESIAN_POINT ( 'NONE',  ( 7.563243396832008081, 124.2956292408697863, 0.1602470646927417752 ) ) ;
#20012 = CARTESIAN_POINT ( 'NONE',  ( -9.482824821900010193, 153.9068681542131856, 0.6648444853843686886 ) ) ;
#20013 = CARTESIAN_POINT ( 'NONE',  ( 4.284293204009990141, -11.98693494109343050, 1.176118521537933725 ) ) ;
#20014 = CARTESIAN_POINT ( 'NONE',  ( 17.71558884668061751, 147.6919162452172145, -1.529690151225475470 ) ) ;
#20015 = CIRCLE ( 'NONE', #8447, 0.2540000000000023350 ) ;
#20016 = CARTESIAN_POINT ( 'NONE',  ( -2.398927117899045225, 157.8629595415303584, -1.727538386417435179 ) ) ;
#20017 = CARTESIAN_POINT ( 'NONE',  ( 3.385259569132474944, 115.7029692307686162, 1.641278830299353508 ) ) ;
#20018 = CARTESIAN_POINT ( 'NONE',  ( 1.979733141779612016, -15.19599036556555660, 5.309005240801834447 ) ) ;
#20019 = CARTESIAN_POINT ( 'NONE',  ( -4.223161182163281957, 33.49016550088244060, 2.148155765408566342 ) ) ;
#20020 = CARTESIAN_POINT ( 'NONE',  ( 9.248842176949983340, 124.1957968681474824, 0.02334546025992364007 ) ) ;
#20021 = EDGE_LOOP ( 'NONE', ( #35424, #15424, #9736, #12734 ) ) ;
#20022 = CARTESIAN_POINT ( 'NONE',  ( -3.182864231321134163, 107.7307366742556667, 4.270808201732677389 ) ) ;
#20023 = CARTESIAN_POINT ( 'NONE',  ( 0.1816879500932431502, 105.8845321911205133, 5.338643427584144341 ) ) ;
#20024 = DIRECTION ( 'NONE',  ( 5.188838149069472160E-16, -1.699382548006136559E-16, -1.000000000000000000 ) ) ;
#20025 = CARTESIAN_POINT ( 'NONE',  ( -23.16987411132078734, 77.52691185402750307, 1.523999999999994470 ) ) ;
#20026 = CARTESIAN_POINT ( 'NONE',  ( 5.789608264049557640, 116.9447284183608389, 0.03249775470882608486 ) ) ;
#20027 = CARTESIAN_POINT ( 'NONE',  ( -5.317809737553872651, 116.7000894413872629, 0.8094161617621953297 ) ) ;
#20028 = CARTESIAN_POINT ( 'NONE',  ( -3.205472953781653533, 118.7629491485510442, 1.047959515690910060 ) ) ;
#20029 = CARTESIAN_POINT ( 'NONE',  ( 11.66725022230186859, 55.42194143536244155, 5.016499999999783910 ) ) ;
#20030 = CARTESIAN_POINT ( 'NONE',  ( -5.208405493689606480, 31.38331509014777154, -0.6716542322870746595 ) ) ;
#20031 = CARTESIAN_POINT ( 'NONE',  ( 2.699166815671171005, 158.5977336698458089, 1.597229775447004618 ) ) ;
#20032 = CARTESIAN_POINT ( 'NONE',  ( -0.9239673467531356321, 25.61616486456964736, -4.531977062890359065 ) ) ;
#20033 = CARTESIAN_POINT ( 'NONE',  ( -6.244303144875123834, 11.31477948022340208, -5.679040650537692692 ) ) ;
#20034 = CARTESIAN_POINT ( 'NONE',  ( -8.636847134335058129, 118.3872487031030403, -1.029711822167878710 ) ) ;
#20035 = CARTESIAN_POINT ( 'NONE',  ( -2.157690779482436927, 123.3349985135950959, -0.1620144005770981221 ) ) ;
#20036 = CARTESIAN_POINT ( 'NONE',  ( 4.847990641624395636, 117.4106256157386809, 1.172052288416076005 ) ) ;
#20037 = CARTESIAN_POINT ( 'NONE',  ( -10.96186877710187879, 56.39406130473896894, -5.016500000000648996 ) ) ;
#20038 = CARTESIAN_POINT ( 'NONE',  ( -1.157812389548250165, 104.6144662015456959, 4.694735647476201201 ) ) ;
#20039 = CARTESIAN_POINT ( 'NONE',  ( -4.374560056058969693, 13.03735028915297534, 1.504755201125916875 ) ) ;
#20040 = CARTESIAN_POINT ( 'NONE',  ( 14.60500000000000043, 71.11999999999999034, -5.016499999999999737 ) ) ;
#20041 = CARTESIAN_POINT ( 'NONE',  ( -3.168818291390510300, 117.3993833748032216, -1.398835752645559927 ) ) ;
#20042 = CARTESIAN_POINT ( 'NONE',  ( 3.066387819753066069, -14.51305101688413224, 3.912045622741378903 ) ) ;
#20043 = EDGE_CURVE ( 'NONE', #25505, #18759, #9507, .T. ) ;
#20044 = CARTESIAN_POINT ( 'NONE',  ( 2.578112510117919864, 120.6526784328644339, -0.3421008684282440537 ) ) ;
#20045 = CARTESIAN_POINT ( 'NONE',  ( -1.373401713467861329, 159.5224216140176168, 0.5650407700211933504 ) ) ;
#20046 = CARTESIAN_POINT ( 'NONE',  ( 4.828582363101557640, 117.4037123032867385, -1.009936161916218378 ) ) ;
#20047 = ORIENTED_EDGE ( 'NONE', *, *, #3768, .F. ) ;
#20048 = CARTESIAN_POINT ( 'NONE',  ( -11.43668055974971587, 78.14103736854400495, -1.523999999999999133 ) ) ;
#20049 = EDGE_LOOP ( 'NONE', ( #28692, #20637, #29346, #26461 ) ) ;
#20050 = CARTESIAN_POINT ( 'NONE',  ( -2.667392527469405916, 31.33771804890096746, 0.9893360403373154810 ) ) ;
#20051 = CARTESIAN_POINT ( 'NONE',  ( 3.166528004143551289, -15.72052770450255110, 4.635360722337766859 ) ) ;
#20052 = CARTESIAN_POINT ( 'NONE',  ( -20.46161261025647349, 147.6366098820875266, 1.667455336067830807 ) ) ;
#20053 = CARTESIAN_POINT ( 'NONE',  ( 9.254844111042901389, 119.0402042963619351, -0.8977872906997165225 ) ) ;
#20054 = CARTESIAN_POINT ( 'NONE',  ( 0.3093957028193324299, 29.65535775802675289, -0.9258560203679269129 ) ) ;
#20055 = CARTESIAN_POINT ( 'NONE',  ( -58.68693696493448186, -0.3142683078187059609, -0.3029362029564767189 ) ) ;
#20056 = VERTEX_POINT ( 'NONE', #6526 ) ;
#20057 = CARTESIAN_POINT ( 'NONE',  ( -58.36720124622751626, -0.2861505079054943446, -0.06388190288962447561 ) ) ;
#20058 = CARTESIAN_POINT ( 'NONE',  ( 0.8285762425323237590, 121.5536190086353372, 0.3701497059917960297 ) ) ;
#20059 = CARTESIAN_POINT ( 'NONE',  ( -3.514252322483388813, 120.2313485970928326, 0.5318214084310807221 ) ) ;
#20060 = CARTESIAN_POINT ( 'NONE',  ( -28.36525985791271154, 77.02308833105713859, 1.523999999999992028 ) ) ;
#20061 = CARTESIAN_POINT ( 'NONE',  ( 18.22365405440197250, 148.2327041560005512, -1.660465927639720229 ) ) ;
#20062 = CARTESIAN_POINT ( 'NONE',  ( -20.20973109032216541, 149.9354415288716780, -2.375026552130124369 ) ) ;
#20063 = CARTESIAN_POINT ( 'NONE',  ( -58.40597088826705630, 0.2738206778524349128, -0.9753506901443967925 ) ) ;
#20064 = VERTEX_POINT ( 'NONE', #32512 ) ;
#20065 = CARTESIAN_POINT ( 'NONE',  ( 4.463504259782801853, 118.1585507804028907, -0.4269113537636273770 ) ) ;
#20066 = CARTESIAN_POINT ( 'NONE',  ( 2.740744172220221042, 120.7841308545065431, -0.2151145298216794455 ) ) ;
#20067 = EDGE_LOOP ( 'NONE', ( #299, #26744, #37728, #9915 ) ) ;
#20068 = CARTESIAN_POINT ( 'NONE',  ( 3.261251233531137217, -14.70027692227136917, 2.623613175195522285 ) ) ;
#20069 = DIRECTION ( 'NONE',  ( -1.000000000000000000, 0.000000000000000000, 0.000000000000000000 ) ) ;
#20070 = ADVANCED_FACE ( 'NONE', ( #16310 ), #3485, .T. ) ;
#20071 = CARTESIAN_POINT ( 'NONE',  ( -58.35171525856283381, -0.2536858515840151318, 0.1680674994488967344 ) ) ;
#20072 = CARTESIAN_POINT ( 'NONE',  ( 1.583070580811935191, 1.852152477310867074, 4.353984577079609508 ) ) ;
#20073 = CARTESIAN_POINT ( 'NONE',  ( 5.838061318222974805, 120.4133487461328826, 1.005638731867922964 ) ) ;
#20074 = CARTESIAN_POINT ( 'NONE',  ( -2.525735733961075979, 30.63084530247838444, 1.130430605335521310 ) ) ;
#20075 = CARTESIAN_POINT ( 'NONE',  ( 4.087030650986479330, 6.990161447142720696, 2.163025551504125232 ) ) ;
#20076 = CARTESIAN_POINT ( 'NONE',  ( 9.099523502024073451, 123.9936668703698075, 0.3412791990392153307 ) ) ;
#20077 = DIRECTION ( 'NONE',  ( -1.000000000000000000, 0.000000000000000000, 0.000000000000000000 ) ) ;
#20078 = CARTESIAN_POINT ( 'NONE',  ( -54.82379132704179625, 7.242239488055856711, -3.238872252923487682 ) ) ;
#20079 = CARTESIAN_POINT ( 'NONE',  ( 8.797372769768484702, 117.7003220351452910, 0.04568619392659034606 ) ) ;
#20080 = CARTESIAN_POINT ( 'NONE',  ( -0.8290918312103936483, 117.3993839334940077, 1.455271914084780738 ) ) ;
#20081 = CARTESIAN_POINT ( 'NONE',  ( -46.84768978681289298, 25.58645032415531517, -1.575055156418467162 ) ) ;
#20082 = LINE ( 'NONE', #735, #17930 ) ;
#20083 = CARTESIAN_POINT ( 'NONE',  ( -29.67105550538132519, 68.29201113456635142, -1.524000000002203814 ) ) ;
#20084 = DIRECTION ( 'NONE',  ( 5.188838149069472160E-16, -1.699382548006136559E-16, -1.000000000000000000 ) ) ;
#20085 = CARTESIAN_POINT ( 'NONE',  ( -5.860205464924994168, 57.14999999999999147, 5.019550311879309668 ) ) ;
#20086 = DIRECTION ( 'NONE',  ( 0.9998004120163608288, 0.000000000000000000, 0.01997839162482736852 ) ) ;
#20087 = CARTESIAN_POINT ( 'NONE',  ( -58.50860430493788300, 0.7049166599848583070, 0.9756837515128382599 ) ) ;
#20088 = EDGE_CURVE ( 'NONE', #38242, #11659, #4685, .T. ) ;
#20089 = CARTESIAN_POINT ( 'NONE',  ( -56.34046819891496938, 4.202508019718290022, 2.501728563949842776 ) ) ;
#20090 = CARTESIAN_POINT ( 'NONE',  ( -21.84047376210821767, 151.4369626909183637, 0.009531295849831233555 ) ) ;
#20091 = VERTEX_POINT ( 'NONE', #10734 ) ;
#20092 = CARTESIAN_POINT ( 'NONE',  ( -57.34105142390577470, 4.241571993195747403, -0.1395372036360086054 ) ) ;
#20093 = CARTESIAN_POINT ( 'NONE',  ( 6.982279026085625340, 121.9522648198741024, 0.07242179238622248327 ) ) ;
#20094 = EDGE_LOOP ( 'NONE', ( #28306, #8507, #3469, #18281 ) ) ;
#20095 = DIRECTION ( 'NONE',  ( 0.7770581983690815209, -0.6294287539884060312, 5.101669463485828849E-16 ) ) ;
#20096 = CARTESIAN_POINT ( 'NONE',  ( -7.557080711912884219, 122.4263405438208991, -0.1815966937148653093 ) ) ;
#20097 = CARTESIAN_POINT ( 'NONE',  ( 5.816378023188423896, -13.23522671163289388, 2.128111738716565338 ) ) ;
#20098 = CARTESIAN_POINT ( 'NONE',  ( -14.09802512849282863, 121.9525460547650226, 1.083329899170117683 ) ) ;
#20099 = CARTESIAN_POINT ( 'NONE',  ( -0.3239230800893593276, 29.42979164457532804, -4.628216972995994993 ) ) ;
#20100 = CARTESIAN_POINT ( 'NONE',  ( 17.01700507317042366, 122.6950552906510694, 0.6769824155666206433 ) ) ;
#20101 = CARTESIAN_POINT ( 'NONE',  ( 10.90720410752496150, 127.9361718968202126, 0.3766330825069126864 ) ) ;
#20102 = CARTESIAN_POINT ( 'NONE',  ( 3.655561289726139140, 27.93047918286777076, -2.829280713513928180 ) ) ;
#20103 = CARTESIAN_POINT ( 'NONE',  ( -0.4866770014159069180, -4.230873095947595530, 0.8487236227246106601 ) ) ;
#20104 = CARTESIAN_POINT ( 'NONE',  ( -1.404208078696352002, 159.5982469381528972, -0.2156159867753335013 ) ) ;
#20105 = FACE_OUTER_BOUND ( 'NONE', #1333, .T. ) ;
#20106 = EDGE_CURVE ( 'NONE', #23143, #17488, #11458, .T. ) ;
#20107 = CARTESIAN_POINT ( 'NONE',  ( -6.654617103318593247E-14, 104.6144662015457243, 1.534725424433578570E-31 ) ) ;
#20108 = VERTEX_POINT ( 'NONE', #39515 ) ;
#20109 = CIRCLE ( 'NONE', #28264, 2.540000000000000480 ) ;
#20110 = CARTESIAN_POINT ( 'NONE',  ( 2.266257171229604683, 116.3486079626738530, 0.2607109679900413424 ) ) ;
#20111 = CARTESIAN_POINT ( 'NONE',  ( -17.98452544307437506, 146.6345634702618952, 1.580200905155535018 ) ) ;
#20112 = CARTESIAN_POINT ( 'NONE',  ( -57.39693641392964452, 1.805818221422732961, -1.488717331793851795 ) ) ;
#20113 = CARTESIAN_POINT ( 'NONE',  ( 11.86420439699943330, 156.4809912657682673, 1.954521554489341062 ) ) ;
#20114 = CARTESIAN_POINT ( 'NONE',  ( 15.53591925045075861, 153.1703808545849483, -1.736877461573578030 ) ) ;
#20115 = CARTESIAN_POINT ( 'NONE',  ( 0.9728917428133897483, -6.565010040704528649, -0.08600706860408523224 ) ) ;
#20116 = CARTESIAN_POINT ( 'NONE',  ( -14.28642979620163267, 121.5541609676003389, -1.504719748795722012 ) ) ;
#20117 = CARTESIAN_POINT ( 'NONE',  ( 4.672671725886756278, 117.9840379399288395, -0.6970879283291996353 ) ) ;
#20118 = CARTESIAN_POINT ( 'NONE',  ( 4.761265772527523588, 104.6144662015456959, 0.8484901397391942934 ) ) ;
#20119 = CARTESIAN_POINT ( 'NONE',  ( 6.676265340062377263, 155.5185402614932570, -1.076558685701346940 ) ) ;
#20120 = CARTESIAN_POINT ( 'NONE',  ( -6.500720044509902706, 121.7799842514348541, -0.1008652220075045153 ) ) ;
#20121 = EDGE_LOOP ( 'NONE', ( #29170, #23282 ) ) ;
#20122 = CARTESIAN_POINT ( 'NONE',  ( -2.275810046414789678, 157.5529522918930638, -1.704261365023472141 ) ) ;
#20123 = CARTESIAN_POINT ( 'NONE',  ( 3.858334187661429215, -15.75373651934012997, 4.144460154494749915 ) ) ;
#20124 = DIRECTION ( 'NONE',  ( 5.188838149069472160E-16, -1.699382548006136559E-16, -1.000000000000000000 ) ) ;
#20125 = CARTESIAN_POINT ( 'NONE',  ( -4.716528458602361695, 117.9480174125288414, -0.8296297511114593126 ) ) ;
#20126 = ADVANCED_FACE ( 'NONE', ( #29706 ), #41901, .T. ) ;
#20127 = CARTESIAN_POINT ( 'NONE',  ( -51.34009458250667279, 14.66650723912346699, -4.800162786360146150 ) ) ;
#20128 = CARTESIAN_POINT ( 'NONE',  ( 4.065926199369043204, 118.2429491485453354, 0.3080910687088499467 ) ) ;
#20129 = PRODUCT ( 'Center Spindle', 'Center Spindle', '', ( #20424 ) ) ;
#20130 = CARTESIAN_POINT ( 'NONE',  ( 9.734001924785392390, 155.3230018269108825, 2.058186707467866583 ) ) ;
#20131 = CARTESIAN_POINT ( 'NONE',  ( -4.834802360910630981, 32.27718159487177729, 0.9856153350916389000 ) ) ;
#20132 = ADVANCED_FACE ( 'NONE', ( #6171 ), #22528, .F. ) ;
#20133 = CARTESIAN_POINT ( 'NONE',  ( 1.798461198689400797, 116.4670535197835051, 0.02282230188723655823 ) ) ;
#20134 = EDGE_CURVE ( 'NONE', #30025, #37691, #10802, .T. ) ;
#20135 = CARTESIAN_POINT ( 'NONE',  ( 8.331117840153179799, 7.414970825009634225, 1.249357972265521255 ) ) ;
#20136 = CARTESIAN_POINT ( 'NONE',  ( 14.86280047924396008, 148.8756053271976327, 1.012714816113364780 ) ) ;
#20137 = CIRCLE ( 'NONE', #31025, 0.2539999999999993929 ) ;
#20138 = CARTESIAN_POINT ( 'NONE',  ( 1.353295744334168216, 159.4649289425152858, -0.7236632733165270226 ) ) ;
#20139 = CARTESIAN_POINT ( 'NONE',  ( -42.48565245465144358, 21.90714463913272780, -1.692305106577525198 ) ) ;
#20140 = ORIENTED_EDGE ( 'NONE', *, *, #15680, .F. ) ;
#20141 = CARTESIAN_POINT ( 'NONE',  ( 0.7582820727000408878, 118.7629491485454025, 1.270951156714173580 ) ) ;
#20142 = UNCERTAINTY_MEASURE_WITH_UNIT (LENGTH_MEASURE( 1.000000000000000082E-05 ), #38995, 'distance_accuracy_value', 'NONE');
#20143 = CARTESIAN_POINT ( 'NONE',  ( -15.48485754026178540, 120.7065362441885981, -0.2052890747276163996 ) ) ;
#20144 = EDGE_LOOP ( 'NONE', ( #39999, #18916, #4744, #35589 ) ) ;
#20145 = CARTESIAN_POINT ( 'NONE',  ( -7.924630949180505368, 121.8615034964088295, -1.018655858764297761 ) ) ;
#20146 = CARTESIAN_POINT ( 'NONE',  ( -46.48504882799048232, 25.86691234155827246, -1.524000000000011346 ) ) ;
#20147 = CARTESIAN_POINT ( 'NONE',  ( -9.187421481788835109, 153.8854248570426080, -0.5770480568347666761 ) ) ;
#20148 = CARTESIAN_POINT ( 'NONE',  ( 3.901187470525758094, -13.68826627043556776, 3.907672046116945186 ) ) ;
#20149 = CARTESIAN_POINT ( 'NONE',  ( -19.78757913416918868, 132.0165317526581816, 1.053352019815566587 ) ) ;
#20150 = CARTESIAN_POINT ( 'NONE',  ( -2.884051542275779756, 156.0957788938021054, -0.05763021347587621995 ) ) ;
#20151 = CARTESIAN_POINT ( 'NONE',  ( 5.755000932441415529, 159.1151184437813981, 0.1316611545253207338 ) ) ;
#20152 = EDGE_LOOP ( 'NONE', ( #18536, #11193, #3052, #11961 ) ) ;
#20153 = CARTESIAN_POINT ( 'NONE',  ( -4.187759052228169132, -5.978784877027076838, 2.003160513425938483 ) ) ;
#20154 = CARTESIAN_POINT ( 'NONE',  ( -3.284316801889665349, 105.1240599693624631, 4.214405307443403359 ) ) ;
#20155 = CARTESIAN_POINT ( 'NONE',  ( -4.825036788391023457, 51.14746620154573264, -0.09641571798141751470 ) ) ;
#20156 = DIRECTION ( 'NONE',  ( 0.6825627711659328911, 0.7308269722843309113, 2.299753143848213649E-16 ) ) ;
#20157 = CARTESIAN_POINT ( 'NONE',  ( -6.395303539164157947, 119.4668496938549396, 1.005475218501896251 ) ) ;
#20158 = CARTESIAN_POINT ( 'NONE',  ( -4.603752034695621553, -0.9465464349810851497, 0.4006815057252178236 ) ) ;
#20159 = CARTESIAN_POINT ( 'NONE',  ( 22.34269864632755898, 148.4347612714453248, 1.893969414928640793 ) ) ;
#20160 = CARTESIAN_POINT ( 'NONE',  ( -57.21909960282354035, 2.250382150496072597, -1.879871960369849271 ) ) ;
#20162 = CARTESIAN_POINT ( 'NONE',  ( 20.57754816582968260, 149.5144255282053223, -1.563875036196712420 ) ) ;
#20161 = DIRECTION ( 'NONE',  ( 5.188838149069472160E-16, -1.699382548006136559E-16, -1.000000000000000000 ) ) ;
#20163 = CARTESIAN_POINT ( 'NONE',  ( -2.587970193024280441, -12.16632112844677494, -3.833404006186521773 ) ) ;
#20164 = CARTESIAN_POINT ( 'NONE',  ( -1.336693583852524458, 159.4956652290339605, -0.6991310044172545091 ) ) ;
#20165 = VERTEX_POINT ( 'NONE', #39383 ) ;
#20166 = ADVANCED_FACE ( 'NONE', ( #10186 ), #13178, .T. ) ;
#20167 = CIRCLE ( 'NONE', #20830, 5.588000000000006295 ) ;
#20168 = CARTESIAN_POINT ( 'NONE',  ( -2.776805996813621391, 120.9068798055765370, 0.1259499506852534423 ) ) ;
#20169 = CARTESIAN_POINT ( 'NONE',  ( 3.435007001638270996, -15.26001923902611779, 5.499761658607620340 ) ) ;
#20170 = DIRECTION ( 'NONE',  ( -1.000000000000000000, -9.933992704233682996E-16, 0.000000000000000000 ) ) ;
#20171 = CARTESIAN_POINT ( 'NONE',  ( -4.679371059064479255, 111.8765634536042626, -2.628838740615948577 ) ) ;
#20172 = VERTEX_POINT ( 'NONE', #19140 ) ;
#20173 = CARTESIAN_POINT ( 'NONE',  ( 18.24829758291878434, 150.1405190176936344, 2.471583571221721343 ) ) ;
#20174 = DIRECTION ( 'NONE',  ( -0.8745520943968249084, 0.4849315768086533418, -5.311926654347176508E-16 ) ) ;
#20175 = DIRECTION ( 'NONE',  ( -5.206863593109713661E-17, 1.000000000000000000, -1.077750396879097183E-30 ) ) ;
#20176 = AXIS2_PLACEMENT_3D ( 'NONE', #8774, #12387, #21314 ) ;
#20177 = CARTESIAN_POINT ( 'NONE',  ( -22.59368173950844749, 146.4122051224262577, 0.8656317577275310926 ) ) ;
#20178 = ADVANCED_FACE ( 'NONE', ( #19343 ), #16730, .T. ) ;
#20179 = CARTESIAN_POINT ( 'NONE',  ( 7.154006291674216200, 2.952895779142483246, 4.500751621275830061 ) ) ;
#20180 = CARTESIAN_POINT ( 'NONE',  ( 0.5759676376929014907, 120.3589971203204669, 0.3694376532493068854 ) ) ;
#20181 = EDGE_CURVE ( 'NONE', #38422, #33761, #27130, .T. ) ;
#20182 = CARTESIAN_POINT ( 'NONE',  ( 22.98897055778763132, 149.8455236008688303, -0.1339715990509169341 ) ) ;
#20183 = CARTESIAN_POINT ( 'NONE',  ( -57.92213827294109763, 0.6733716272070394693, 0.9587715765150526259 ) ) ;
#20184 = CARTESIAN_POINT ( 'NONE',  ( -48.05879467440716013, 25.10120116127142964, 0.1605504162684488478 ) ) ;
#20185 = CARTESIAN_POINT ( 'NONE',  ( -56.04137470801128273, 5.508142037592367757, 2.879222540163115074 ) ) ;
#20186 = CARTESIAN_POINT ( 'NONE',  ( -57.60563996024792743, 1.910284663404326233, 1.727869274997176907 ) ) ;
#20187 = CARTESIAN_POINT ( 'NONE',  ( -4.493393903509352860, 118.1153619691203573, 0.5661490535317686978 ) ) ;
#20188 = CARTESIAN_POINT ( 'NONE',  ( -58.37241122568488549, -0.2962816677227753104, -1.028586707908062104E-14 ) ) ;
#20189 = AXIS2_PLACEMENT_3D ( 'NONE', #15378, #15163, #28170 ) ;
#20190 = ORIENTED_EDGE ( 'NONE', *, *, #11811, .T. ) ;
#20191 = CARTESIAN_POINT ( 'NONE',  ( -45.45367893016184979, 22.54667639846615046, 3.012003376585078662 ) ) ;
#20192 = CARTESIAN_POINT ( 'NONE',  ( -3.944803911500280869, 119.0966328791857762, -0.9223804097932700730 ) ) ;
#20193 = CARTESIAN_POINT ( 'NONE',  ( -5.244916502329433960, 116.2229785614576798, -1.177106425564501402 ) ) ;
#20194 = CARTESIAN_POINT ( 'NONE',  ( 4.491034488983506101, 118.0837758977322238, 0.7972306053495301637 ) ) ;
#20195 = CARTESIAN_POINT ( 'NONE',  ( -15.74774640517369662, 148.1776054874778197, -1.420244701258233988 ) ) ;
#20196 = CARTESIAN_POINT ( 'NONE',  ( -0.5744809549289578987, 115.7029491485453292, -1.760674903347913212 ) ) ;
#20197 = CARTESIAN_POINT ( 'NONE',  ( 1.620813648195540191, 117.9496053335228822, -1.310909995308043197 ) ) ;
#20198 = CARTESIAN_POINT ( 'NONE',  ( 0.8805184999822103231, 105.9455060897651748, -5.280965183963572507 ) ) ;
#20199 = CARTESIAN_POINT ( 'NONE',  ( -4.351716102370955852, 120.3584862571861436, -0.7474562918332058326 ) ) ;
#20200 = CARTESIAN_POINT ( 'NONE',  ( 5.299048467822902175, 104.6144662015457527, -1.294354682138050050 ) ) ;
#20201 = CARTESIAN_POINT ( 'NONE',  ( -17.14500000000466784, 71.11999999999886768, -1.270000000000000684 ) ) ;
#20202 = CARTESIAN_POINT ( 'NONE',  ( 8.334503520420716072, 120.0709494557483339, -1.118110265123128055 ) ) ;
#20203 = CARTESIAN_POINT ( 'NONE',  ( -15.78614082382951977, 146.2329385241212378, -0.1139063483988971143 ) ) ;
#20204 = FACE_OUTER_BOUND ( 'NONE', #2225, .T. ) ;
#20205 = CARTESIAN_POINT ( 'NONE',  ( 21.97734904378678422, 136.8935083344700558, 1.380722529463845660 ) ) ;
#20206 = DIRECTION ( 'NONE',  ( -4.017660918040594346E-17, 1.000000000000000000, 2.376309959284834438E-19 ) ) ;
#20207 = CARTESIAN_POINT ( 'NONE',  ( 3.392805262616394035, -14.86080682751021698, 1.607197643132475040 ) ) ;
#20208 = CARTESIAN_POINT ( 'NONE',  ( -17.15907173562178301, 135.3907879583883869, 1.705144375702607462 ) ) ;
#20209 = CARTESIAN_POINT ( 'NONE',  ( -0.06925455797148694081, -4.192134993018743927, -0.9746272421430232091 ) ) ;
#20210 = CARTESIAN_POINT ( 'NONE',  ( -22.38168272118577207, 137.0915487549672491, -1.023064006592828035 ) ) ;
#20211 = CONICAL_SURFACE ( 'NONE', #22239, 12.69999999999999751, 0.7853981633974485010 ) ;
#20212 = CARTESIAN_POINT ( 'NONE',  ( 0.5759086045921885111, -9.199343823100290862, -0.7873135961421041662 ) ) ;
#20213 = EDGE_LOOP ( 'NONE', ( #33351, #18797, #11045, #17972 ) ) ;
#20214 = CARTESIAN_POINT ( 'NONE',  ( -43.08902205111511563, 20.96483665317663991, 0.2987222196696301402 ) ) ;
#20215 = CARTESIAN_POINT ( 'NONE',  ( 4.758673294993224445, 116.4582014290525507, 1.187054331573000665 ) ) ;
#20216 = CARTESIAN_POINT ( 'NONE',  ( -16.12610658153788634, 147.0533492130506943, 0.6457432798159423726 ) ) ;
#20217 = CARTESIAN_POINT ( 'NONE',  ( 4.523112235310252416, -13.07411707498565256, 2.966381825927230764 ) ) ;
#20218 = CARTESIAN_POINT ( 'NONE',  ( 10.60072409500453894, 154.2769816202975051, -1.465916755537046257 ) ) ;
#20219 = CARTESIAN_POINT ( 'NONE',  ( -0.9995654073149882191, 157.9544661020348997, -1.649992931013676056 ) ) ;
#20220 = CARTESIAN_POINT ( 'NONE',  ( -2.605357903967354893, 104.6144662015456959, 4.072382052623323645 ) ) ;
#20221 = CARTESIAN_POINT ( 'NONE',  ( 1.826496821415126037, -15.21410320048187437, 5.439012564009855666 ) ) ;
#20222 = CARTESIAN_POINT ( 'NONE',  ( -4.796574687651021129, 117.5429962573173981, -1.162632163661158735 ) ) ;
#20223 = CARTESIAN_POINT ( 'NONE',  ( 14.69813734295220442, 148.8396455022467535, 0.06702550439777867075 ) ) ;
#20224 = CIRCLE ( 'NONE', #25684, 0.2539999999999973390 ) ;
#20225 = ORIENTED_EDGE ( 'NONE', *, *, #22058, .T. ) ;
#20226 = CARTESIAN_POINT ( 'NONE',  ( -4.687559322878096957, 113.9922470800761687, 1.949581705681876276 ) ) ;
#20228 = EDGE_CURVE ( 'NONE', #27998, #14963, #13600, .T. ) ;
#20227 = CARTESIAN_POINT ( 'NONE',  ( 4.824354732525579337, 115.9539249584174740, 1.371586674499254421 ) ) ;
#20229 = CARTESIAN_POINT ( 'NONE',  ( 3.967518560505680636, 117.3993838585351881, 1.334307535890729035 ) ) ;
#20230 = EDGE_CURVE ( 'NONE', #17780, #35799, #35610, .T. ) ;
#20231 = CARTESIAN_POINT ( 'NONE',  ( -5.008948584507882273, 27.92152162925472325, 0.4889012661100834434 ) ) ;
#20232 = CARTESIAN_POINT ( 'NONE',  ( 22.83127913370401529, 150.4067493646842593, 0.3029848903584390074 ) ) ;
#20233 = CARTESIAN_POINT ( 'NONE',  ( -1.581412096509254628, 106.2431249238853894, 5.111785082781967304 ) ) ;
#20234 = CARTESIAN_POINT ( 'NONE',  ( 2.067624514165773419, -15.48293130374715787, 5.973957261547347741 ) ) ;
#20235 = DIRECTION ( 'NONE',  ( 0.000000000000000000, 1.000000000000000000, 0.000000000000000000 ) ) ;
#20236 = CARTESIAN_POINT ( 'NONE',  ( -4.870677750350147051, 117.7576918812740558, -0.8062859734791398836 ) ) ;
#20237 = CARTESIAN_POINT ( 'NONE',  ( 13.20682171306282449, 121.8780043825237982, 1.728041046422398086 ) ) ;
#20238 = ORIENTED_EDGE ( 'NONE', *, *, #2488, .T. ) ;
#20239 = CARTESIAN_POINT ( 'NONE',  ( 0.7039615705130309875, 19.50765702457006157, -8.391957350905826729 ) ) ;
#20240 = CARTESIAN_POINT ( 'NONE',  ( 2.231875883732710619, 116.9306593240908683, -0.4829567074209755173 ) ) ;
#20241 = CARTESIAN_POINT ( 'NONE',  ( -0.1328480158796658539, 107.4969721965504021, -4.685401909699153045 ) ) ;
#20242 = CARTESIAN_POINT ( 'NONE',  ( -5.540303739757925783, 78.91648400349117765, 5.100389098699535495 ) ) ;
#20243 = CARTESIAN_POINT ( 'NONE',  ( -10.54112285291057560, 57.14999999999385949, -5.016499999999999737 ) ) ;
#20244 = CARTESIAN_POINT ( 'NONE',  ( -0.05238710761692585982, 113.0327356262574341, 2.621665085262908867 ) ) ;
#20245 = CARTESIAN_POINT ( 'NONE',  ( -3.609430071560130848, 3.966570591990036032, 2.889066364458971137 ) ) ;
#20246 = DIRECTION ( 'NONE',  ( 5.188838149069472160E-16, -1.699382548006136559E-16, -1.000000000000000000 ) ) ;
#20247 = CARTESIAN_POINT ( 'NONE',  ( -5.348924234571052594, 56.51499999999999346, -4.492130288940743732 ) ) ;
#20248 = CARTESIAN_POINT ( 'NONE',  ( 3.370512099616890467, -13.86485436517860492, 3.147780574041331825 ) ) ;
#20249 = CARTESIAN_POINT ( 'NONE',  ( 5.811537524186114467, 124.3836500214474654, 0.1011232793223460352 ) ) ;
#20250 = CARTESIAN_POINT ( 'NONE',  ( -18.06489503062833535, 125.1493905788104684, 0.4137567899827963025 ) ) ;
#20251 = FACE_OUTER_BOUND ( 'NONE', #36804, .T. ) ;
#20252 = FACE_OUTER_BOUND ( 'NONE', #8103, .T. ) ;
#20253 = ORIENTED_EDGE ( 'NONE', *, *, #26109, .F. ) ;
#20254 = FACE_OUTER_BOUND ( 'NONE', #30490, .T. ) ;
#20255 = CARTESIAN_POINT ( 'NONE',  ( 3.150932678494966055, -15.78083729861913476, 4.935700751529307873 ) ) ;
#20256 = CARTESIAN_POINT ( 'NONE',  ( -4.124323422702007136, 118.5849532427036905, 0.8258982430451994317 ) ) ;
#20257 = CARTESIAN_POINT ( 'NONE',  ( 4.114294302962228755, -10.72644468530807416, -2.136776772127288559 ) ) ;
#20258 = CARTESIAN_POINT ( 'NONE',  ( -58.68158197657997022, -0.3140746753423795390, -0.3081004635821821824 ) ) ;
#20259 = ORIENTED_EDGE ( 'NONE', *, *, #40422, .T. ) ;
#20260 = CARTESIAN_POINT ( 'NONE',  ( -58.36222274556654099, -0.2757005147482338714, -0.1096927518867439194 ) ) ;
#20261 = CARTESIAN_POINT ( 'NONE',  ( -0.07931638298556013822, 106.1822392402443143, 5.212590348647615279 ) ) ;
#20262 = FILL_AREA_STYLE_COLOUR ( '', #33221 ) ;
#20263 = CARTESIAN_POINT ( 'NONE',  ( -6.553475369667642880, 120.9817801663137971, 0.6941111757064589716 ) ) ;
#20264 = DIRECTION ( 'NONE',  ( 0.8745520943968240202, -0.4849315768086553402, 6.829619984160650158E-16 ) ) ;
#20265 = CARTESIAN_POINT ( 'NONE',  ( 14.85905242749865707, 128.5561590274816126, -1.519445497462470263 ) ) ;
#20266 = CARTESIAN_POINT ( 'NONE',  ( -11.58042324368383014, 121.0393782313542346, -1.653871040030608475 ) ) ;
#20267 = PLANE ( 'NONE',  #19509 ) ;
#20268 = AXIS2_PLACEMENT_3D ( 'NONE', #9804, #22984, #25775 ) ;
#20269 = CARTESIAN_POINT ( 'NONE',  ( 4.117084068517360862, 118.2429491485453354, -0.1876423749214011782 ) ) ;
#20270 = CARTESIAN_POINT ( 'NONE',  ( 13.37097581265829938, 134.1388935151753401, -0.4393653360420517462 ) ) ;
#20271 = ORIENTED_EDGE ( 'NONE', *, *, #7752, .T. ) ;
#20272 = CARTESIAN_POINT ( 'NONE',  ( 3.348477204222540138, -14.79883842983281639, 1.177367440313774605 ) ) ;
#20273 = CARTESIAN_POINT ( 'NONE',  ( 1.490983790026257028, 105.1236484711430847, -5.131369187154176004 ) ) ;
#20274 = CARTESIAN_POINT ( 'NONE',  ( -49.24775882308124864, 17.43196194296904267, 5.046047204421642007 ) ) ;
#20275 = ADVANCED_FACE ( 'NONE', ( #20390 ), #27788, .T. ) ;
#20276 = CARTESIAN_POINT ( 'NONE',  ( -3.663749374568059380, -0.07195744677916669774, 2.838909333946205482 ) ) ;
#20277 = CARTESIAN_POINT ( 'NONE',  ( 5.014048726638124620, 156.2174774745075183, 1.508183953414442557 ) ) ;
#20278 = CARTESIAN_POINT ( 'NONE',  ( -2.647397774264983017, 29.53842282114184670, -0.004108860927264268610 ) ) ;
#20279 = CARTESIAN_POINT ( 'NONE',  ( 4.076717266748975277, 8.489475128091552136, -2.202413229635628689 ) ) ;
#20280 = CARTESIAN_POINT ( 'NONE',  ( 11.17680165766851808, 128.1157469881088105, 0.4152311708251575362 ) ) ;
#20281 = CARTESIAN_POINT ( 'NONE',  ( -5.101912418190827303, 113.7221701807922329, 1.664754118330573851 ) ) ;
#20282 = CARTESIAN_POINT ( 'NONE',  ( -55.83515739322315596, 4.224161455597911008, -0.1887094293950861423 ) ) ;
#20283 = CARTESIAN_POINT ( 'NONE',  ( -5.544930032391052421, 116.7707190791428928, -0.4007225579332259202 ) ) ;
#20284 = CARTESIAN_POINT ( 'NONE',  ( 8.078287538471617069, 158.6595088495342338, 0.1614234102745199240 ) ) ;
#20285 = CARTESIAN_POINT ( 'NONE',  ( -30.50798996576767763, 65.61473877417354572, -1.270000000000006901 ) ) ;
#20286 = DIRECTION ( 'NONE',  ( 0.7071067811865504593, 0.000000000000000000, 0.7071067811865445751 ) ) ;
#20287 = CARTESIAN_POINT ( 'NONE',  ( -30.03903471085840238, 57.95649848198893750, -1.523999999999813282 ) ) ;
#20288 = CARTESIAN_POINT ( 'NONE',  ( -6.529493367164978770E-14, 72.99146620154573384, -7.899616498973244731E-18 ) ) ;
#20289 = CARTESIAN_POINT ( 'NONE',  ( -5.449044798801134348, 56.51500000000043400, 5.145813327035688722 ) ) ;
#20290 = FACE_OUTER_BOUND ( 'NONE', #35709, .T. ) ;
#20291 = CARTESIAN_POINT ( 'NONE',  ( -58.69054519303719530, 0.2722345423086247607, 0.6021937201626180736 ) ) ;
#20292 = CARTESIAN_POINT ( 'NONE',  ( 0.4220321208936545498, 124.6436471961814050, -0.02396868521112067649 ) ) ;
#20293 = CARTESIAN_POINT ( 'NONE',  ( -20.63094779205708562, 152.5829384802601396, 0.02634999427677331418 ) ) ;
#20294 = VERTEX_POINT ( 'NONE', #37798 ) ;
#20295 = CARTESIAN_POINT ( 'NONE',  ( -56.07077906059188166, 6.725046902222183931, -2.233835758070444655 ) ) ;
#20296 = CARTESIAN_POINT ( 'NONE',  ( 6.967896315201691948, 121.9471128632948620, 0.02251729312944412628 ) ) ;
#20297 = AXIS2_PLACEMENT_3D ( 'NONE', #32890, #318, #7326 ) ;
#20298 = VERTEX_POINT ( 'NONE', #36407 ) ;
#20299 = CARTESIAN_POINT ( 'NONE',  ( -17.14500000000466784, 71.11999999999886768, -1.270000000000000684 ) ) ;
#20300 = CARTESIAN_POINT ( 'NONE',  ( -12.88021573494099314, 133.7932622986943159, -0.3045934876098301269 ) ) ;
#20301 = CARTESIAN_POINT ( 'NONE',  ( 6.169188725349925129, -14.24425063093240418, 1.535968726618487379 ) ) ;
#20302 = AXIS2_PLACEMENT_3D ( 'NONE', #15445, #28448, #12258 ) ;
#20303 = CARTESIAN_POINT ( 'NONE',  ( -21.06902287100059823, 145.7918284779248665, 1.526944944257475845 ) ) ;
#20304 = CARTESIAN_POINT ( 'NONE',  ( -4.563195415240126174, 21.88328375387019165, -0.7336086519975816289 ) ) ;
#20305 = CARTESIAN_POINT ( 'NONE',  ( 11.56079167746327130, 118.7825156662901378, 0.6096482884850571438 ) ) ;
#20306 = CARTESIAN_POINT ( 'NONE',  ( -5.451267667241070720E-14, 85.80437499999999318, 0.000000000000000000 ) ) ;
#20307 = CARTESIAN_POINT ( 'NONE',  ( 3.211436584971100849, 28.15539441671475274, -3.345526564039049688 ) ) ;
#20308 = CARTESIAN_POINT ( 'NONE',  ( 0.7576854961709549308, -2.078890728193560467, 0.6140693529290401909 ) ) ;
#20309 = CARTESIAN_POINT ( 'NONE',  ( -0.9122582399081905491, 116.5216256635990391, -0.1489946802529017456 ) ) ;
#20310 = DIRECTION ( 'NONE',  ( 0.1906721105965039909, -0.9816537812491094028, 2.657572025465702696E-16 ) ) ;
#20311 = DIRECTION ( 'NONE',  ( 5.188838149069472160E-16, -1.699382548006136559E-16, -1.000000000000000000 ) ) ;
#20312 = CARTESIAN_POINT ( 'NONE',  ( 5.539609713687273285, 116.8468292325185587, 0.4796846802364603812 ) ) ;
#20313 = CARTESIAN_POINT ( 'NONE',  ( -17.40456409200978527, 148.7932787949812905, 1.578286399122462935 ) ) ;
#20314 = CARTESIAN_POINT ( 'NONE',  ( -58.09428082180522779, 0.3001999070928298430, -0.7274870244324989077 ) ) ;
#20315 = CARTESIAN_POINT ( 'NONE',  ( 2.141138273642768208, 117.8876587302075194, 0.7126953207602170215 ) ) ;
#20316 = CARTESIAN_POINT ( 'NONE',  ( 13.00445675891829467, 122.7019651155717384, -1.321991537619922497 ) ) ;
#20317 = CARTESIAN_POINT ( 'NONE',  ( -0.1719059670432218079, -9.367746741450257986, 0.9581547781327369728 ) ) ;
#20318 = CARTESIAN_POINT ( 'NONE',  ( -13.54946078406819332, 121.5020190402118203, -1.609302047640724931 ) ) ;
#20319 = CARTESIAN_POINT ( 'NONE',  ( -46.07906060731711761, 24.80782705053048076, -1.769089518196001798 ) ) ;
#20320 = CARTESIAN_POINT ( 'NONE',  ( 4.971145480241967007, 105.1217302803469664, 1.943640820323331742 ) ) ;
#20321 = ADVANCED_FACE ( 'NONE', ( #40593 ), #27783, .T. ) ;
#20322 = CARTESIAN_POINT ( 'NONE',  ( 3.332096981532907343, 156.3062290909284116, -1.017430637527963588 ) ) ;
#20323 = CARTESIAN_POINT ( 'NONE',  ( 7.785313405276816034, 122.6175842484440324, 0.2316741178401685586 ) ) ;
#20324 = ORIENTED_EDGE ( 'NONE', *, *, #38073, .T. ) ;
#20325 = CARTESIAN_POINT ( 'NONE',  ( -12.01154561878613336, 123.1955650103826798, -1.772196977085516156 ) ) ;
#20326 = CARTESIAN_POINT ( 'NONE',  ( 5.270497567351643653, -15.36183412081716604, 0.7307456425073816098 ) ) ;
#20327 = CARTESIAN_POINT ( 'NONE',  ( -12.21488373879588885, 56.36092316367923871, 5.016500000000000625 ) ) ;
#20328 = CARTESIAN_POINT ( 'NONE',  ( -4.565208948191195937, 118.0820071162333988, -0.7244444172681095973 ) ) ;
#20329 = EDGE_CURVE ( 'NONE', #26503, #2001, #4021, .T. ) ;
#20330 = CARTESIAN_POINT ( 'NONE',  ( -54.98111839650035648, 8.542840639972862249, -3.427624633821342304 ) ) ;
#20331 = CARTESIAN_POINT ( 'NONE',  ( 4.065926199369043204, 118.2429491485453354, 0.3080910687088499467 ) ) ;
#20332 = CARTESIAN_POINT ( 'NONE',  ( 8.349261126152542900, 120.8878392079396065, 1.399984990019641717 ) ) ;
#20333 = CARTESIAN_POINT ( 'NONE',  ( -4.679832524073478162, 32.47693947602098063, 1.143146696348500635 ) ) ;
#20334 = CIRCLE ( 'NONE', #23744, 0.7620000000000000107 ) ;
#20335 = CARTESIAN_POINT ( 'NONE',  ( 0.0002511744760192916428, 116.4254662015457171, -0.01256979787922172728 ) ) ;
#20336 = CARTESIAN_POINT ( 'NONE',  ( -7.546363725996330984, 11.73557930518083303, -3.739946900464478752 ) ) ;
#20337 = CARTESIAN_POINT ( 'NONE',  ( 6.479597433594296518, 121.6155390319085683, 0.5171962410403526667 ) ) ;
#20338 = EDGE_CURVE ( 'NONE', #27342, #19390, #18262, .T. ) ;
#20339 = CARTESIAN_POINT ( 'NONE',  ( 14.74755344529021173, 121.0688405154646858, -0.6244351273456010265 ) ) ;
#20340 = DIRECTION ( 'NONE',  ( 5.188838149069472160E-16, -1.699382548006136559E-16, -1.000000000000000000 ) ) ;
#20341 = CARTESIAN_POINT ( 'NONE',  ( -33.20758249455312239, 49.81222039523557044, -1.524000000000005572 ) ) ;
#20342 = CARTESIAN_POINT ( 'NONE',  ( -16.27668397883912377, 121.4070763266325628, -0.2738251655545989038 ) ) ;
#20343 = ORIENTED_EDGE ( 'NONE', *, *, #35530, .F. ) ;
#20344 = EDGE_CURVE ( 'NONE', #30637, #34369, #38014, .T. ) ;
#20345 = CARTESIAN_POINT ( 'NONE',  ( -6.800033062875029621, 121.3213576459294529, -0.8666892964309956815 ) ) ;
#20346 = CARTESIAN_POINT ( 'NONE',  ( -47.16908398257407953, 25.15707121737368013, -1.640988021986792500 ) ) ;
#20347 = ORIENTED_EDGE ( 'NONE', *, *, #8174, .F. ) ;
#20348 = DIRECTION ( 'NONE',  ( -5.206863593109713661E-17, 1.000000000000000000, -1.077750396879097183E-30 ) ) ;
#20349 = CARTESIAN_POINT ( 'NONE',  ( -10.48728279712184452, 126.1106773019354819, -0.5683957799248650078 ) ) ;
#20350 = CARTESIAN_POINT ( 'NONE',  ( 3.920414950246539298, -14.18668476855415506, 4.724392046630619291 ) ) ;
#20351 = CARTESIAN_POINT ( 'NONE',  ( -14.77829941377254563, 121.3346631531286164, 0.7297537739211615859 ) ) ;
#20352 = CARTESIAN_POINT ( 'NONE',  ( -5.959810334499720419, 155.3892724211786742, -0.1190911940436165245 ) ) ;
#20353 = CARTESIAN_POINT ( 'NONE',  ( 10.82992898448777730, 157.9016520041087688, 0.2364045824791625727 ) ) ;
#20354 = ORIENTED_EDGE ( 'NONE', *, *, #37346, .F. ) ;
#20355 = CARTESIAN_POINT ( 'NONE',  ( -2.646443841375008432, -8.127818987380491578, -3.789199236247322133 ) ) ;
#20356 = EDGE_CURVE ( 'NONE', #9144, #41686, #34615, .T. ) ;
#20357 = CARTESIAN_POINT ( 'NONE',  ( -23.36005780523123576, 148.8745345081378559, -0.4925575130201674812 ) ) ;
#20358 = CARTESIAN_POINT ( 'NONE',  ( 13.85159022459154876, 16.68226173831723003, 5.016499999999999737 ) ) ;
#20359 = AXIS2_PLACEMENT_3D ( 'NONE', #27368, #5806, #34764 ) ;
#20360 = CARTESIAN_POINT ( 'NONE',  ( -4.466782427718574588, 71.06098887363195615, -1.523999999999994248 ) ) ;
#20361 = ORIENTED_EDGE ( 'NONE', *, *, #8325, .F. ) ;
#20362 = CARTESIAN_POINT ( 'NONE',  ( -4.680895062149801333, 118.8338629270736675, 0.8901742599232486119 ) ) ;
#20363 = AXIS2_PLACEMENT_3D ( 'NONE', #24877, #15281, #22083 ) ;
#20364 = CARTESIAN_POINT ( 'NONE',  ( 0.3254831797250597458, 1.427361272777448509, 4.610396533461925905 ) ) ;
#20365 = CARTESIAN_POINT ( 'NONE',  ( 21.58117366275196503, 150.4657531037631486, 1.865176240683389830 ) ) ;
#20366 = CARTESIAN_POINT ( 'NONE',  ( -57.50985127144645048, 1.621858126758690455, -1.632528232182590466 ) ) ;
#20368 = CARTESIAN_POINT ( 'NONE',  ( 4.979196860906016653, 118.3881331334009985, -0.8414419690753369707 ) ) ;
#20367 = DIRECTION ( 'NONE',  ( 0.4849315768086389089, 0.8745520943968330130, 4.371515779989697137E-15 ) ) ;
#20369 = CARTESIAN_POINT ( 'NONE',  ( -0.6580430243309095539, -8.493043821084315326, 4.585212396833119541 ) ) ;
#20370 = CARTESIAN_POINT ( 'NONE',  ( -0.3562832388057288191, 117.2097358735305050, -0.4069867078728326426 ) ) ;
#20371 = EDGE_CURVE ( 'NONE', #27023, #12982, #23707, .T. ) ;
#20372 = VERTEX_POINT ( 'NONE', #22016 ) ;
#20373 = CARTESIAN_POINT ( 'NONE',  ( -15.83367336760682242, 146.2622375132148989, 0.01472612784998108409 ) ) ;
#20374 = CARTESIAN_POINT ( 'NONE',  ( 5.498554953534677381, -14.76196523188227872, 3.265392988355040327 ) ) ;
#20375 = DIRECTION ( 'NONE',  ( 5.188838149069472160E-16, -1.699382548006136559E-16, -1.000000000000000000 ) ) ;
#20376 = DIRECTION ( 'NONE',  ( 1.011795553208986377E-16, 1.000000000000000000, -0.000000000000000000 ) ) ;
#20377 = EDGE_LOOP ( 'NONE', ( #26971, #32427, #26577, #28941 ) ) ;
#20378 = CARTESIAN_POINT ( 'NONE',  ( 18.75244783997680642, 140.8526363637247982, 2.516729932275435289 ) ) ;
#20379 = LINE ( 'NONE', #30400, #37291 ) ;
#20380 = DIRECTION ( 'NONE',  ( 0.9998004120163608288, 0.000000000000000000, 0.01997839162482749342 ) ) ;
#20381 = CARTESIAN_POINT ( 'NONE',  ( -22.55594873278735690, 149.0203452686010337, 0.8552431815872720833 ) ) ;
#20382 = CARTESIAN_POINT ( 'NONE',  ( 5.057590804293729647, 14.82039226405042243, -6.742867120243351664 ) ) ;
#20383 = CARTESIAN_POINT ( 'NONE',  ( 1.480437121830054492, 120.3785564700922492, 0.4209679054048331426 ) ) ;
#20384 = LINE ( 'NONE', #7843, #19915 ) ;
#20385 = AXIS2_PLACEMENT_3D ( 'NONE', #2559, #34708, #1923 ) ;
#20386 = CARTESIAN_POINT ( 'NONE',  ( 23.19190728264271684, 146.6831645211815101, -0.2733909575703941663 ) ) ;
#20387 = CARTESIAN_POINT ( 'NONE',  ( -26.51793118801306548, 72.98537704160715123, -1.270000000000006013 ) ) ;
#20388 = CARTESIAN_POINT ( 'NONE',  ( -57.73720092555902283, 1.073063965931175145, 1.165893645650359911 ) ) ;
#20389 = CARTESIAN_POINT ( 'NONE',  ( -48.33886291794431145, 23.55519408767752054, 1.110521498696428910 ) ) ;
#20390 = FACE_OUTER_BOUND ( 'NONE', #6658, .T. ) ;
#20391 = CARTESIAN_POINT ( 'NONE',  ( -52.97391985390434144, 12.30611266682019789, 4.247241762254901687 ) ) ;
#20392 = CARTESIAN_POINT ( 'NONE',  ( -58.18395191960946278, 0.6639886956250335981, 1.155333695069822975 ) ) ;
#20393 = CARTESIAN_POINT ( 'NONE',  ( -4.373713130305017849, 118.1839426225389929, 0.4384037898859596272 ) ) ;
#20394 = CARTESIAN_POINT ( 'NONE',  ( 0.1058213901577373939, 105.9761915687788729, -5.295735085525933528 ) ) ;
#20395 = ADVANCED_FACE ( 'NONE', ( #28214 ), #31189, .F. ) ;
#20396 = VERTEX_POINT ( 'NONE', #22426 ) ;
#20397 = CARTESIAN_POINT ( 'NONE',  ( -45.76673701974917208, 25.51931200435043934, 1.523999999999991806 ) ) ;
#20398 = CARTESIAN_POINT ( 'NONE',  ( -8.321911373758148045, 119.8826751762191947, -1.444119111808247036 ) ) ;
#20399 = CARTESIAN_POINT ( 'NONE',  ( -5.752478121743209272, 118.4424948052634647, -0.6632437998952303015 ) ) ;
#20400 = CARTESIAN_POINT ( 'NONE',  ( 4.592985736287271692, 118.0632451551486639, 0.7326753542377543171 ) ) ;
#20401 = CARTESIAN_POINT ( 'NONE',  ( -13.94748453383795983, 150.2679186505038160, -1.219128122479325338 ) ) ;
#20402 = CARTESIAN_POINT ( 'NONE',  ( -0.6559789189618892014, 115.7031633261756127, -1.758493996336355059 ) ) ;
#20403 = CARTESIAN_POINT ( 'NONE',  ( 2.608821018174404927, 117.3993834728566270, -1.321848261876171327 ) ) ;
#20404 = CARTESIAN_POINT ( 'NONE',  ( 5.270289556066540371, 116.2365830367532595, -0.9655167061512665017 ) ) ;
#20405 = CARTESIAN_POINT ( 'NONE',  ( -16.63795227869236015, 147.2809512400332608, -1.774228895505126413 ) ) ;
#20406 = CARTESIAN_POINT ( 'NONE',  ( -5.247413993112555630, 104.6144662015457385, -1.481417380683311968 ) ) ;
#20407 = CARTESIAN_POINT ( 'NONE',  ( -46.48963984823834039, 20.58996865087918238, 4.821990630911828113 ) ) ;
#20408 = DIRECTION ( 'NONE',  ( -0.9998004120163608288, 0.000000000000000000, -0.01997839162482749342 ) ) ;
#20409 = CARTESIAN_POINT ( 'NONE',  ( -0.6434349170078753621, 156.3034662015460583, 0.09435672052066400306 ) ) ;
#20410 = EDGE_CURVE ( 'NONE', #22322, #23948, #18935, .T. ) ;
#20411 = CARTESIAN_POINT ( 'NONE',  ( 4.560443946511397506, -11.68866997254031936, 0.6947937310338139216 ) ) ;
#20412 = CARTESIAN_POINT ( 'NONE',  ( 15.61264994714010079, 121.4606353739761744, 1.010464550865948663 ) ) ;
#20413 = CARTESIAN_POINT ( 'NONE',  ( 6.059261036834406866, 65.30181249999998272, -5.016499999999999737 ) ) ;
#20414 = CARTESIAN_POINT ( 'NONE',  ( 3.405374690515594605, -14.89039384781155917, 1.812165507210882209 ) ) ;
#20415 = AXIS2_PLACEMENT_3D ( 'NONE', #31396, #9656, #3921 ) ;
#20416 = CARTESIAN_POINT ( 'NONE',  ( -4.259301615573863664, 119.5670751559891585, 0.7808790134437381125 ) ) ;
#20417 = CARTESIAN_POINT ( 'NONE',  ( 0.9474642044963531573, -6.343762114497205395, -0.2236011429025598352 ) ) ;
#20418 = CARTESIAN_POINT ( 'NONE',  ( -23.10841651933913354, 148.9583646262859133, -1.191549328111825456 ) ) ;
#20419 = EDGE_CURVE ( 'NONE', #1859, #34293, #31833, .T. ) ;
#20420 = CARTESIAN_POINT ( 'NONE',  ( -0.7486558104752240039, 25.82057725623272759, -0.6268360674696834556 ) ) ;
#20421 = VERTEX_POINT ( 'NONE', #35249 ) ;
#20422 = CARTESIAN_POINT ( 'NONE',  ( -53.87733401397680666, 8.744676589845553849, 2.811092830483123084 ) ) ;
#20423 = CARTESIAN_POINT ( 'NONE',  ( 5.433204070470799785, 117.5340897209903517, 0.8253704096831886439 ) ) ;
#20424 = PRODUCT_CONTEXT ( 'NONE', #24331, 'mechanical' ) ;
#20425 = CARTESIAN_POINT ( 'NONE',  ( -2.723409340394791212, 120.7183352303693340, 0.2545450062501627420 ) ) ;
#20426 = CARTESIAN_POINT ( 'NONE',  ( 2.708195657389492084, -14.88772387794683105, 5.660366118324242635 ) ) ;
#20427 = CARTESIAN_POINT ( 'NONE',  ( 16.99563481483657412, 148.6336825499269310, -1.463981761124605985 ) ) ;
#20428 = EDGE_LOOP ( 'NONE', ( #5580, #14828, #26300 ) ) ;
#20429 = CARTESIAN_POINT ( 'NONE',  ( -12.70837813489441359, 122.8260676081006153, -1.843161107213562966 ) ) ;
#20430 = CARTESIAN_POINT ( 'NONE',  ( 4.831188463146562917, 104.6144662015457527, 0.2218974365694108553 ) ) ;
#20431 = CARTESIAN_POINT ( 'NONE',  ( 3.198224922426783579, -14.19254063666773291, 2.189163805996276579 ) ) ;
#20432 = CARTESIAN_POINT ( 'NONE',  ( -4.932018240231780482, 117.5375708271148767, -1.014072823415046454 ) ) ;
#20433 = CARTESIAN_POINT ( 'NONE',  ( 7.821695933845084880, 154.6216606121152495, -0.03501689623823063535 ) ) ;
#20434 = VERTEX_POINT ( 'NONE', #32040 ) ;
#20435 = DIRECTION ( 'NONE',  ( 9.627370216492862708E-17, 1.000000000000000000, -0.000000000000000000 ) ) ;
#20436 = DIRECTION ( 'NONE',  ( 4.017660918040594346E-17, -1.000000000000000000, -2.376309959284834438E-19 ) ) ;
#20437 =( BOUNDED_CURVE ( )  B_SPLINE_CURVE ( 3, ( #39777, #13194, #41968, #12973 ),
 .UNSPECIFIED., .F., .T. ) 
 B_SPLINE_CURVE_WITH_KNOTS ( ( 4, 4 ),
 ( 4.712388980384688786, 5.673871460451329618 ),
 .UNSPECIFIED. ) 
 CURVE ( )  GEOMETRIC_REPRESENTATION_ITEM ( )  RATIONAL_B_SPLINE_CURVE ( ( 1.000000000000000000, 0.9244349266169029633, 0.9244349266169029633, 1.000000000000000000 ) ) 
 REPRESENTATION_ITEM ( '' )  );
#20438 = CARTESIAN_POINT ( 'NONE',  ( -11.74288454345109756, 118.7273140689154616, -0.2346507796901759757 ) ) ;
#20439 = AXIS2_PLACEMENT_3D ( 'NONE', #38044, #5687, #31009 ) ;
#20440 = CARTESIAN_POINT ( 'NONE',  ( -9.960492004070044203, 64.81807050032566053, 1.270000000000003126 ) ) ;
#20441 = CARTESIAN_POINT ( 'NONE',  ( 16.13169674176108970, 121.3783152868344075, 0.08747489889995967161 ) ) ;
#20442 = CARTESIAN_POINT ( 'NONE',  ( 18.35410564743290607, 77.35382415001784295, -5.016499999999999737 ) ) ;
#20443 = AXIS2_PLACEMENT_3D ( 'NONE', #3441, #20024, #16836 ) ;
#20444 = CARTESIAN_POINT ( 'NONE',  ( 2.066596093631920983, -15.63843245996494957, 5.503614811026269038 ) ) ;
#20445 = CARTESIAN_POINT ( 'NONE',  ( 5.035933200060415338, 117.3993844219003648, -0.5513780243448201945 ) ) ;
#20446 = CARTESIAN_POINT ( 'NONE',  ( 0.7352267002175607580, 35.04949881550903967, -0.1714435552774139504 ) ) ;
#20447 = CARTESIAN_POINT ( 'NONE',  ( 13.02489573621943286, 155.4510764517707742, 2.156236249524808635 ) ) ;
#20448 = ORIENTED_EDGE ( 'NONE', *, *, #12552, .F. ) ;
#20449 = CARTESIAN_POINT ( 'NONE',  ( -3.861838729977780993, 14.11015702457025078, 7.483763204152318771 ) ) ;
#20450 = CARTESIAN_POINT ( 'NONE',  ( 8.638409582537143194, 118.5547056413952873, -0.7669449099685430316 ) ) ;
#20451 = CARTESIAN_POINT ( 'NONE',  ( -0.7907262360441658089, 106.8474934270474392, -4.937153267606968932 ) ) ;
#20452 = DIRECTION ( 'NONE',  ( 0.7770581983690701966, -0.6294287539884197979, 8.537024980200731099E-16 ) ) ;
#20453 = CARTESIAN_POINT ( 'NONE',  ( -1.569970522942491176, 106.5487815437991515, -5.038282329708090757 ) ) ;
#20454 = FACE_OUTER_BOUND ( 'NONE', #14710, .T. ) ;
#20455 = CARTESIAN_POINT ( 'NONE',  ( 2.229080734463354307, 9.364070591990056869, -4.050418370856919914 ) ) ;
#20456 = CARTESIAN_POINT ( 'NONE',  ( -11.24191166894635074, 82.34025985790688651, -1.269999999999999574 ) ) ;
#20457 = CARTESIAN_POINT ( 'NONE',  ( -4.829921688775540289, 118.5264896598256854, 0.7637249497284026578 ) ) ;
#20458 = CARTESIAN_POINT ( 'NONE',  ( 3.036083976128487016, -13.30543680819082297, 1.158518541688273729 ) ) ;
#20459 = CARTESIAN_POINT ( 'NONE',  ( 1.638321535317228239, 108.1711930243730109, -4.327427591587794886 ) ) ;
#20460 = CARTESIAN_POINT ( 'NONE',  ( -22.74771312706173276, 149.7444054411783441, 0.5134062617908414783 ) ) ;
#20461 = CARTESIAN_POINT ( 'NONE',  ( -3.521685918548247418, 29.33394459973516888, 3.031038535435704340 ) ) ;
#20462 = CYLINDRICAL_SURFACE ( 'NONE', #10021, 0.2539999999999998925 ) ;
#20463 = ORIENTED_EDGE ( 'NONE', *, *, #30257, .T. ) ;
#20464 = CARTESIAN_POINT ( 'NONE',  ( -2.362993923122841178, 104.6144662015455111, -4.208660904431277494 ) ) ;
#20465 = CARTESIAN_POINT ( 'NONE',  ( 4.689621780486535663, -15.62538141832135707, 3.172200491054990579 ) ) ;
#20466 = CARTESIAN_POINT ( 'NONE',  ( -20.46656357041398877, 147.8414448467482600, 1.666390110339677877 ) ) ;
#20467 = AXIS2_PLACEMENT_3D ( 'NONE', #10273, #3698, #17081 ) ;
#20468 = EDGE_CURVE ( 'NONE', #20372, #26546, #1306, .T. ) ;
#20469 = CARTESIAN_POINT ( 'NONE',  ( 0.8139239711521952803, 26.85569158835278003, 0.5393279072465841928 ) ) ;
#20470 = ORIENTED_EDGE ( 'NONE', *, *, #41179, .T. ) ;
#20471 = CARTESIAN_POINT ( 'NONE',  ( -58.36582417653014687, -0.2832568706219312782, -0.07935633695538733823 ) ) ;
#20472 = CARTESIAN_POINT ( 'NONE',  ( 0.2949767777649464628, 114.7739974199301116, 2.049407731665748855 ) ) ;
#20473 = B_SPLINE_SURFACE_WITH_KNOTS ( 'NONE', 1, 3, ( 
 ( #40844, #11646, #18233, #5282, #24630, #15042 ),
 ( #21422, #21632, #34450, #9096, #31235, #28259 ) ),
 .UNSPECIFIED., .F., .F., .F.,
 ( 2, 2 ),
 ( 4, 2, 4 ),
 ( 0.000000000000000000, 1.000000000000000000 ),
 ( 0.000000000000000000, 0.5000000000000000000, 1.000000000000000000 ),
 .UNSPECIFIED. ) ;
#20474 = CARTESIAN_POINT ( 'NONE',  ( -10.33346200648618840, 123.4707319107414492, 0.9080611472405732965 ) ) ;
#20475 = CARTESIAN_POINT ( 'NONE',  ( -4.974001918040873882, 117.3966124607983659, -0.9751453929904890794 ) ) ;
#20476 = CARTESIAN_POINT ( 'NONE',  ( 4.045847121365343746, 157.1622345443605582, -1.633529996401409612 ) ) ;
#20477 = VECTOR ( 'NONE', #13169, 1000.000000000000000 ) ;
#20478 = CARTESIAN_POINT ( 'NONE',  ( -20.59518377851929571, 148.5655811199389689, -2.440016074255365819 ) ) ;
#20479 = CARTESIAN_POINT ( 'NONE',  ( 5.332935397695203861, 104.6144662015457243, 0.1065647409268305201 ) ) ;
#20480 = CARTESIAN_POINT ( 'NONE',  ( 4.319275104837216439, 118.2117203735061395, -0.3219079343282689187 ) ) ;
#20481 = CARTESIAN_POINT ( 'NONE',  ( 4.503927054024090992, 120.9948550335633115, -0.2290337153283756866 ) ) ;
#20482 = EDGE_LOOP ( 'NONE', ( #39031, #24548, #26105, #23754 ) ) ;
#20483 = CARTESIAN_POINT ( 'NONE',  ( 3.263309282894114371, -14.66069363451780205, 2.445366243406764006 ) ) ;
#20484 = CARTESIAN_POINT ( 'NONE',  ( 11.32678463655022405, 56.02547433970799773, -4.456118031212427333 ) ) ;
#20485 = CARTESIAN_POINT ( 'NONE',  ( -57.87993506102255736, 0.7648122704443233166, 1.011066771891486749 ) ) ;
#20486 = CARTESIAN_POINT ( 'NONE',  ( 1.368391094521330897, 11.37271669962338372, 4.434453701053673313 ) ) ;
#20487 = CARTESIAN_POINT ( 'NONE',  ( 17.20807765352988028, 147.1820577694790018, 2.053081559533530331 ) ) ;
#20488 = CARTESIAN_POINT ( 'NONE',  ( -0.1611612690460884623, 32.88059107141324944, 1.736765093886240008 ) ) ;
#20489 = VECTOR ( 'NONE', #19880, 1000.000000000000114 ) ;
#20490 = CARTESIAN_POINT ( 'NONE',  ( -3.234384296441582762, 11.31316835407710819, -3.315160845070126427 ) ) ;
#20491 = CARTESIAN_POINT ( 'NONE',  ( 14.67383990354511702, 148.8475317811793559, 0.3438330757172307628 ) ) ;
#20492 = CARTESIAN_POINT ( 'NONE',  ( -5.274544067074300457, 115.7029491485454002, 0.8135768287290441325 ) ) ;
#20493 = CARTESIAN_POINT ( 'NONE',  ( -56.38098843839168950, 3.837951075127326916, -1.838241461164923596 ) ) ;
#20494 = CARTESIAN_POINT ( 'NONE',  ( -5.555076865044160428, 116.7283850868982711, -0.3026861340469938488 ) ) ;
#20495 = FACE_OUTER_BOUND ( 'NONE', #16165, .T. ) ;
#20496 = VECTOR ( 'NONE', #17464, 1000.000000000000114 ) ;
#20497 = ORIENTED_EDGE ( 'NONE', *, *, #41421, .T. ) ;
#20498 = CARTESIAN_POINT ( 'NONE',  ( -46.84878041887307631, 25.58252992934718861, -1.577652289021667986 ) ) ;
#20499 = DIRECTION ( 'NONE',  ( 0.9998239923360758841, -0.01876124593811817620, 2.121609341712732885E-15 ) ) ;
#20500 = CARTESIAN_POINT ( 'NONE',  ( -30.30981065304866107, 56.20484928089094012, -1.524000000000004240 ) ) ;
#20501 = CARTESIAN_POINT ( 'NONE',  ( 7.354229849910361771, -2.730604093522916109, 4.103208822889532925 ) ) ;
#20502 = DIRECTION ( 'NONE',  ( -0.9998004120163608288, 0.000000000000000000, -0.01997839162482747608 ) ) ;
#20503 = CARTESIAN_POINT ( 'NONE',  ( 1.231754723633442730E-15, 12.17394877578617063, 0.000000000000000000 ) ) ;
#20504 = CARTESIAN_POINT ( 'NONE',  ( -58.35673254475433680, 1.205555466438051893, 0.1480423017862440571 ) ) ;
#20505 = CARTESIAN_POINT ( 'NONE',  ( -58.73801720703743001, -0.4998429216807459552, -1.049519136981926467E-14 ) ) ;
#20506 = CARTESIAN_POINT ( 'NONE',  ( -15.31729018078755722, 120.6995131204970875, 0.01165691202436099257 ) ) ;
#20507 = EDGE_LOOP ( 'NONE', ( #30535, #34084, #39458, #8985 ) ) ;
#20508 = CARTESIAN_POINT ( 'NONE',  ( -57.92935616279446265, 2.416188466839983118, -0.2259612492382147286 ) ) ;
#20509 = DIRECTION ( 'NONE',  ( -0.8745520943968249084, 0.4849315768086533418, -5.271987356194193006E-16 ) ) ;
#20510 = EDGE_LOOP ( 'NONE', ( #16556, #15086, #11564, #20497, #8024 ) ) ;
#20511 = CARTESIAN_POINT ( 'NONE',  ( -45.67969256299926428, 21.13156854447444744, -4.214927840907465750 ) ) ;
#20512 = CARTESIAN_POINT ( 'NONE',  ( -15.78392762965212448, 146.2390805666957192, -0.3668625800963856709 ) ) ;
#20513 = CARTESIAN_POINT ( 'NONE',  ( 2.292478802652971659, -15.50831694688660534, 5.896745190559482985 ) ) ;
#20514 = CARTESIAN_POINT ( 'NONE',  ( -3.107221341096740197, 117.9340107969418341, 0.6831876054667452847 ) ) ;
#20515 = CARTESIAN_POINT ( 'NONE',  ( -4.191205975170537279, 21.45845178295031630, -1.961646697876042511 ) ) ;
#20516 = CARTESIAN_POINT ( 'NONE',  ( 21.37844900359467815, 132.5159896776619917, 0.8378797052005131363 ) ) ;
#20517 = CARTESIAN_POINT ( 'NONE',  ( 2.050826208811672657, -15.68011782295399037, 5.762527612234801921 ) ) ;
#20518 = CARTESIAN_POINT ( 'NONE',  ( -6.422645615570758970, 77.88548590848095898, -1.269999999999996465 ) ) ;
#20519 = CARTESIAN_POINT ( 'NONE',  ( 0.1793159252905947298, -3.154364953387045034, 0.9593126492898319535 ) ) ;
#20520 = CARTESIAN_POINT ( 'NONE',  ( -3.280774808778091245, 159.4678586119998442, -0.2050961497903012465 ) ) ;
#20521 = DIRECTION ( 'NONE',  ( -5.206863593109713661E-17, 1.000000000000000000, -1.077750396879097183E-30 ) ) ;
#20522 = DIRECTION ( 'NONE',  ( -0.8745520943968240202, 0.4849315768086551737, -5.361993529360572958E-16 ) ) ;
#20523 = CARTESIAN_POINT ( 'NONE',  ( 5.533816750157554587, 116.9218703105320429, 0.5587418741630174601 ) ) ;
#20524 = CARTESIAN_POINT ( 'NONE',  ( -5.414978495245632573, 156.5090806470891209, 1.537019876316040090 ) ) ;
#20525 = CARTESIAN_POINT ( 'NONE',  ( -58.06686319096232296, 0.3595372361034740449, -0.7669821491821283699 ) ) ;
#20526 = CARTESIAN_POINT ( 'NONE',  ( 6.794677088231689588, 118.4250403807481575, 1.128628347181275915 ) ) ;
#20527 = CARTESIAN_POINT ( 'NONE',  ( 13.71253074539970562, 123.6869008171703541, -1.368039988124472695 ) ) ;
#20528 = B_SPLINE_CURVE_WITH_KNOTS ( 'NONE', 3,
 ( #6232, #31789, #13242, #19203, #35833, #32211, #35204, #6649, #26014, #3044, #16002, #25803, #38405, #9622, #22590, #29211, #3459, #35622, #6436, #19410, #32417, #3247, #16422, #38188 ),
 .UNSPECIFIED., .F., .F.,
 ( 4, 2, 2, 2, 2, 2, 2, 2, 2, 2, 2, 4 ),
 ( 0.0005723024039399593997, 0.003660507319800902683, 0.006748712235661846401, 0.008292814693592298961, 0.009064865922557507893, 0.009836917151522718561, 0.01060896838048792923, 0.01138101960945313816, 0.01215307083841834883, 0.01253909645290095763, 0.01273210926014226724, 0.01292512206738357684 ),
 .UNSPECIFIED. ) ;
#20529 = CARTESIAN_POINT ( 'NONE',  ( 0.7131539557513479899, -7.844638678481905103, 0.6656887750258669856 ) ) ;
#20530 = CARTESIAN_POINT ( 'NONE',  ( -15.28824200187838755, 154.8698957928756954, -2.015933685939941267 ) ) ;
#20531 = CARTESIAN_POINT ( 'NONE',  ( -45.45367893016184979, 22.54667639846615046, -3.012003376585093317 ) ) ;
#20532 = AXIS2_PLACEMENT_3D ( 'NONE', #20503, #10929, #5196 ) ;
#20533 = CARTESIAN_POINT ( 'NONE',  ( 15.97699994813249091, 148.2453349897154737, -0.9478121846735142464 ) ) ;
#20534 = CARTESIAN_POINT ( 'NONE',  ( 7.846913280328204010, 122.2669436912714929, 0.7513606219076406356 ) ) ;
#20535 = VERTEX_POINT ( 'NONE', #35883 ) ;
#20536 = CARTESIAN_POINT ( 'NONE',  ( -16.38646240326728432, 135.1966315799913900, -2.295807278541857954 ) ) ;
#20537 = CARTESIAN_POINT ( 'NONE',  ( 4.918313631922730522, -15.33159817589810281, -0.1794070962640156031 ) ) ;
#20538 = DIRECTION ( 'NONE',  ( 5.188838149069472160E-16, -1.699382548006136559E-16, -1.000000000000000000 ) ) ;
#20539 = CARTESIAN_POINT ( 'NONE',  ( -4.528805603826046244, 118.1086152786259333, -0.6811083559245456609 ) ) ;
#20540 = CARTESIAN_POINT ( 'NONE',  ( -56.34046819891496938, 4.202508019718290022, -2.501728563949862760 ) ) ;
#20541 = CARTESIAN_POINT ( 'NONE',  ( -5.137966006445163991, 56.84472104120892055, -5.330653870689114449 ) ) ;
#20542 = CARTESIAN_POINT ( 'NONE',  ( 17.12878219156693760, 140.2562023718666353, 2.330665938063504417 ) ) ;
#20543 = DIRECTION ( 'NONE',  ( -0.01997839162482749342, -1.040247600000944484E-18, 0.9998004120163608288 ) ) ;
#20544 = AXIS2_PLACEMENT_3D ( 'NONE', #34780, #37338, #40549 ) ;
#20545 = CARTESIAN_POINT ( 'NONE',  ( 0.2937963077018297398, 116.4254261620736344, -0.006796306282692754844 ) ) ;
#20546 = CARTESIAN_POINT ( 'NONE',  ( 8.109546976224176973, 7.201272144248561879, 2.403482862635152539 ) ) ;
#20547 = CARTESIAN_POINT ( 'NONE',  ( 3.687801383043704639, 120.9852966486377710, 0.2688355818071224701 ) ) ;
#20548 = CARTESIAN_POINT ( 'NONE',  ( 22.54293160324719381, 149.6594668941642681, -0.7271591872719224137 ) ) ;
#20549 = CARTESIAN_POINT ( 'NONE',  ( 6.059261036834406866, 57.14999999999999858, 5.016499999999999737 ) ) ;
#20550 = CARTESIAN_POINT ( 'NONE',  ( -6.578476689077728991E-14, 85.18346620154574111, -5.002419396613184919E-18 ) ) ;
#20551 = TOROIDAL_SURFACE ( 'NONE', #2234, 5.080000000000005400, 0.5080000000000000071 ) ;
#20552 = CARTESIAN_POINT ( 'NONE',  ( -57.85534701229749999, 0.8496279762696401505, 1.203237356453207063 ) ) ;
#20553 = CARTESIAN_POINT ( 'NONE',  ( -18.63219679753396107, 154.1293031355326946, -0.2996243416495529832 ) ) ;
#20554 = ORIENTED_EDGE ( 'NONE', *, *, #41179, .F. ) ;
#20555 = CARTESIAN_POINT ( 'NONE',  ( -47.09845139715251605, 25.49303147219070098, -0.5484243623142366353 ) ) ;
#20556 = CARTESIAN_POINT ( 'NONE',  ( -6.814076468830258193, 121.3873156153395456, -0.8343114639089803664 ) ) ;
#20557 = DIRECTION ( 'NONE',  ( 4.017660918040594346E-17, -1.000000000000000000, -2.376309959284832031E-19 ) ) ;
#20558 = ORIENTED_EDGE ( 'NONE', *, *, #1925, .F. ) ;
#20559 = CARTESIAN_POINT ( 'NONE',  ( -9.712308604790303335, 65.53852105402241079, -1.269999999999996021 ) ) ;
#20560 = CARTESIAN_POINT ( 'NONE',  ( -14.79492108907976267, 148.8567844064068026, -0.8802232212986719206 ) ) ;
#20561 = CARTESIAN_POINT ( 'NONE',  ( 3.942998349758990440, -14.41637075870405482, 4.944918514907367779 ) ) ;
#20562 = CARTESIAN_POINT ( 'NONE',  ( -14.41840636618848670, 121.0470547900126519, 0.7241072410554124650 ) ) ;
#20563 = PLANE ( 'NONE',  #12491 ) ;
#20564 = CARTESIAN_POINT ( 'NONE',  ( 17.26848747421918873, 122.7565812399420651, 0.3979830900422688944 ) ) ;
#20565 = EDGE_CURVE ( 'NONE', #4600, #11324, #28473, .T. ) ;
#20566 = VERTEX_POINT ( 'NONE', #29260 ) ;
#20567 = CARTESIAN_POINT ( 'NONE',  ( -0.5496829067194369811, 0.7180641350488168317, -4.598301960397928489 ) ) ;
#20568 = ADVANCED_FACE ( 'NONE', ( #33103 ), #3293, .F. ) ;
#20569 = CARTESIAN_POINT ( 'NONE',  ( -20.50094783971104917, 129.0975500345852822, -0.4299227524276373891 ) ) ;
#20570 = DIRECTION ( 'NONE',  ( 0.01731298258487879230, -0.9998501190848636533, 2.678710623147156226E-15 ) ) ;
#20571 = AXIS2_PLACEMENT_3D ( 'NONE', #11179, #27781, #24164 ) ;
#20572 = CARTESIAN_POINT ( 'NONE',  ( -18.13811525448111439, 9.293884745518889545, 2.221278478896607584E-15 ) ) ;
#20573 = ORIENTED_EDGE ( 'NONE', *, *, #40422, .F. ) ;
#20574 = CARTESIAN_POINT ( 'NONE',  ( 8.133763292779583765, 120.8066077149993163, 1.378299465333653107 ) ) ;
#20575 = CARTESIAN_POINT ( 'NONE',  ( 4.471266627501615076, -5.469457446779734333, -1.220754042301255948 ) ) ;
#20576 = CARTESIAN_POINT ( 'NONE',  ( 15.93415399606955951, 122.8751182158008959, 1.397711951582541801 ) ) ;
#20577 = CARTESIAN_POINT ( 'NONE',  ( -58.64342337385304660, -0.3142157529030242813, -0.3359497956441734878 ) ) ;
#20578 = CARTESIAN_POINT ( 'NONE',  ( 18.49784594330472842, 151.8926627062091086, -1.576652458532300960 ) ) ;
#20579 = CARTESIAN_POINT ( 'NONE',  ( -1.722957355399680202, -2.895624787512894649, -4.295268622497145472 ) ) ;
#20580 = CARTESIAN_POINT ( 'NONE',  ( -1.323305960456944597, 159.4649289425152858, -0.7771481453362865111 ) ) ;
#20581 = VERTEX_POINT ( 'NONE', #19876 ) ;
#20582 = CARTESIAN_POINT ( 'NONE',  ( -11.18446751737367428, 128.1157469881088105, -0.03160020415517764830 ) ) ;
#20583 = CARTESIAN_POINT ( 'NONE',  ( 5.915669078949217230, -14.48123931593440972, 2.327441804047190033 ) ) ;
#20584 = CARTESIAN_POINT ( 'NONE',  ( -45.61851195612215548, 20.88128798641532313, 4.109017096223889887 ) ) ;
#20585 = DIRECTION ( 'NONE',  ( -1.000000000000000000, 0.000000000000000000, 0.000000000000000000 ) ) ;
#20586 = ORIENTED_EDGE ( 'NONE', *, *, #19801, .T. ) ;
#20587 = CARTESIAN_POINT ( 'NONE',  ( 13.34589015847587135, 154.0568829568526041, 2.281985820853443592 ) ) ;
#20588 = CARTESIAN_POINT ( 'NONE',  ( -6.606029807653651701E-14, 92.04146620154574521, -3.372746026535634231E-18 ) ) ;
#20589 = DIRECTION ( 'NONE',  ( 0.01997839162482749689, 1.040247600000945640E-18, -0.9998004120163610509 ) ) ;
#20590 = AXIS2_PLACEMENT_3D ( 'NONE', #11184, #30574, #17369 ) ;
#20591 = CARTESIAN_POINT ( 'NONE',  ( -11.13388036866237663, 119.2389763063149388, 0.6860836662663823970 ) ) ;
#20593 = EDGE_CURVE ( 'NONE', #28199, #40141, #9205, .T. ) ;
#20592 = CARTESIAN_POINT ( 'NONE',  ( 2.488832714281139946, 5.747567886007050042, -8.044950587805361764 ) ) ;
#20594 = CARTESIAN_POINT ( 'NONE',  ( 6.473539731754311077, 155.4519854478747902, 1.179574399179393662 ) ) ;
#20595 = CARTESIAN_POINT ( 'NONE',  ( -6.654617103318593247E-14, 104.6144662015457243, 1.534725424433578570E-31 ) ) ;
#20596 = CARTESIAN_POINT ( 'NONE',  ( 22.15286039372319493, 136.9573810088325843, -0.3857095667871863753 ) ) ;
#20597 = CARTESIAN_POINT ( 'NONE',  ( -3.174366308152013705, 104.6144662015457243, -0.06343139340882732180 ) ) ;
#20598 = CARTESIAN_POINT ( 'NONE',  ( -55.46911355273442013, 5.859935818251603479, 2.757237622174628644 ) ) ;
#20599 = CARTESIAN_POINT ( 'NONE',  ( -47.66286930719412851, 20.62480072838431155, 5.054501799269492501 ) ) ;
#20600 = CARTESIAN_POINT ( 'NONE',  ( -50.36516092884956208, 15.79195539882771726, 4.916963016749596349 ) ) ;
#20601 = CARTESIAN_POINT ( 'NONE',  ( -58.46107188299979640, 0.06432868000574894218, 0.7596429210606043814 ) ) ;
#20602 = CARTESIAN_POINT ( 'NONE',  ( -4.424064652446513257, 118.1653673812831471, 0.4722651929950075766 ) ) ;
#20603 = CARTESIAN_POINT ( 'NONE',  ( 0.6542085308957266143, 106.0197932915460228, -5.259646073629641094 ) ) ;
#20604 = ORIENTED_EDGE ( 'NONE', *, *, #15331, .F. ) ;
#20605 = CARTESIAN_POINT ( 'NONE',  ( -42.79661761208809168, 21.81806929429799879, 2.089873509012810882 ) ) ;
#20606 = CARTESIAN_POINT ( 'NONE',  ( 8.380735907288704212, 119.8444783950307198, -1.107720622939692756 ) ) ;
#20607 = CARTESIAN_POINT ( 'NONE',  ( -0.1506203121293892555, 105.8833743670705445, -5.338473058816376238 ) ) ;
#20608 = AXIS2_PLACEMENT_3D ( 'NONE', #37661, #8690, #8898 ) ;
#20609 = CARTESIAN_POINT ( 'NONE',  ( 4.627536327950492634, 118.0321392792698560, 0.7764583414207147927 ) ) ;
#20610 = CARTESIAN_POINT ( 'NONE',  ( -9.347632431636418104, 123.5785764018267514, -0.8560492856234916959 ) ) ;
#20611 = CARTESIAN_POINT ( 'NONE',  ( -0.5151781122927419077, 115.7029491485453434, -1.762078896387328397 ) ) ;
#20612 = DIRECTION ( 'NONE',  ( -1.000000000000000000, 0.000000000000000000, -1.776356839400250465E-15 ) ) ;
#20613 = EDGE_CURVE ( 'NONE', #11942, #24980, #25088, .T. ) ;
#20614 = CARTESIAN_POINT ( 'NONE',  ( -4.507778648822867495, 31.37953541088120346, -1.025544427737863362 ) ) ;
#20615 = CARTESIAN_POINT ( 'NONE',  ( -10.24488040547501733, 123.7737839053064022, -1.229789271442949472 ) ) ;
#20616 = CARTESIAN_POINT ( 'NONE',  ( -20.21600168833980149, 80.16988503754176065, 1.269999999999995355 ) ) ;
#20617 = AXIS2_PLACEMENT_3D ( 'NONE', #26575, #39802, #23574 ) ;
#20618 = CARTESIAN_POINT ( 'NONE',  ( -45.89458612274084714, 20.88821703128090235, 4.453918368558905883 ) ) ;
#20619 = CARTESIAN_POINT ( 'NONE',  ( 7.903630729593992932, 122.1168884809556232, -0.5501188935066759766 ) ) ;
#20620 = CARTESIAN_POINT ( 'NONE',  ( -11.72060482218064337, 130.2300814166513305, -0.06371650795576043469 ) ) ;
#20621 = DIRECTION ( 'NONE',  ( 4.017660918040594346E-17, -1.000000000000000000, -2.376309959284834438E-19 ) ) ;
#20622 = CARTESIAN_POINT ( 'NONE',  ( 1.940752395788238660, 116.9162416783649689, 0.4172132017389483805 ) ) ;
#20623 = CARTESIAN_POINT ( 'NONE',  ( -4.808149584360944750, 104.6144662015457243, 0.4147572885131461939 ) ) ;
#20624 = CARTESIAN_POINT ( 'NONE',  ( 3.348477204222540138, -14.79883842983281639, 1.177367440313774605 ) ) ;
#20625 = CARTESIAN_POINT ( 'NONE',  ( -7.522503210159361409, 120.3045338523282197, 1.038419263833407546 ) ) ;
#20626 = CARTESIAN_POINT ( 'NONE',  ( -0.9136164112762927836, -2.447138680932527066, -0.3421040304710446511 ) ) ;
#20627 = CARTESIAN_POINT ( 'NONE',  ( -22.36400590086645579, 150.5530013069706285, -1.293239838729947078 ) ) ;
#20628 = AXIS2_PLACEMENT_3D ( 'NONE', #35872, #10076, #9657 ) ;
#20629 = CARTESIAN_POINT ( 'NONE',  ( -0.2091969695887432312, -7.904008462454454431, -0.9542532860826526964 ) ) ;
#20630 = ORIENTED_EDGE ( 'NONE', *, *, #26749, .T. ) ;
#20631 = EDGE_CURVE ( 'NONE', #23570, #27974, #4141, .T. ) ;
#20632 = CARTESIAN_POINT ( 'NONE',  ( -49.58053446479453186, 16.59387910164543456, 4.528212452174703806 ) ) ;
#20633 = CARTESIAN_POINT ( 'NONE',  ( 6.891280466594640330, 121.8252198949890186, 0.2939903263561804425 ) ) ;
#20634 = CARTESIAN_POINT ( 'NONE',  ( -16.05525886874805863, 145.8417561620165372, 0.5351738620951718151 ) ) ;
#20635 = CARTESIAN_POINT ( 'NONE',  ( 2.601617458372238900, -15.08031326607275879, 5.801161347629554044 ) ) ;
#20636 = CARTESIAN_POINT ( 'NONE',  ( 16.16280394421523070, 139.8573806175465961, -1.392748567604541687 ) ) ;
#20637 = ORIENTED_EDGE ( 'NONE', *, *, #10507, .T. ) ;
#20638 = CARTESIAN_POINT ( 'NONE',  ( -12.10717961583478441, 122.5392882283422864, -1.794329550371803972 ) ) ;
#20639 = CARTESIAN_POINT ( 'NONE',  ( 3.600447276656479900, 115.7029491485453150, 1.622454299057154881 ) ) ;
#20640 = CARTESIAN_POINT ( 'NONE',  ( 2.491201389814710065, -14.86453887000410745, 4.964479704013470496 ) ) ;
#20641 = CARTESIAN_POINT ( 'NONE',  ( -4.947191892140043734, 117.5302764761379990, -0.9660299176223910989 ) ) ;
#20642 = CARTESIAN_POINT ( 'NONE',  ( 5.280870373041073762, 121.3253820001177417, -0.01155303659100754415 ) ) ;
#20643 = ORIENTED_EDGE ( 'NONE', *, *, #38355, .F. ) ;
#20644 = EDGE_CURVE ( 'NONE', #42027, #38617, #1974, .T. ) ;
#20645 = CARTESIAN_POINT ( 'NONE',  ( 6.532233579562727321, 157.6773268839678508, 1.915660460402585752 ) ) ;
#20646 = DIRECTION ( 'NONE',  ( -0.9998004120163608288, 0.000000000000000000, -0.01997839162482747608 ) ) ;
#20647 = AXIS2_PLACEMENT_3D ( 'NONE', #22864, #2895, #38875 ) ;
#20648 = CARTESIAN_POINT ( 'NONE',  ( -17.32429653712378936, 61.56493206124108042, -1.523999999999999355 ) ) ;
#20649 = CARTESIAN_POINT ( 'NONE',  ( 12.21488373879589062, 56.36092316367926003, 5.016499999999999737 ) ) ;
#20650 = AXIS2_PLACEMENT_3D ( 'NONE', #6074, #13502, #3513 ) ;
#20651 = CARTESIAN_POINT ( 'NONE',  ( 5.733252156539616173, 159.1225378944267845, -0.03759195597257673077 ) ) ;
#20652 = EDGE_CURVE ( 'NONE', #1790, #3203, #6480, .T. ) ;
#20653 = CARTESIAN_POINT ( 'NONE',  ( 6.059261036833980540, 78.87450423423040036, -5.016499999999999737 ) ) ;
#20654 = AXIS2_PLACEMENT_3D ( 'NONE', #3550, #26309, #355 ) ;
#20655 = EDGE_CURVE ( 'NONE', #15693, #24814, #7413, .T. ) ;
#20656 = CARTESIAN_POINT ( 'NONE',  ( 1.793193054604032222, -15.65090912328376227, 5.542963820967112376 ) ) ;
#20657 = DIRECTION ( 'NONE',  ( 1.000000000000000000, -1.177520686924251719E-16, 0.000000000000000000 ) ) ;
#20658 = CARTESIAN_POINT ( 'NONE',  ( -8.095114962461808616, 74.19100168833409725, -1.269999999999996687 ) ) ;
#20659 = CARTESIAN_POINT ( 'NONE',  ( 19.59170213216421175, 150.6586468064772646, 2.354958926090490845 ) ) ;
#20660 = ORIENTED_EDGE ( 'NONE', *, *, #20697, .F. ) ;
#20661 = CARTESIAN_POINT ( 'NONE',  ( -2.821688713678647709, 20.15627898171042176, -7.936949992814660071 ) ) ;
#20662 = CARTESIAN_POINT ( 'NONE',  ( -2.408872516888110216, 117.3686073472606921, -0.7136685935690528781 ) ) ;
#20663 = CARTESIAN_POINT ( 'NONE',  ( -2.259516459295737079, 118.2243428780609662, -0.9293431707136510234 ) ) ;
#20664 = AXIS2_PLACEMENT_3D ( 'NONE', #36716, #24124, #37544 ) ;
#20666 = CARTESIAN_POINT ( 'NONE',  ( -5.714078020758869059, 78.90256189635195483, 5.042866571093570727 ) ) ;
#20665 = AXIS2_PLACEMENT_3D ( 'NONE', #12738, #32128, #35751 ) ;
#20667 = DIRECTION ( 'NONE',  ( -0.8745520943968243532, 0.4849315768086547296, -6.829619984160642269E-16 ) ) ;
#20668 = CARTESIAN_POINT ( 'NONE',  ( -0.01254005783143666460, 120.1716774721351157, 0.6275557724548824767 ) ) ;
#20669 = CARTESIAN_POINT ( 'NONE',  ( 2.551540157903699146, -0.3564265548712530207, -3.854280124997286450 ) ) ;
#20670 = CARTESIAN_POINT ( 'NONE',  ( -46.95911617132933458, 24.98948415085536823, -1.986615011824472088 ) ) ;
#20671 = CARTESIAN_POINT ( 'NONE',  ( -4.792324638262704717, 56.51998046905272588, -4.972049999962482758 ) ) ;
#20672 = CARTESIAN_POINT ( 'NONE',  ( 3.381076509412870301, -13.31623885458479961, 2.121725202727857695 ) ) ;
#20673 = CARTESIAN_POINT ( 'NONE',  ( 5.132724724882859135, 121.7269124416356192, -0.09984968675566523177 ) ) ;
#20674 = CARTESIAN_POINT ( 'NONE',  ( -8.141728797601244239, 117.8329967196738153, 0.4384511054415166087 ) ) ;
#20675 = EDGE_CURVE ( 'NONE', #23570, #12906, #31517, .T. ) ;
#20676 = CARTESIAN_POINT ( 'NONE',  ( -2.501798531443050422, 32.04972782698715861, 4.390535724770350257 ) ) ;
#20677 = DIRECTION ( 'NONE',  ( 0.7548010569845196027, 0.6559537821943342006, 6.697925912855741462E-15 ) ) ;
#20678 = EDGE_LOOP ( 'NONE', ( #31232, #21232, #11573, #2656 ) ) ;
#20679 = CARTESIAN_POINT ( 'NONE',  ( -4.842539706364327401, 104.6144662015370272, -2.263382849314995671 ) ) ;
#20680 = AXIS2_PLACEMENT_3D ( 'NONE', #40155, #13527, #20522 ) ;
#20681 = CARTESIAN_POINT ( 'NONE',  ( 4.270102617218862306, -15.70017440876955739, 3.434341872514240723 ) ) ;
#20682 = CARTESIAN_POINT ( 'NONE',  ( -14.84283187390168379, 125.6006210965460781, 1.448481940162723358 ) ) ;
#20683 = CARTESIAN_POINT ( 'NONE',  ( -2.070226828232369254, -8.352695179381779411, -4.151654383260235726 ) ) ;
#20684 = ORIENTED_EDGE ( 'NONE', *, *, #2411, .F. ) ;
#20685 = VERTEX_POINT ( 'NONE', #529 ) ;
#20686 = CARTESIAN_POINT ( 'NONE',  ( -10.44685452804831804, 82.62549350906336088, -1.523999999999999355 ) ) ;
#20687 = CARTESIAN_POINT ( 'NONE',  ( 3.074626428557167390, 123.1875568577169560, 0.1788317054798709282 ) ) ;
#20688 = FILL_AREA_STYLE ('',( #23455 ) ) ;
#20689 = CARTESIAN_POINT ( 'NONE',  ( -11.70197428064591527, 126.1299551460304542, 0.9179571146301048756 ) ) ;
#20690 = CARTESIAN_POINT ( 'NONE',  ( -46.44929277073200069, 20.74717582246854874, 4.783910118526112143 ) ) ;
#20691 =( BOUNDED_SURFACE ( )  B_SPLINE_SURFACE ( 3, 3, ( 
 ( #23933, #7770, #26511, #20733, #16702, #33757, #7145, #1173, #39943, #3956, #14136, #966, #4583, #30543, #29917, #756, #20307, #20102, #26725, #27138, #40362, #549, #33126, #10532, #10735, #23501, #36528, #26931, #33333, #4163, #31597, #11365, #41190, #5000, #34172, #14552, #27971, #15394, #12212, #28400, #2433, #41405, #24773, #21559, #27762, #25202, #21143, #21350, #34587, #17958, #18371, #2007, #40981, #24988, #11570, #34375, #37560, #40772, #30958, #24556, #5416, #38206, #1798, #8812, #18163, #28185, #31166, #37988, #37771, #11993, #21986, #14761, #9023, #4794, #34797, #8386, #40567, #11783, #5630, #17745, #8176, #5208, #24351, #27560, #14969, #30745, #8595, #31378, #2222, #21771, #15182, #18588, #1595, #37357, #32229, #71, #25418, #26241, #28608, #3060, #41617, #12426, #26030, #3263, #38419, #38626, #39039, #10057, #13257, #19426, #39250, #18793, #5840, #16017, #35019, #22398, #31806, #9846, #29445, #3479, #2643, #28818, #15603, #29016, #9231, #35422, #22189, #22814, #284, #16438, #35219, #41833, #6045, #19007, #32011, #32432, #2850, #15811, #16223, #13040, #12627, #35851, #25615, #29230, #9428, #6665, #42036, #6249, #38828, #19218, #19628, #32643, #12832, #25819, #9638, #22606, #35638, #6453, #33496, #17492, #1120, #17290, #17074, #30488, #32858, #33284, #39888, #27090, #7719, #29658, #30279, #23237, #10265, #3690, #4114, #33707, #1331, #4528, #20683, #14289, #913, #10685, #3904, #27299, #39463, #39677, #23666, #36272, #36686, #20257, #30076, #14089, #29868, #10480, #13678, #16867, #7092, #707 ),
 ( #36477, #40098, #13887, #4326, #40313, #33073, #23028, #36058, #10894, #20054, #16651, #26880, #23882, #6872, #26459, #26669, #498, #13471, #23449, #19845, #7297, #7508, #20469, #36901, #4947, #31326, #7923, #4741, #8334, #18323, #1543, #2383, #17694, #21304, #30694, #14498, #2170, #21509, #27513, #14709, #15128, #28348, #31539, #37726, #15343, #37105, #40521, #24722, #34333, #5161, #28131, #17907, #40722, #1750, #34121, #11312, #30911, #27921, #18534, #24299, #41141, #24503, #34543, #37509, #11947, #31120, #5369, #11107, #21096, #24096, #37936, #24938, #37305, #8122, #18116, #8761, #21721, #27713, #11518, #1957, #20889, #14917, #33913, #40928, #11733, #8550, #34746, #5578, #19374, #38155, #34965, #38570, #6405, #31754, #32589, #5788, #9382, #18743, #2596, #32380, #9588, #15556, #2802, #3211, #16389, #19581, #25770, #3422, #25153, #12160, #22346, #41357, #28765, #8969, #16171, #35798, #9799, #21936, #35168, #28558, #41567, #12376, #38777, #22766, #25363, #22558, #29176, #38367, #22, #6612, #35588, #9181, #12988, #35369, #22138, #3008, #41778, #25982, #38990, #5995, #18957, #31963, #15762, #12578, #6199, #25565, #19170, #32174, #15967, #28965, #41982, #12780, #39626, #4067, #33447, #14040, #36007, #23619, #29612, #16604, #39198, #10432, #40053, #36853, #10846, #27045, #23832, #7252, #17026, #10214, #7671, #3640, #3854, #30024, #20008, #33658, #20629, #22978, #865, #4483, #29395, #29821, #20212, #235, #33238, #659, #13211, #13838, #26193, #6819, #447, #26618, #10006, #19789, #32809, #26835, #39842, #13419 ),
 ( #23402, #26407, #33025, #39411, #23184, #10639, #36639, #36433, #13627, #7461, #20420, #4275, #17238, #30233, #16819, #36220, #1072, #7041, #5114, #15080, #17860, #40676, #34489, #34695, #27251, #11266, #17650, #11468, #31069, #30860, #2117, #1706, #24670, #8501, #21052, #20841, #11683, #37679, #8079, #40267, #8710, #14453, #28081, #5320, #14660, #34286, #18272, #14871, #37060, #41092, #30652, #17443, #21458, #27464, #40475, #27664, #11899, #33866, #24888, #7878, #1286, #37885, #14244, #21672, #40882, #27873, #30441, #11062, #8286, #24457, #31274, #24046, #18067, #4695, #34078, #24252, #1496, #37260, #37461, #4905, #21256, #1908, #6940, #19487, #5742, #9906, #10121, #25309, #18694, #28508, #15292, #3324, #3545, #23092, #13535, #32496, #16291, #41304, #13319, #29295, #138, #29513, #26305, #39314, #13105, #26097, #9134, #12109, #39103, #12322, #35916, #3757, #6512, #22878, #36126, #23303, #28297, #41516, #31704, #6726, #19694, #32711, #32927, #16506, #19911, #16715, #22668, #8917, #352, #29718, #38315, #25099, #39529, #2546, #560, #26523, #10333, #5525, #18482, #31488, #38102, #2333, #15507, #21883, #34910, #35701, #36539, #39953, #27358, #26736, #30552, #766, #7156, #1391, #20115, #11166, #40161, #27149, #37159, #40370, #20529, #13944, #10954, #23941, #4392, #24150, #17136, #20317, #10543, #23512, #33558, #33344, #7358, #36958, #4592, #26942, #4174, #17348, #7781, #30138, #979, #10747, #33137, #23728, #20742, #33767, #36341, #7568, #36747, #39745, #30336, #3967, #16928, #1183, #17551, #29928, #13742, #14146 ),
 ( #14347, #10243, #39654, #13448, #38805, #16631, #13237, #19405, #36035, #32621, #23214, #20032, #3242, #32412, #22793, #9617, #16201, #39225, #475, #26646, #36247, #26436, #684, #23428, #39440, #7068, #28996, #33051, #10458, #3881, #22585, #29638, #26221, #29206, #6850, #3454, #16846, #29846, #49, #13015, #35828, #35617, #26009, #10035, #13656, #36457, #7276, #32206, #23007, #3039, #42013, #263, #19819, #15997, #12809, #6431, #25799, #39018, #9826, #6644, #32836, #19608, #16416, #29422, #3665, #3713, #17309, #7113, #13493, #36496, #26898, #26693, #40118, #39700, #20486, #4347, #16885, #16672, #7525, #33513, #3925, #36082, #4551, #10289, #10912, #1141, #13699, #30095, #30298, #10704, #32881, #23901, #26479, #13277, #14107, #23259, #36294, #10500, #7736, #29677, #36918, #520, #39271, #20702, #10077, #17511, #36704, #23683, #30508, #33728, #4133, #23470, #27106, #26261, #936, #23048, #29886, #20072, #39483, #33094, #33303, #724, #7316, #6896, #19866, #20276, #17092, #13906, #39910, #21115, #14522, #24322, #11126, #40743, #40950, #5389, #8785, #27732, #14730, #37121, #34141, #5602, #11967, #7943, #1978, #41161, #37960, #1770, #21322, #14306, #31139, #17715, #14940, #11540, #37529, #21530, #8144, #30931, #4968, #37328, #30714, #17926, #18134, #21743, #1566, #18344, #24524, #24743, #8354, #34562, #34350, #37745, #18557, #11334, #34769, #28155, #31350, #27532, #20912, #5182, #2193, #24959, #4763, #40539, #33935, #24113, #27942, #1349, #11755, #8569, #15151, #27319, #40332, #10179, #28370, #25176, #28789, #39377 ),
 ( #23148, #413, #38177, #35190, #36187, #7218, #10396, #16568, #23368, #15364, #2404, #41801, #36401, #18980, #31563, #7006, #26582, #624, #41377, #25387, #18766, #12183, #8991, #29578, #13593, #21959, #13382, #19975, #34989, #32991, #39592, #26369, #5810, #3819, #12599, #31775, #35390, #31984, #16782, #29785, #2616, #15576, #22160, #28581, #41589, #38593, #12397, #38390, #9201, #6016, #25586, #2822, #15781, #9401, #6784, #22365, #19752, #32774, #3604, #20382, #7424, #29987, #1254, #30823, #27627, #1669, #37224, #8043, #30199, #14209, #1039, #14624, #36605, #36815, #4239, #40639, #11433, #33408, #17825, #27216, #16987, #23794, #37426, #17201, #30615, #27424, #30405, #4451, #1458, #40437, #11228, #40230, #17409, #7634, #26800, #33622, #27010, #7841, #24421, #20592, #24214, #4029, #10602, #21016, #14004, #40019, #11025, #33830, #24006, #4867, #37026, #34039, #20179, #20804, #23582, #14417, #33203, #10813, #827, #13802, #4658, #39809, #17614, #8673, #25061, #25276, #5707, #27838, #5914, #8469, #8247, #28477, #5285, #18235, #34660, #2721, #24633, #18876, #40846, #34249, #31885, #5079, #41691, #31670, #18664, #25493, #15678, #41269, #21634, #2511, #15475, #38065, #28682, #41055, #31237, #21424, #34452, #28261, #15044, #2080, #41481, #9099, #5488, #28046, #12074, #12289, #11865, #24854, #37851, #18029, #18448, #38281, #22065, #12501, #31454, #2298, #1872, #15258, #21219, #31031, #14834, #8882, #11648, #37643, #21846, #34874, #35091, #29316, #9721, #23109, #158, #29739, #2926, #38702, #35720, #16735, #35295, #6123 ),
 ( #9509, #6528, #580, #19088, #32091, #13128, #26118, #32948, #15888, #22478, #3777, #13552, #35506, #36145, #32515, #28892, #42118, #38490, #25696, #6745, #3564, #19504, #22686, #19713, #16525, #29534, #3346, #16312, #12911, #41906, #39121, #3132, #9927, #6960, #38909, #370, #22271, #12706, #13336, #32302, #6325, #22896, #35933, #32733, #19931, #26325, #39331, #10138, #25903, #19296, #9309, #16093, #29099, #7175, #17772, #23533, #24166, #14366, #26961, #1203, #1410, #23959, #3986, #37176, #26756, #26542, #4612, #36560, #7376, #10767, #20968, #784, #7999, #16946, #10352, #33990, #23324, #30770, #7798, #36977, #1619, #4818, #17366, #39974, #20760, #33784, #14163, #39549, #17156, #20336, #39766, #10560, #4409, #33361, #4194, #17567, #27376, #23747, #30156, #30355, #30570, #997, #13961, #36766, #36359, #7585, #40386, #11181, #20135, #20546, #33575, #33158, #27170, #29944, #13759, #40181, #10975, #12234, #9045, #14994, #34609, #27580, #5438, #27994, #41427, #18396, #17982, #8833, #21795, #5230, #37381, #5861, #11595, #25225, #2456, #41002, #31405, #31617, #12018, #34199, #38230, #14783, #14575, #34823, #24578, #37584, #11808, #22011, #30979, #35041, #5024, #40588, #18821, #11388, #31828, #38011, #25011, #24373, #8196, #2246, #24799, #5656, #18612, #15205, #21167, #18185, #8412, #27785, #40795, #28208, #21371, #34397, #15419, #28422, #37793, #31186, #41216, #1819, #2031, #8619, #21581, #12448, #42062, #98, #6688, #10080, #29044, #16042, #38441, #35449, #6900, #13280, #9256, #3288, #312, #39274, #3082, #22629 ),
 ( #22838, #23052, #26055, #22213, #29253, #25843, #32036, #6475, #12856, #35877, #32670, #15835, #2873, #6272, #35243, #28842, #9663, #13064, #36086, #19655, #39066, #38852, #19869, #25442, #35665, #19450, #3505, #29470, #6068, #9868, #41855, #12652, #19030, #32459, #26264, #2665, #15624, #16463, #28628, #25641, #16249, #38648, #41641, #9454, #19243, #22421, #32253, #4351, #30099, #26901, #4136, #40123, #23907, #36499, #36297, #27111, #10917, #23474, #13496, #24117, #29889, #30514, #20707, #33306, #7529, #7740, #30302, #10294, #1353, #33098, #32884, #36922, #727, #13704, #17096, #27325, #7118, #14312, #23262, #16676, #40336, #29680, #37126, #14112, #1144, #7947, #11130, #23688, #939, #33732, #4555, #20490, #3717, #7320, #26697, #3928, #16888, #10708, #39703, #10504, #17515, #523, #13909, #20279, #36707, #26482, #39914, #33516, #17312, #39487, #20075, #18349, #24964, #28376, #5186, #34354, #14527, #11544, #25181, #31570, #27536, #21536, #18563, #15370, #21327, #40955, #33939, #11760, #18139, #5607, #24749, #12188, #40543, #21119, #31143, #41383, #17719, #30720, #37749, #8573, #38182, #11340, #4973, #20916, #4767, #34147, #2409, #14944, #1570, #24528, #24326, #8148, #31354, #28161, #1983, #27946, #2198, #41165, #11971, #34566, #5393, #37535, #37332, #15156, #27737, #37964, #17932, #8789, #21747, #30935, #1774, #34774, #14735, #40747, #8359, #22582, #22372, #35825, #9207, #8999, #29202, #6022, #18985, #35397, #3450, #25395, #6641, #28586, #34995, #19605, #5815, #259, #32409, #19401, #26217, #16413, #42009, #9406 ) ),
 .UNSPECIFIED., .T., .F., .T. ) 
 B_SPLINE_SURFACE_WITH_KNOTS ( ( 4, 3, 4 ),
 ( 4, 1, 1, 1, 1, 1, 1, 1, 1, 1, 1, 1, 1, 1, 1, 1, 1, 1, 1, 1, 1, 1, 1, 1, 1, 1, 1, 1, 1, 1, 1, 1, 1, 1, 1, 1, 1, 1, 1, 1, 1, 1, 1, 1, 1, 1, 1, 1, 1, 1, 1, 1, 1, 1, 1, 1, 1, 1, 1, 1, 1, 1, 1, 1, 1, 1, 1, 1, 1, 1, 1, 1, 1, 1, 1, 1, 1, 1, 1, 1, 1, 1, 1, 1, 1, 1, 1, 1, 1, 1, 1, 1, 1, 1, 1, 1, 1, 1, 1, 1, 1, 1, 1, 1, 1, 1, 1, 1, 1, 1, 1, 1, 1, 1, 1, 1, 1, 1, 1, 1, 1, 1, 1, 1, 1, 1, 1, 1, 1, 1, 1, 1, 1, 1, 1, 1, 1, 1, 1, 1, 1, 1, 1, 1, 1, 1, 1, 1, 1, 1, 1, 1, 1, 1, 1, 1, 1, 1, 1, 1, 1, 1, 1, 1, 1, 1, 1, 1, 1, 1, 1, 1, 1, 1, 1, 1, 1, 1, 1, 1, 1, 1, 1, 1, 1, 1, 1, 1, 1, 1, 1, 1, 3, 4 ),
 ( 0.000000000000000000, 0.5000000000000000000, 1.000000000000000000 ),
 ( 0.000000000000000000, 0.007812500000000423273, 0.01388888888888889506, 0.01562500000000000000, 0.02343749999999998959, 0.02777777777777778317, 0.03125000000000092981, 0.03906249999999999306, 0.04166666666666667823, 0.04687500000000000000, 0.05468749999999999306, 0.05555555555555556635, 0.06249999999999997918, 0.06944444444444446141, 0.07031250000000000000, 0.07812500000000000000, 0.08333333333333334259, 0.08593749999999998612, 0.09374999999999603095, 0.09722222222222223764, 0.1015625000000000139, 0.1093750000000000000, 0.1111111111111111188, 0.1171875000000000000, 0.1250000000000000000, 0.1328125000000000000, 0.1388888888888889228, 0.1406250000000000000, 0.1484375000000000000, 0.1527777777777778179, 0.1562500000000039690, 0.1640625000000000000, 0.1666666666666666852, 0.1718750000000000000, 0.1796875000000000000, 0.1805555555555555802, 0.1875000000000000000, 0.1944444444444444753, 0.1953125000000000000, 0.2031250000000000000, 0.2083333333333333703, 0.2109375000000000000, 0.2187499999999960310, 0.2222222222222222376, 0.2265625000000000000, 0.2343750000000000000, 0.2361111111111111327, 0.2421875000000000000, 0.2500000000000000000, 0.2578125000000000000, 0.2638888888888888951, 0.2656250000000000000, 0.2734375000000000000, 0.2777777777777777346, 0.2812500000000039968, 0.2890625000000000000, 0.2916666666666665741, 0.2968750000000000000, 0.3046875000000000000, 0.3055555555555554692, 0.3125000000000000000, 0.3194444444444443088, 0.3203125000000000000, 0.3281250000000000000, 0.3333333333333332038, 0.3359375000000000000, 0.3437499999999960587, 0.3472222222222220434, 0.3515625000000000000, 0.3593750000000000000, 0.3611111111111109384, 0.3671875000000000000, 0.3750000000000000000, 0.3828125000000000000, 0.3888888888888886175, 0.3906250000000000000, 0.3984375000000000000, 0.4027777777777775126, 0.4062500000000039968, 0.4140625000000000000, 0.4166666666666663521, 0.4218750000000000000, 0.4296875000000000000, 0.4305555555555552472, 0.4375000000000000000, 0.4444444444444440867, 0.4453125000000000000, 0.4531250000000000000, 0.4583333333333329818, 0.4609375000000000000, 0.4687499999999960587, 0.4722222222222218768, 0.4765625000000000000, 0.4843750000000000000, 0.4861111111111107719, 0.4921875000000000000, 0.5000000000000000000, 0.5078125000000000000, 0.5138888888888886175, 0.5156250000000000000, 0.5234375000000000000, 0.5277777777777775681, 0.5312500000000039968, 0.5390625000000000000, 0.5416666666666664076, 0.5468750000000000000, 0.5546875000000000000, 0.5555555555555553582, 0.5625000000000000000, 0.5694444444444443088, 0.5703125000000000000, 0.5781250000000000000, 0.5833333333333331483, 0.5859375000000000000, 0.5937499999999960032, 0.5972222222222220989, 0.6015625000000000000, 0.6093750000000000000, 0.6111111111111110494, 0.6171875000000000000, 0.6250000000000000000, 0.6328125000000000000, 0.6388888888888888395, 0.6406250000000000000, 0.6484375000000000000, 0.6527777777777777901, 0.6562500000000039968, 0.6640625000000000000, 0.6666666666666666297, 0.6718750000000000000, 0.6796875000000000000, 0.6805555555555555802, 0.6875000000000000000, 0.6944444444444445308, 0.6953125000000000000, 0.7031250000000000000, 0.7083333333333333703, 0.7109375000000000000, 0.7187499999999960032, 0.7222222222222223209, 0.7265625000000000000, 0.7343750000000000000, 0.7361111111111111605, 0.7421875000000000000, 0.7500000000000000000, 0.7578125000000000000, 0.7638888888888889506, 0.7656250000000000000, 0.7734375000000000000, 0.7777777777777779011, 0.7812500000000039968, 0.7890625000000000000, 0.7916666666666668517, 0.7968750000000000000, 0.8046875000000000000, 0.8055555555555556912, 0.8125000000000000000, 0.8194444444444446418, 0.8203125000000000000, 0.8281250000000000000, 0.8333333333333335924, 0.8359375000000000000, 0.8437499999999960032, 0.8472222222222224319, 0.8515625000000000000, 0.8593750000000000000, 0.8611111111111113825, 0.8671875000000000000, 0.8750000000000000000, 0.8828125000000000000, 0.8888888888888891726, 0.8906250000000000000, 0.8984375000000000000, 0.9027777777777781232, 0.9062500000000039968, 0.9140625000000000000, 0.9166666666666670737, 0.9218750000000000000, 0.9296875000000000000, 0.9305555555555559133, 0.9375000000000000000, 0.9444444444444447528, 0.9453125000000000000, 0.9531250000000000000, 0.9583333333333335924, 0.9609375000000000000, 0.9687499999999991118, 0.9722222222222224319, 0.9765625000000000000, 0.9843750000000000000, 0.9861111111111111605, 0.9921874999999995559, 1.000000000000000000, 1.000012325855852646 ),
 .UNSPECIFIED. ) 
 GEOMETRIC_REPRESENTATION_ITEM ( )  RATIONAL_B_SPLINE_SURFACE ( (
 ( 1.000000000000000000, 1.000000000000000000, 1.000000000000000000, 1.000000000000000000, 1.000000000000000000, 1.000000000000000000, 0.9999999999999998890, 0.9999999999999997780, 1.000000000000000000, 1.000000000000000000, 1.000000000000000000, 1.000000000000000000, 1.000000000000000000, 1.000000000000000000, 0.9999999999999998890, 1.000000000000000000, 1.000000000000000222, 1.000000000000000000, 1.000000000000000000, 1.000000000000000000, 1.000000000000000000, 1.000000000000000000, 0.9999999999999998890, 0.9999999999999997780, 1.000000000000000000, 1.000000000000000222, 1.000000000000000000, 1.000000000000000000, 1.000000000000000000, 1.000000000000000000, 0.9999999999999998890, 0.9999999999999997780, 1.000000000000000000, 0.9999999999999998890, 0.9999999999999997780, 1.000000000000000000, 1.000000000000000222, 1.000000000000000222, 1.000000000000000000, 1.000000000000000000, 1.000000000000000222, 1.000000000000000000, 0.9999999999999997780, 1.000000000000000000, 1.000000000000000000, 1.000000000000000000, 1.000000000000000000, 1.000000000000000000, 1.000000000000000000, 1.000000000000000222, 1.000000000000000222, 1.000000000000000000, 1.000000000000000000, 1.000000000000000222, 1.000000000000000222, 1.000000000000000222, 1.000000000000000000, 1.000000000000000000, 1.000000000000000222, 1.000000000000000000, 1.000000000000000000, 1.000000000000000222, 1.000000000000000000, 1.000000000000000000, 1.000000000000000222, 1.000000000000000000, 1.000000000000000000, 0.9999999999999997780, 0.9999999999999998890, 1.000000000000000000, 1.000000000000000000, 1.000000000000000000, 1.000000000000000000, 1.000000000000000222, 1.000000000000000222, 1.000000000000000000, 1.000000000000000000, 1.000000000000000222, 1.000000000000000222, 1.000000000000000222, 1.000000000000000000, 1.000000000000000000, 1.000000000000000222, 1.000000000000000000, 1.000000000000000000, 1.000000000000000222, 1.000000000000000000, 1.000000000000000000, 1.000000000000000222, 1.000000000000000000, 1.000000000000000000, 0.9999999999999997780, 0.9999999999999998890, 1.000000000000000000, 1.000000000000000000, 1.000000000000000000, 1.000000000000000000, 1.000000000000000222, 1.000000000000000222, 1.000000000000000000, 1.000000000000000000, 1.000000000000000222, 1.000000000000000222, 1.000000000000000222, 1.000000000000000000, 1.000000000000000000, 1.000000000000000222, 1.000000000000000000, 0.9999999999999998890, 1.000000000000000222, 1.000000000000000000, 1.000000000000000000, 1.000000000000000222, 1.000000000000000000, 1.000000000000000000, 1.000000000000000222, 1.000000000000000000, 1.000000000000000000, 1.000000000000000000, 1.000000000000000000, 1.000000000000000000, 1.000000000000000222, 1.000000000000000222, 1.000000000000000000, 1.000000000000000000, 1.000000000000000222, 1.000000000000000222, 1.000000000000000222, 1.000000000000000000, 1.000000000000000222, 1.000000000000000222, 1.000000000000000000, 1.000000000000000000, 1.000000000000000222, 1.000000000000000000, 1.000000000000000000, 1.000000000000000222, 1.000000000000000000, 1.000000000000000000, 1.000000000000000222, 1.000000000000000222, 1.000000000000000000, 1.000000000000000000, 1.000000000000000222, 1.000000000000000000, 1.000000000000000222, 1.000000000000000222, 1.000000000000000000, 1.000000000000000000, 1.000000000000000222, 1.000000000000000222, 1.000000000000000222, 1.000000000000000000, 1.000000000000000000, 1.000000000000000222, 1.000000000000000000, 0.9999999999999998890, 1.000000000000000222, 1.000000000000000000, 1.000000000000000000, 1.000000000000000222, 1.000000000000000000, 1.000000000000000000, 1.000000000000000222, 1.000000000000000000, 1.000000000000000000, 1.000000000000000000, 1.000000000000000000, 1.000000000000000000, 1.000000000000000222, 1.000000000000000222, 1.000000000000000000, 1.000000000000000000, 1.000000000000000222, 1.000000000000000222, 1.000000000000000222, 1.000000000000000000, 1.000000000000000000, 1.000000000000000222, 1.000000000000000000, 1.000000000000000000, 1.000000000000000222, 1.000000000000000000, 1.000000000000000000, 1.000000000000000222, 1.000000000000000000, 0.9999999999999996669, 0.9999999999999996669, 1.000000000000000000, 1.000000000000000222, 1.000000000000000000, 1.000000000000000000, 1.000000000000000000, 1.000000000000000000, 1.000000000000000000, 1.000000000000000000, 1.000000000000000000, 1.000000000000000000),
 ( 0.3333333333333333703, 0.3333333333333333703, 0.3333333333333333703, 0.3333333333333334259, 0.3333333333333334259, 0.3333333333333334259, 0.3333333333333333703, 0.3333333333333333148, 0.3333333333333333703, 0.3333333333333333703, 0.3333333333333333148, 0.3333333333333333703, 0.3333333333333333703, 0.3333333333333334814, 0.3333333333333333703, 0.3333333333333333703, 0.3333333333333334259, 0.3333333333333333703, 0.3333333333333333148, 0.3333333333333333703, 0.3333333333333333703, 0.3333333333333333703, 0.3333333333333333703, 0.3333333333333333703, 0.3333333333333333148, 0.3333333333333334259, 0.3333333333333333703, 0.3333333333333333703, 0.3333333333333333703, 0.3333333333333334259, 0.3333333333333333703, 0.3333333333333333703, 0.3333333333333333703, 0.3333333333333333703, 0.3333333333333333148, 0.3333333333333333703, 0.3333333333333334259, 0.3333333333333333703, 0.3333333333333333703, 0.3333333333333333703, 0.3333333333333333703, 0.3333333333333333703, 0.3333333333333333703, 0.3333333333333333703, 0.3333333333333333703, 0.3333333333333333148, 0.3333333333333333703, 0.3333333333333333703, 0.3333333333333333703, 0.3333333333333334259, 0.3333333333333333703, 0.3333333333333333703, 0.3333333333333333703, 0.3333333333333333703, 0.3333333333333333703, 0.3333333333333334259, 0.3333333333333333703, 0.3333333333333333703, 0.3333333333333333703, 0.3333333333333333703, 0.3333333333333334259, 0.3333333333333333703, 0.3333333333333333703, 0.3333333333333333703, 0.3333333333333333703, 0.3333333333333333703, 0.3333333333333333703, 0.3333333333333333148, 0.3333333333333333148, 0.3333333333333333148, 0.3333333333333333703, 0.3333333333333333703, 0.3333333333333333148, 0.3333333333333334259, 0.3333333333333333703, 0.3333333333333333703, 0.3333333333333333703, 0.3333333333333333703, 0.3333333333333333703, 0.3333333333333333703, 0.3333333333333333703, 0.3333333333333333703, 0.3333333333333333703, 0.3333333333333334259, 0.3333333333333334259, 0.3333333333333333703, 0.3333333333333333703, 0.3333333333333333703, 0.3333333333333333703, 0.3333333333333333703, 0.3333333333333333703, 0.3333333333333333703, 0.3333333333333333148, 0.3333333333333333148, 0.3333333333333333703, 0.3333333333333333703, 0.3333333333333333148, 0.3333333333333334259, 0.3333333333333333703, 0.3333333333333333703, 0.3333333333333333703, 0.3333333333333333703, 0.3333333333333333703, 0.3333333333333333703, 0.3333333333333333703, 0.3333333333333333703, 0.3333333333333333703, 0.3333333333333333703, 0.3333333333333333703, 0.3333333333333333148, 0.3333333333333333703, 0.3333333333333333703, 0.3333333333333333703, 0.3333333333333333703, 0.3333333333333333148, 0.3333333333333333703, 0.3333333333333333703, 0.3333333333333333148, 0.3333333333333333703, 0.3333333333333333703, 0.3333333333333333148, 0.3333333333333334259, 0.3333333333333333703, 0.3333333333333333703, 0.3333333333333333703, 0.3333333333333333703, 0.3333333333333333703, 0.3333333333333334259, 0.3333333333333333703, 0.3333333333333333703, 0.3333333333333334259, 0.3333333333333334259, 0.3333333333333334259, 0.3333333333333333703, 0.3333333333333333703, 0.3333333333333333703, 0.3333333333333333703, 0.3333333333333333703, 0.3333333333333333703, 0.3333333333333333703, 0.3333333333333333703, 0.3333333333333333703, 0.3333333333333334259, 0.3333333333333333703, 0.3333333333333333148, 0.3333333333333334259, 0.3333333333333333703, 0.3333333333333333703, 0.3333333333333333703, 0.3333333333333333703, 0.3333333333333333703, 0.3333333333333334259, 0.3333333333333333703, 0.3333333333333333703, 0.3333333333333333703, 0.3333333333333334259, 0.3333333333333333703, 0.3333333333333333703, 0.3333333333333333703, 0.3333333333333333703, 0.3333333333333333703, 0.3333333333333333703, 0.3333333333333333148, 0.3333333333333334259, 0.3333333333333333703, 0.3333333333333333148, 0.3333333333333333703, 0.3333333333333333703, 0.3333333333333333703, 0.3333333333333334259, 0.3333333333333333703, 0.3333333333333333703, 0.3333333333333333703, 0.3333333333333333703, 0.3333333333333333703, 0.3333333333333334259, 0.3333333333333333703, 0.3333333333333333703, 0.3333333333333333703, 0.3333333333333333703, 0.3333333333333334259, 0.3333333333333333703, 0.3333333333333333703, 0.3333333333333333703, 0.3333333333333333703, 0.3333333333333333703, 0.3333333333333333703, 0.3333333333333333148, 0.3333333333333333703, 0.3333333333333333703, 0.3333333333333333703, 0.3333333333333333703, 0.3333333333333333148, 0.3333333333333333703, 0.3333333333333333703, 0.3333333333333333703, 0.3333333333333333703, 0.3333333333333333703),
 ( 0.3333333333333333703, 0.3333333333333333703, 0.3333333333333333703, 0.3333333333333334259, 0.3333333333333334259, 0.3333333333333334259, 0.3333333333333333703, 0.3333333333333333148, 0.3333333333333333703, 0.3333333333333333703, 0.3333333333333333148, 0.3333333333333333703, 0.3333333333333333703, 0.3333333333333334814, 0.3333333333333333703, 0.3333333333333333703, 0.3333333333333334259, 0.3333333333333333703, 0.3333333333333333148, 0.3333333333333333703, 0.3333333333333333703, 0.3333333333333333703, 0.3333333333333333703, 0.3333333333333333703, 0.3333333333333333148, 0.3333333333333334259, 0.3333333333333333703, 0.3333333333333333703, 0.3333333333333333703, 0.3333333333333334259, 0.3333333333333333703, 0.3333333333333333703, 0.3333333333333333703, 0.3333333333333333703, 0.3333333333333333148, 0.3333333333333333703, 0.3333333333333334259, 0.3333333333333333703, 0.3333333333333333703, 0.3333333333333333703, 0.3333333333333333703, 0.3333333333333333703, 0.3333333333333333703, 0.3333333333333333703, 0.3333333333333333703, 0.3333333333333333148, 0.3333333333333333703, 0.3333333333333333703, 0.3333333333333333703, 0.3333333333333334259, 0.3333333333333333703, 0.3333333333333333703, 0.3333333333333333703, 0.3333333333333333703, 0.3333333333333333703, 0.3333333333333334259, 0.3333333333333333703, 0.3333333333333333703, 0.3333333333333333703, 0.3333333333333333703, 0.3333333333333334259, 0.3333333333333333703, 0.3333333333333333703, 0.3333333333333333703, 0.3333333333333333703, 0.3333333333333333703, 0.3333333333333333703, 0.3333333333333333148, 0.3333333333333333148, 0.3333333333333333148, 0.3333333333333333703, 0.3333333333333333703, 0.3333333333333333148, 0.3333333333333334259, 0.3333333333333333703, 0.3333333333333333703, 0.3333333333333333703, 0.3333333333333333703, 0.3333333333333333703, 0.3333333333333333703, 0.3333333333333333703, 0.3333333333333333703, 0.3333333333333333703, 0.3333333333333334259, 0.3333333333333334259, 0.3333333333333333703, 0.3333333333333333703, 0.3333333333333333703, 0.3333333333333333703, 0.3333333333333333703, 0.3333333333333333703, 0.3333333333333333703, 0.3333333333333333148, 0.3333333333333333148, 0.3333333333333333703, 0.3333333333333333703, 0.3333333333333333148, 0.3333333333333334259, 0.3333333333333333703, 0.3333333333333333703, 0.3333333333333333703, 0.3333333333333333703, 0.3333333333333333703, 0.3333333333333333703, 0.3333333333333333703, 0.3333333333333333703, 0.3333333333333333703, 0.3333333333333333703, 0.3333333333333333703, 0.3333333333333333148, 0.3333333333333333703, 0.3333333333333333703, 0.3333333333333333703, 0.3333333333333333703, 0.3333333333333333148, 0.3333333333333333703, 0.3333333333333333703, 0.3333333333333333148, 0.3333333333333333703, 0.3333333333333333703, 0.3333333333333333148, 0.3333333333333334259, 0.3333333333333333703, 0.3333333333333333703, 0.3333333333333333703, 0.3333333333333333703, 0.3333333333333333703, 0.3333333333333334259, 0.3333333333333333703, 0.3333333333333333703, 0.3333333333333334259, 0.3333333333333334259, 0.3333333333333334259, 0.3333333333333333703, 0.3333333333333333703, 0.3333333333333333703, 0.3333333333333333703, 0.3333333333333333703, 0.3333333333333333703, 0.3333333333333333703, 0.3333333333333333703, 0.3333333333333333703, 0.3333333333333334259, 0.3333333333333333703, 0.3333333333333333148, 0.3333333333333334259, 0.3333333333333333703, 0.3333333333333333703, 0.3333333333333333703, 0.3333333333333333703, 0.3333333333333333703, 0.3333333333333334259, 0.3333333333333333703, 0.3333333333333333703, 0.3333333333333333703, 0.3333333333333334259, 0.3333333333333333703, 0.3333333333333333703, 0.3333333333333333703, 0.3333333333333333703, 0.3333333333333333703, 0.3333333333333333703, 0.3333333333333333148, 0.3333333333333334259, 0.3333333333333333703, 0.3333333333333333148, 0.3333333333333333703, 0.3333333333333333703, 0.3333333333333333703, 0.3333333333333334259, 0.3333333333333333703, 0.3333333333333333703, 0.3333333333333333703, 0.3333333333333333703, 0.3333333333333333703, 0.3333333333333334259, 0.3333333333333333703, 0.3333333333333333703, 0.3333333333333333703, 0.3333333333333333703, 0.3333333333333334259, 0.3333333333333333703, 0.3333333333333333703, 0.3333333333333333703, 0.3333333333333333703, 0.3333333333333333703, 0.3333333333333333703, 0.3333333333333333148, 0.3333333333333333703, 0.3333333333333333703, 0.3333333333333333703, 0.3333333333333333703, 0.3333333333333333148, 0.3333333333333333703, 0.3333333333333333703, 0.3333333333333333703, 0.3333333333333333703, 0.3333333333333333703),
 ( 1.000000000000000000, 1.000000000000000000, 1.000000000000000000, 1.000000000000000000, 1.000000000000000000, 1.000000000000000000, 0.9999999999999998890, 0.9999999999999997780, 1.000000000000000000, 1.000000000000000000, 1.000000000000000000, 1.000000000000000000, 1.000000000000000000, 1.000000000000000000, 0.9999999999999998890, 1.000000000000000000, 1.000000000000000222, 1.000000000000000000, 1.000000000000000000, 1.000000000000000000, 1.000000000000000000, 1.000000000000000000, 0.9999999999999998890, 0.9999999999999997780, 1.000000000000000000, 1.000000000000000222, 1.000000000000000000, 1.000000000000000000, 1.000000000000000000, 1.000000000000000000, 0.9999999999999998890, 0.9999999999999997780, 1.000000000000000000, 0.9999999999999998890, 0.9999999999999997780, 1.000000000000000000, 1.000000000000000222, 1.000000000000000222, 1.000000000000000000, 1.000000000000000000, 1.000000000000000222, 1.000000000000000000, 0.9999999999999997780, 1.000000000000000000, 1.000000000000000000, 1.000000000000000000, 1.000000000000000000, 1.000000000000000000, 1.000000000000000000, 1.000000000000000222, 1.000000000000000222, 1.000000000000000000, 1.000000000000000000, 1.000000000000000222, 1.000000000000000222, 1.000000000000000222, 1.000000000000000000, 1.000000000000000000, 1.000000000000000222, 1.000000000000000000, 1.000000000000000000, 1.000000000000000222, 1.000000000000000000, 1.000000000000000000, 1.000000000000000222, 1.000000000000000000, 1.000000000000000000, 0.9999999999999997780, 0.9999999999999998890, 1.000000000000000000, 1.000000000000000000, 1.000000000000000000, 1.000000000000000000, 1.000000000000000222, 1.000000000000000222, 1.000000000000000000, 1.000000000000000000, 1.000000000000000222, 1.000000000000000222, 1.000000000000000222, 1.000000000000000000, 1.000000000000000000, 1.000000000000000222, 1.000000000000000000, 1.000000000000000000, 1.000000000000000222, 1.000000000000000000, 1.000000000000000000, 1.000000000000000222, 1.000000000000000000, 1.000000000000000000, 0.9999999999999997780, 0.9999999999999998890, 1.000000000000000000, 1.000000000000000000, 1.000000000000000000, 1.000000000000000000, 1.000000000000000222, 1.000000000000000222, 1.000000000000000000, 1.000000000000000000, 1.000000000000000222, 1.000000000000000222, 1.000000000000000222, 1.000000000000000000, 1.000000000000000000, 1.000000000000000222, 1.000000000000000000, 0.9999999999999998890, 1.000000000000000222, 1.000000000000000000, 1.000000000000000000, 1.000000000000000222, 1.000000000000000000, 1.000000000000000000, 1.000000000000000222, 1.000000000000000000, 1.000000000000000000, 1.000000000000000000, 1.000000000000000000, 1.000000000000000000, 1.000000000000000222, 1.000000000000000222, 1.000000000000000000, 1.000000000000000000, 1.000000000000000222, 1.000000000000000222, 1.000000000000000222, 1.000000000000000000, 1.000000000000000222, 1.000000000000000222, 1.000000000000000000, 1.000000000000000000, 1.000000000000000222, 1.000000000000000000, 1.000000000000000000, 1.000000000000000222, 1.000000000000000000, 1.000000000000000000, 1.000000000000000222, 1.000000000000000222, 1.000000000000000000, 1.000000000000000000, 1.000000000000000222, 1.000000000000000000, 1.000000000000000222, 1.000000000000000222, 1.000000000000000000, 1.000000000000000000, 1.000000000000000222, 1.000000000000000222, 1.000000000000000222, 1.000000000000000000, 1.000000000000000000, 1.000000000000000222, 1.000000000000000000, 0.9999999999999998890, 1.000000000000000222, 1.000000000000000000, 1.000000000000000000, 1.000000000000000222, 1.000000000000000000, 1.000000000000000000, 1.000000000000000222, 1.000000000000000000, 1.000000000000000000, 1.000000000000000000, 1.000000000000000000, 1.000000000000000000, 1.000000000000000222, 1.000000000000000222, 1.000000000000000000, 1.000000000000000000, 1.000000000000000222, 1.000000000000000222, 1.000000000000000222, 1.000000000000000000, 1.000000000000000000, 1.000000000000000222, 1.000000000000000000, 1.000000000000000000, 1.000000000000000222, 1.000000000000000000, 1.000000000000000000, 1.000000000000000222, 1.000000000000000000, 0.9999999999999996669, 0.9999999999999996669, 1.000000000000000000, 1.000000000000000222, 1.000000000000000000, 1.000000000000000000, 1.000000000000000000, 1.000000000000000000, 1.000000000000000000, 1.000000000000000000, 1.000000000000000000, 1.000000000000000000),
 ( 0.3333333333333333703, 0.3333333333333333703, 0.3333333333333333703, 0.3333333333333334259, 0.3333333333333334259, 0.3333333333333334259, 0.3333333333333333703, 0.3333333333333333148, 0.3333333333333333703, 0.3333333333333333703, 0.3333333333333333148, 0.3333333333333333703, 0.3333333333333333703, 0.3333333333333334814, 0.3333333333333333703, 0.3333333333333333703, 0.3333333333333334259, 0.3333333333333333703, 0.3333333333333333148, 0.3333333333333333703, 0.3333333333333333703, 0.3333333333333333703, 0.3333333333333333703, 0.3333333333333333703, 0.3333333333333333148, 0.3333333333333334259, 0.3333333333333333703, 0.3333333333333333703, 0.3333333333333333703, 0.3333333333333334259, 0.3333333333333333703, 0.3333333333333333703, 0.3333333333333333703, 0.3333333333333333703, 0.3333333333333333148, 0.3333333333333333703, 0.3333333333333334259, 0.3333333333333333703, 0.3333333333333333703, 0.3333333333333333703, 0.3333333333333333703, 0.3333333333333333703, 0.3333333333333333703, 0.3333333333333333703, 0.3333333333333333703, 0.3333333333333333148, 0.3333333333333333703, 0.3333333333333333703, 0.3333333333333333703, 0.3333333333333334259, 0.3333333333333333703, 0.3333333333333333703, 0.3333333333333333703, 0.3333333333333333703, 0.3333333333333333703, 0.3333333333333334259, 0.3333333333333333703, 0.3333333333333333703, 0.3333333333333333703, 0.3333333333333333703, 0.3333333333333334259, 0.3333333333333333703, 0.3333333333333333703, 0.3333333333333333703, 0.3333333333333333703, 0.3333333333333333703, 0.3333333333333333703, 0.3333333333333333148, 0.3333333333333333148, 0.3333333333333333148, 0.3333333333333333703, 0.3333333333333333703, 0.3333333333333333148, 0.3333333333333334259, 0.3333333333333333703, 0.3333333333333333703, 0.3333333333333333703, 0.3333333333333333703, 0.3333333333333333703, 0.3333333333333333703, 0.3333333333333333703, 0.3333333333333333703, 0.3333333333333333703, 0.3333333333333334259, 0.3333333333333334259, 0.3333333333333333703, 0.3333333333333333703, 0.3333333333333333703, 0.3333333333333333703, 0.3333333333333333703, 0.3333333333333333703, 0.3333333333333333703, 0.3333333333333333148, 0.3333333333333333148, 0.3333333333333333703, 0.3333333333333333703, 0.3333333333333333148, 0.3333333333333334259, 0.3333333333333333703, 0.3333333333333333703, 0.3333333333333333703, 0.3333333333333333703, 0.3333333333333333703, 0.3333333333333333703, 0.3333333333333333703, 0.3333333333333333703, 0.3333333333333333703, 0.3333333333333333703, 0.3333333333333333703, 0.3333333333333333148, 0.3333333333333333703, 0.3333333333333333703, 0.3333333333333333703, 0.3333333333333333703, 0.3333333333333333148, 0.3333333333333333703, 0.3333333333333333703, 0.3333333333333333148, 0.3333333333333333703, 0.3333333333333333703, 0.3333333333333333148, 0.3333333333333334259, 0.3333333333333333703, 0.3333333333333333703, 0.3333333333333333703, 0.3333333333333333703, 0.3333333333333333703, 0.3333333333333334259, 0.3333333333333333703, 0.3333333333333333703, 0.3333333333333334259, 0.3333333333333334259, 0.3333333333333334259, 0.3333333333333333703, 0.3333333333333333703, 0.3333333333333333703, 0.3333333333333333703, 0.3333333333333333703, 0.3333333333333333703, 0.3333333333333333703, 0.3333333333333333703, 0.3333333333333333703, 0.3333333333333334259, 0.3333333333333333703, 0.3333333333333333148, 0.3333333333333334259, 0.3333333333333333703, 0.3333333333333333703, 0.3333333333333333703, 0.3333333333333333703, 0.3333333333333333703, 0.3333333333333334259, 0.3333333333333333703, 0.3333333333333333703, 0.3333333333333333703, 0.3333333333333334259, 0.3333333333333333703, 0.3333333333333333703, 0.3333333333333333703, 0.3333333333333333703, 0.3333333333333333703, 0.3333333333333333703, 0.3333333333333333148, 0.3333333333333334259, 0.3333333333333333703, 0.3333333333333333148, 0.3333333333333333703, 0.3333333333333333703, 0.3333333333333333703, 0.3333333333333334259, 0.3333333333333333703, 0.3333333333333333703, 0.3333333333333333703, 0.3333333333333333703, 0.3333333333333333703, 0.3333333333333334259, 0.3333333333333333703, 0.3333333333333333703, 0.3333333333333333703, 0.3333333333333333703, 0.3333333333333334259, 0.3333333333333333703, 0.3333333333333333703, 0.3333333333333333703, 0.3333333333333333703, 0.3333333333333333703, 0.3333333333333333703, 0.3333333333333333148, 0.3333333333333333703, 0.3333333333333333703, 0.3333333333333333703, 0.3333333333333333703, 0.3333333333333333148, 0.3333333333333333703, 0.3333333333333333703, 0.3333333333333333703, 0.3333333333333333703, 0.3333333333333333703),
 ( 0.3333333333333333703, 0.3333333333333333703, 0.3333333333333333703, 0.3333333333333334259, 0.3333333333333334259, 0.3333333333333334259, 0.3333333333333333703, 0.3333333333333333148, 0.3333333333333333703, 0.3333333333333333703, 0.3333333333333333148, 0.3333333333333333703, 0.3333333333333333703, 0.3333333333333334814, 0.3333333333333333703, 0.3333333333333333703, 0.3333333333333334259, 0.3333333333333333703, 0.3333333333333333148, 0.3333333333333333703, 0.3333333333333333703, 0.3333333333333333703, 0.3333333333333333703, 0.3333333333333333703, 0.3333333333333333148, 0.3333333333333334259, 0.3333333333333333703, 0.3333333333333333703, 0.3333333333333333703, 0.3333333333333334259, 0.3333333333333333703, 0.3333333333333333703, 0.3333333333333333703, 0.3333333333333333703, 0.3333333333333333148, 0.3333333333333333703, 0.3333333333333334259, 0.3333333333333333703, 0.3333333333333333703, 0.3333333333333333703, 0.3333333333333333703, 0.3333333333333333703, 0.3333333333333333703, 0.3333333333333333703, 0.3333333333333333703, 0.3333333333333333148, 0.3333333333333333703, 0.3333333333333333703, 0.3333333333333333703, 0.3333333333333334259, 0.3333333333333333703, 0.3333333333333333703, 0.3333333333333333703, 0.3333333333333333703, 0.3333333333333333703, 0.3333333333333334259, 0.3333333333333333703, 0.3333333333333333703, 0.3333333333333333703, 0.3333333333333333703, 0.3333333333333334259, 0.3333333333333333703, 0.3333333333333333703, 0.3333333333333333703, 0.3333333333333333703, 0.3333333333333333703, 0.3333333333333333703, 0.3333333333333333148, 0.3333333333333333148, 0.3333333333333333148, 0.3333333333333333703, 0.3333333333333333703, 0.3333333333333333148, 0.3333333333333334259, 0.3333333333333333703, 0.3333333333333333703, 0.3333333333333333703, 0.3333333333333333703, 0.3333333333333333703, 0.3333333333333333703, 0.3333333333333333703, 0.3333333333333333703, 0.3333333333333333703, 0.3333333333333334259, 0.3333333333333334259, 0.3333333333333333703, 0.3333333333333333703, 0.3333333333333333703, 0.3333333333333333703, 0.3333333333333333703, 0.3333333333333333703, 0.3333333333333333703, 0.3333333333333333148, 0.3333333333333333148, 0.3333333333333333703, 0.3333333333333333703, 0.3333333333333333148, 0.3333333333333334259, 0.3333333333333333703, 0.3333333333333333703, 0.3333333333333333703, 0.3333333333333333703, 0.3333333333333333703, 0.3333333333333333703, 0.3333333333333333703, 0.3333333333333333703, 0.3333333333333333703, 0.3333333333333333703, 0.3333333333333333703, 0.3333333333333333148, 0.3333333333333333703, 0.3333333333333333703, 0.3333333333333333703, 0.3333333333333333703, 0.3333333333333333148, 0.3333333333333333703, 0.3333333333333333703, 0.3333333333333333148, 0.3333333333333333703, 0.3333333333333333703, 0.3333333333333333148, 0.3333333333333334259, 0.3333333333333333703, 0.3333333333333333703, 0.3333333333333333703, 0.3333333333333333703, 0.3333333333333333703, 0.3333333333333334259, 0.3333333333333333703, 0.3333333333333333703, 0.3333333333333334259, 0.3333333333333334259, 0.3333333333333334259, 0.3333333333333333703, 0.3333333333333333703, 0.3333333333333333703, 0.3333333333333333703, 0.3333333333333333703, 0.3333333333333333703, 0.3333333333333333703, 0.3333333333333333703, 0.3333333333333333703, 0.3333333333333334259, 0.3333333333333333703, 0.3333333333333333148, 0.3333333333333334259, 0.3333333333333333703, 0.3333333333333333703, 0.3333333333333333703, 0.3333333333333333703, 0.3333333333333333703, 0.3333333333333334259, 0.3333333333333333703, 0.3333333333333333703, 0.3333333333333333703, 0.3333333333333334259, 0.3333333333333333703, 0.3333333333333333703, 0.3333333333333333703, 0.3333333333333333703, 0.3333333333333333703, 0.3333333333333333703, 0.3333333333333333148, 0.3333333333333334259, 0.3333333333333333703, 0.3333333333333333148, 0.3333333333333333703, 0.3333333333333333703, 0.3333333333333333703, 0.3333333333333334259, 0.3333333333333333703, 0.3333333333333333703, 0.3333333333333333703, 0.3333333333333333703, 0.3333333333333333703, 0.3333333333333334259, 0.3333333333333333703, 0.3333333333333333703, 0.3333333333333333703, 0.3333333333333333703, 0.3333333333333334259, 0.3333333333333333703, 0.3333333333333333703, 0.3333333333333333703, 0.3333333333333333703, 0.3333333333333333703, 0.3333333333333333703, 0.3333333333333333148, 0.3333333333333333703, 0.3333333333333333703, 0.3333333333333333703, 0.3333333333333333703, 0.3333333333333333148, 0.3333333333333333703, 0.3333333333333333703, 0.3333333333333333703, 0.3333333333333333703, 0.3333333333333333703),
 ( 1.000000000000000000, 1.000000000000000000, 1.000000000000000000, 1.000000000000000000, 1.000000000000000000, 1.000000000000000000, 0.9999999999999998890, 0.9999999999999997780, 1.000000000000000000, 1.000000000000000000, 1.000000000000000000, 1.000000000000000000, 1.000000000000000000, 1.000000000000000000, 0.9999999999999998890, 1.000000000000000000, 1.000000000000000222, 1.000000000000000000, 1.000000000000000000, 1.000000000000000000, 1.000000000000000000, 1.000000000000000000, 0.9999999999999998890, 0.9999999999999997780, 1.000000000000000000, 1.000000000000000222, 1.000000000000000000, 1.000000000000000000, 1.000000000000000000, 1.000000000000000000, 0.9999999999999998890, 0.9999999999999997780, 1.000000000000000000, 0.9999999999999998890, 0.9999999999999997780, 1.000000000000000000, 1.000000000000000222, 1.000000000000000222, 1.000000000000000000, 1.000000000000000000, 1.000000000000000222, 1.000000000000000000, 0.9999999999999997780, 1.000000000000000000, 1.000000000000000000, 1.000000000000000000, 1.000000000000000000, 1.000000000000000000, 1.000000000000000000, 1.000000000000000222, 1.000000000000000222, 1.000000000000000000, 1.000000000000000000, 1.000000000000000222, 1.000000000000000222, 1.000000000000000222, 1.000000000000000000, 1.000000000000000000, 1.000000000000000222, 1.000000000000000000, 1.000000000000000000, 1.000000000000000222, 1.000000000000000000, 1.000000000000000000, 1.000000000000000222, 1.000000000000000000, 1.000000000000000000, 0.9999999999999997780, 0.9999999999999998890, 1.000000000000000000, 1.000000000000000000, 1.000000000000000000, 1.000000000000000000, 1.000000000000000222, 1.000000000000000222, 1.000000000000000000, 1.000000000000000000, 1.000000000000000222, 1.000000000000000222, 1.000000000000000222, 1.000000000000000000, 1.000000000000000000, 1.000000000000000222, 1.000000000000000000, 1.000000000000000000, 1.000000000000000222, 1.000000000000000000, 1.000000000000000000, 1.000000000000000222, 1.000000000000000000, 1.000000000000000000, 0.9999999999999997780, 0.9999999999999998890, 1.000000000000000000, 1.000000000000000000, 1.000000000000000000, 1.000000000000000000, 1.000000000000000222, 1.000000000000000222, 1.000000000000000000, 1.000000000000000000, 1.000000000000000222, 1.000000000000000222, 1.000000000000000222, 1.000000000000000000, 1.000000000000000000, 1.000000000000000222, 1.000000000000000000, 0.9999999999999998890, 1.000000000000000222, 1.000000000000000000, 1.000000000000000000, 1.000000000000000222, 1.000000000000000000, 1.000000000000000000, 1.000000000000000222, 1.000000000000000000, 1.000000000000000000, 1.000000000000000000, 1.000000000000000000, 1.000000000000000000, 1.000000000000000222, 1.000000000000000222, 1.000000000000000000, 1.000000000000000000, 1.000000000000000222, 1.000000000000000222, 1.000000000000000222, 1.000000000000000000, 1.000000000000000222, 1.000000000000000222, 1.000000000000000000, 1.000000000000000000, 1.000000000000000222, 1.000000000000000000, 1.000000000000000000, 1.000000000000000222, 1.000000000000000000, 1.000000000000000000, 1.000000000000000222, 1.000000000000000222, 1.000000000000000000, 1.000000000000000000, 1.000000000000000222, 1.000000000000000000, 1.000000000000000222, 1.000000000000000222, 1.000000000000000000, 1.000000000000000000, 1.000000000000000222, 1.000000000000000222, 1.000000000000000222, 1.000000000000000000, 1.000000000000000000, 1.000000000000000222, 1.000000000000000000, 0.9999999999999998890, 1.000000000000000222, 1.000000000000000000, 1.000000000000000000, 1.000000000000000222, 1.000000000000000000, 1.000000000000000000, 1.000000000000000222, 1.000000000000000000, 1.000000000000000000, 1.000000000000000000, 1.000000000000000000, 1.000000000000000000, 1.000000000000000222, 1.000000000000000222, 1.000000000000000000, 1.000000000000000000, 1.000000000000000222, 1.000000000000000222, 1.000000000000000222, 1.000000000000000000, 1.000000000000000000, 1.000000000000000222, 1.000000000000000000, 1.000000000000000000, 1.000000000000000222, 1.000000000000000000, 1.000000000000000000, 1.000000000000000222, 1.000000000000000000, 0.9999999999999996669, 0.9999999999999996669, 1.000000000000000000, 1.000000000000000222, 1.000000000000000000, 1.000000000000000000, 1.000000000000000000, 1.000000000000000000, 1.000000000000000000, 1.000000000000000000, 1.000000000000000000, 1.000000000000000000) ) ) 
 REPRESENTATION_ITEM ( '' )  SURFACE ( )  );
#20692 = CARTESIAN_POINT ( 'NONE',  ( 18.44328704050455769, 144.7751241387205425, -1.717333923880829616 ) ) ;
#20693 = CARTESIAN_POINT ( 'NONE',  ( -6.734570810858633294, 118.9580315507705706, -1.247721039026444378 ) ) ;
#20694 = PLANE ( 'NONE',  #5250 ) ;
#20695 = CARTESIAN_POINT ( 'NONE',  ( 4.265934612124557823, 118.2243144435457936, -0.2925027961061675286 ) ) ;
#20696 = CARTESIAN_POINT ( 'NONE',  ( 13.89276580153818230, 150.2454140652271803, -0.5485491450630708421 ) ) ;
#20697 = EDGE_CURVE ( 'NONE', #35234, #12250, #40073, .T. ) ;
#20698 = ORIENTED_EDGE ( 'NONE', *, *, #40520, .T. ) ;
#20699 = CARTESIAN_POINT ( 'NONE',  ( 3.113553847179573175, -14.91884098843750195, 3.610284256090800170 ) ) ;
#20700 = CARTESIAN_POINT ( 'NONE',  ( -4.828569062062975092, 117.4060461567800786, 1.008118597039231235 ) ) ;
#20701 = CARTESIAN_POINT ( 'NONE',  ( -56.97096143714178140, 2.717004285893040549, 1.832255202882757450 ) ) ;
#20702 = CARTESIAN_POINT ( 'NONE',  ( 3.363087486136625337, 4.875765145370108300, -3.182472177310056605 ) ) ;
#20703 = CARTESIAN_POINT ( 'NONE',  ( 16.93203274801135905, 148.0818255213264365, 2.041866944467892964 ) ) ;
#20704 = CARTESIAN_POINT ( 'NONE',  ( 2.958531772299236362, 39.20946620154573026, 1.329372033065076231 ) ) ;
#20705 = CARTESIAN_POINT ( 'NONE',  ( -6.675377558974173731, 121.2389289720308199, 0.07470202506228494632 ) ) ;
#20706 = EDGE_CURVE ( 'NONE', #24253, #1422, #20971, .T. ) ;
#20707 = CARTESIAN_POINT ( 'NONE',  ( 4.419457123578296454, 17.78516144714274105, -1.360477052881604143 ) ) ;
#20708 = CARTESIAN_POINT ( 'NONE',  ( 8.793090887880877560, 123.6850765633735421, 0.2090564433599598482 ) ) ;
#20709 = CARTESIAN_POINT ( 'NONE',  ( -2.105106575660352419, 106.4592691022973270, 4.917738869260992907 ) ) ;
#20710 = EDGE_CURVE ( 'NONE', #15145, #4252, #22633, .T. ) ;
#20711 = CARTESIAN_POINT ( 'NONE',  ( -51.86985193027732066, 10.34936321858913999, -0.3560079035465085751 ) ) ;
#20712 = CARTESIAN_POINT ( 'NONE',  ( 8.796521542695449725, 117.7070916852149907, 0.01881401154734642714 ) ) ;
#20713 = DIRECTION ( 'NONE',  ( -0.1715592850456333363, -0.1224830539174543431, -0.9775302108976914317 ) ) ;
#20714 = FACE_OUTER_BOUND ( 'NONE', #23115, .T. ) ;
#20715 = CARTESIAN_POINT ( 'NONE',  ( -1.247394927440314882, 105.9869000721035661, 5.191483356333327137 ) ) ;
#20716 = CARTESIAN_POINT ( 'NONE',  ( -3.682264917456324227, 91.53346620154573543, -0.07358041635423968885 ) ) ;
#20717 = CARTESIAN_POINT ( 'NONE',  ( 5.949252453048933909, -3.155934468320678921, 5.972130579448434951 ) ) ;
#20718 = CARTESIAN_POINT ( 'NONE',  ( -6.654617103318593247E-14, 104.6144662015457243, 1.534725424433578570E-31 ) ) ;
#20719 = DIRECTION ( 'NONE',  ( -0.8745520943968243532, 0.4849315768086547296, -5.361993529360573944E-16 ) ) ;
#20720 = CARTESIAN_POINT ( 'NONE',  ( -58.79341205368594814, 0.01963237121659078266, 0.1476394306258261846 ) ) ;
#20721 = CARTESIAN_POINT ( 'NONE',  ( -4.987188648064493357, 117.3993836136597366, -0.9009750914350973527 ) ) ;
#20722 = CARTESIAN_POINT ( 'NONE',  ( -22.92015980622324989, 150.1344166263168347, -0.006220127847215065238 ) ) ;
#20723 = ORIENTED_EDGE ( 'NONE', *, *, #29039, .F. ) ;
#20724 = CARTESIAN_POINT ( 'NONE',  ( -57.40598286442868670, 3.481741809872221260, -1.566274799519931760 ) ) ;
#20725 = CARTESIAN_POINT ( 'NONE',  ( -6.064028428014071714, 121.4341838187324782, -0.1213693123384972511 ) ) ;
#20726 = VERTEX_POINT ( 'NONE', #22843 ) ;
#20727 = CARTESIAN_POINT ( 'NONE',  ( 6.349999999999945466, 86.35999999999998522, 0.000000000000000000 ) ) ;
#20728 = CARTESIAN_POINT ( 'NONE',  ( -9.016099448416641238, 124.0612890738674992, -0.1356653335066258237 ) ) ;
#20729 = CARTESIAN_POINT ( 'NONE',  ( 3.231152580208111580, -15.43077800403741584, 5.551260886339890455 ) ) ;
#20730 = CARTESIAN_POINT ( 'NONE',  ( -11.94841889513460664, 120.7721054874162974, 1.107169436317064770 ) ) ;
#20731 = CARTESIAN_POINT ( 'NONE',  ( 23.12143742665057289, 148.7607265879045144, 1.192451864686425722 ) ) ;
#20732 = CARTESIAN_POINT ( 'NONE',  ( 21.63845757858504726, 150.4657531037631486, -1.001545151475623951 ) ) ;
#20733 = CARTESIAN_POINT ( 'NONE',  ( -4.050807963365556930, 30.95410787014092335, -2.229501126309402448 ) ) ;
#20734 = CARTESIAN_POINT ( 'NONE',  ( -20.67395311655602086, 152.5754960671270055, -0.6363119977773274982 ) ) ;
#20735 = CARTESIAN_POINT ( 'NONE',  ( -51.03866287897986354, 14.58798107696808444, -4.681202568652266471 ) ) ;
#20736 = CARTESIAN_POINT ( 'NONE',  ( 4.973439878603004516, 117.3975399628824903, 0.9753616027188249937 ) ) ;
#20737 = VERTEX_POINT ( 'NONE', #32676 ) ;
#20738 = CARTESIAN_POINT ( 'NONE',  ( -8.775993782722990133, 117.8320326000692830, 0.2360534736673538525 ) ) ;
#20739 = CARTESIAN_POINT ( 'NONE',  ( -5.099922610524069810, 119.9665122172617231, 0.7872683264543848258 ) ) ;
#20740 = CARTESIAN_POINT ( 'NONE',  ( -57.37058287830014791, 1.862367624825627788, -1.511443718440989459 ) ) ;
#20741 = CARTESIAN_POINT ( 'NONE',  ( 12.68516923343323910, 122.7135068550949200, -1.328447112472142644 ) ) ;
#20742 = CARTESIAN_POINT ( 'NONE',  ( -0.4041098725243945644, -13.24273492701920141, -0.8882236940730178221 ) ) ;
#20743 = CARTESIAN_POINT ( 'NONE',  ( -13.72986513748895732, 121.3979351292862816, -1.556522170903472890 ) ) ;
#20744 = CARTESIAN_POINT ( 'NONE',  ( -44.13308345971568514, 24.21351174012166396, -1.567149544246662973 ) ) ;
#20745 = CARTESIAN_POINT ( 'NONE',  ( -8.584014518950164430, 73.13423810798757074, -1.269999999999996687 ) ) ;
#20746 = CARTESIAN_POINT ( 'NONE',  ( 15.38818086081963976, 149.0334586719817764, -0.9521378535654881903 ) ) ;
#20747 = CARTESIAN_POINT ( 'NONE',  ( -2.884051542275779756, 156.0957788938021054, -0.05763021347587621995 ) ) ;
#20748 = CIRCLE ( 'NONE', #16671, 3.683000000000001162 ) ;
#20749 = ORIENTED_EDGE ( 'NONE', *, *, #28749, .T. ) ;
#20750 = CARTESIAN_POINT ( 'NONE',  ( -11.58692091624697973, 123.4149316504530702, -1.682406715187617419 ) ) ;
#20751 = CARTESIAN_POINT ( 'NONE',  ( 4.596189786833723367, -15.64549520875656263, 3.377287787771500849 ) ) ;
#20752 = DIRECTION ( 'NONE',  ( -0.9816537812491126225, -0.1906721105964872265, -8.537024980200846470E-16 ) ) ;
#20753 = CARTESIAN_POINT ( 'NONE',  ( -4.364856043270152419, 118.1847667706781095, -0.6011001361930394804 ) ) ;
#20754 = CARTESIAN_POINT ( 'NONE',  ( -49.59816314059867182, 17.91649583374774224, -5.069000701391666475 ) ) ;
#20755 = DIRECTION ( 'NONE',  ( -0.8745520943968225769, 0.4849315768086578382, -5.691349986800571545E-16 ) ) ;
#20756 = CARTESIAN_POINT ( 'NONE',  ( 17.79834178490394336, 144.5560955566678558, 2.349204209454023307 ) ) ;
#20757 = DIRECTION ( 'NONE',  ( 0.01731298258488073172, -0.9998501190848634312, 1.788962107505278366E-16 ) ) ;
#20758 = CARTESIAN_POINT ( 'NONE',  ( 21.90559427349690935, 151.4293160993575498, 0.4377259060014666026 ) ) ;
#20759 = B_SPLINE_CURVE_WITH_KNOTS ( 'NONE', 3,
 ( #41114, #34310, #5548, #35142 ),
 .UNSPECIFIED., .F., .F.,
 ( 4, 4 ),
 ( 0.000000000000000000, 6.355780391027510178E-05 ),
 .UNSPECIFIED. ) ;
#20760 = CARTESIAN_POINT ( 'NONE',  ( -8.175057852536518510, 12.81247082500981094, 2.033924511151908199 ) ) ;
#20761 = CARTESIAN_POINT ( 'NONE',  ( 11.34253674425776204, 128.2076764602477681, 0.6137764907266788361 ) ) ;
#20762 = CARTESIAN_POINT ( 'NONE',  ( 5.863496024706776666, 117.4684171610355747, -0.5179920176435334200 ) ) ;
#20763 = LINE ( 'NONE', #33788, #17894 ) ;
#20764 = CARTESIAN_POINT ( 'NONE',  ( 1.075792877641968071, 115.6909491485452719, 1.747631130524746279 ) ) ;
#20765 = CARTESIAN_POINT ( 'NONE',  ( -57.68935019796909813, 1.134378438699040759, 1.023808352551137890 ) ) ;
#20766 = CARTESIAN_POINT ( 'NONE',  ( -20.47124607682640729, 129.0748834149669904, -0.3487454591146176841 ) ) ;
#20767 = AXIS2_PLACEMENT_3D ( 'NONE', #14027, #37049, #4263 ) ;
#20768 = ORIENTED_EDGE ( 'NONE', *, *, #28163, .T. ) ;
#20769 = CARTESIAN_POINT ( 'NONE',  ( -46.91604881613258016, 25.30076613767155180, -1.786867259277526543 ) ) ;
#20770 = CARTESIAN_POINT ( 'NONE',  ( 6.898830447510338360, 121.7080221937641369, -0.3537813070057239107 ) ) ;
#20771 = CARTESIAN_POINT ( 'NONE',  ( -46.38316532014823679, 26.05065462784537900, -1.524000000000008459 ) ) ;
#20772 = ORIENTED_EDGE ( 'NONE', *, *, #13097, .F. ) ;
#20773 = CARTESIAN_POINT ( 'NONE',  ( 0.2373273420099217268, 115.6909491485452719, -1.758352294689179196 ) ) ;
#20774 = CARTESIAN_POINT ( 'NONE',  ( -4.329655997251418142, 155.8404949922767742, -0.5159277680907118357 ) ) ;
#20775 = CARTESIAN_POINT ( 'NONE',  ( 4.667506617707346983, -11.86120359225895093, 0.9697133514482669803 ) ) ;
#20776 = CARTESIAN_POINT ( 'NONE',  ( -14.56950268504908941, 121.1548589120785095, 0.7262516135598525713 ) ) ;
#20777 = DIRECTION ( 'NONE',  ( -0.9454731675810331692, 0.3256999990547864154, 8.329459401252003088E-15 ) ) ;
#20778 = CARTESIAN_POINT ( 'NONE',  ( 15.43849248880384906, 120.7004057517279989, 0.4663222373074407678 ) ) ;
#20779 = ORIENTED_EDGE ( 'NONE', *, *, #19063, .F. ) ;
#20780 = CARTESIAN_POINT ( 'NONE',  ( 0.09481320634720795393, -4.229605868409334057, 4.636458411128852930 ) ) ;
#20781 = CARTESIAN_POINT ( 'NONE',  ( -15.95982161465190430, 121.0385544001969436, -0.3359599701671935890 ) ) ;
#20782 = CARTESIAN_POINT ( 'NONE',  ( -41.06677624517580227, 23.07857903943744304, -1.269999999997401652 ) ) ;
#20783 = PLANE ( 'NONE',  #6787 ) ;
#20784 = ORIENTED_EDGE ( 'NONE', *, *, #15180, .F. ) ;
#20785 = CARTESIAN_POINT ( 'NONE',  ( -5.117521106717683566, 119.2591321592902744, 0.9016134253432759316 ) ) ;
#20786 = CARTESIAN_POINT ( 'NONE',  ( -4.070821798575407158, -9.904843093959119216, 2.245307785351264407 ) ) ;
#20787 = CARTESIAN_POINT ( 'NONE',  ( 7.998778050759611347, 118.2752802814886053, 1.041156008592528659 ) ) ;
#20788 = CARTESIAN_POINT ( 'NONE',  ( -58.82782897837071800, -0.2608788304223202958, -0.04583423360434937810 ) ) ;
#20789 = CARTESIAN_POINT ( 'NONE',  ( 0.4390033025490695517, 118.1045761740670201, -0.5613618447453815330 ) ) ;
#20790 = CARTESIAN_POINT ( 'NONE',  ( 3.440871586586784936, -6.993729544307834445, 3.087053954803492761 ) ) ;
#20791 = CARTESIAN_POINT ( 'NONE',  ( -22.50377699857072145, 149.0203452686010337, -1.755643737887156997 ) ) ;
#20792 = EDGE_LOOP ( 'NONE', ( #31818, #11684, #22277, #14636, #173 ) ) ;
#20793 = VERTEX_POINT ( 'NONE', #6905 ) ;
#20794 = CARTESIAN_POINT ( 'NONE',  ( -9.165091971927694203, 123.9989874199980022, 0.04717021870285753593 ) ) ;
#20795 = CARTESIAN_POINT ( 'NONE',  ( 6.089492611447847814, -14.32660765653466584, 1.811095812122764270 ) ) ;
#20796 = LINE ( 'NONE', #33821, #7729 ) ;
#20797 = DIRECTION ( 'NONE',  ( 9.627370216492862708E-17, 1.000000000000000000, -0.000000000000000000 ) ) ;
#20799 = ORIENTED_EDGE ( 'NONE', *, *, #26054, .T. ) ;
#20798 = CIRCLE ( 'NONE', #30331, 0.2540000000000010583 ) ;
#20800 = CARTESIAN_POINT ( 'NONE',  ( 19.16322371038626571, 147.9830121424878939, 2.503561316673066806 ) ) ;
#20801 = DIRECTION ( 'NONE',  ( -1.000000000000000000, 1.011795553208986254E-16, 0.000000000000000000 ) ) ;
#20802 = CARTESIAN_POINT ( 'NONE',  ( -46.87509351769019617, 25.14555728883381391, -1.859034946739896776 ) ) ;
#20803 = CARTESIAN_POINT ( 'NONE',  ( -4.866704567515652613, 117.3073154462328063, 0.4935321157908419409 ) ) ;
#20804 = CARTESIAN_POINT ( 'NONE',  ( 6.390864997528122871, 2.724353428444007630, 5.482255947279437436 ) ) ;
#20805 = CARTESIAN_POINT ( 'NONE',  ( 15.74774640517356517, 148.1776054874778197, 1.420244701258234210 ) ) ;
#20806 = FACE_OUTER_BOUND ( 'NONE', #10482, .T. ) ;
#20807 = CARTESIAN_POINT ( 'NONE',  ( 20.50889283491256876, 152.5656283612522657, -0.2944088047499978655 ) ) ;
#20808 = CYLINDRICAL_SURFACE ( 'NONE', #899, 0.6350000000000001199 ) ;
#20809 = CARTESIAN_POINT ( 'NONE',  ( -57.57924614125985840, 1.413868729064180707, 1.323882363220449054 ) ) ;
#20810 = DIRECTION ( 'NONE',  ( -0.9454731675810336133, 0.3256999990547843615, -5.459396135145337199E-16 ) ) ;
#20811 = CARTESIAN_POINT ( 'NONE',  ( -57.69570286664291103, 2.558035660193719529, 1.875687456014364152 ) ) ;
#20812 = CARTESIAN_POINT ( 'NONE',  ( -58.49135324493490629, -0.001359889153940653820, 0.7038351056170361053 ) ) ;
#20813 = CARTESIAN_POINT ( 'NONE',  ( -4.116168481435051874, 118.2429491485453354, 0.1886889149009219058 ) ) ;
#20814 = CARTESIAN_POINT ( 'NONE',  ( 1.247284263955336758, 105.9875614017104368, -5.191247707446073889 ) ) ;
#20815 = PRODUCT_DEFINITION_SHAPE ( 'NONE', 'NONE',  #42163 ) ;
#20816 = ORIENTED_EDGE ( 'NONE', *, *, #27463, .F. ) ;
#20817 = CARTESIAN_POINT ( 'NONE',  ( -47.20791569504335428, 21.28685671521062517, 4.803936552638831792 ) ) ;
#20818 = CARTESIAN_POINT ( 'NONE',  ( 8.325909852675222211, 120.1128631755567113, -1.118201085292081176 ) ) ;
#20819 = CARTESIAN_POINT ( 'NONE',  ( -5.298772840285949748, 116.6867539651165373, -1.022742042655826022 ) ) ;
#20820 = CARTESIAN_POINT ( 'NONE',  ( 4.381205243309556963, 118.1833089681223470, 0.5842985504508096950 ) ) ;
#20821 = CARTESIAN_POINT ( 'NONE',  ( -6.352854517228420761, 155.4084287100276072, -1.029490774253102536 ) ) ;
#20822 = CARTESIAN_POINT ( 'NONE',  ( -0.4623567408945805646, 115.7034747641299930, -1.762870502475438972 ) ) ;
#20823 = CARTESIAN_POINT ( 'NONE',  ( -3.682264917456322895, 69.94346620154573202, -0.07358041635423923088 ) ) ;
#20824 = CONICAL_SURFACE ( 'NONE', #21482, 12.69999999999999751, 0.7853981633974471688 ) ;
#20825 = ORIENTED_EDGE ( 'NONE', *, *, #23992, .F. ) ;
#20826 = CARTESIAN_POINT ( 'NONE',  ( 4.844936406558457698, 112.7696648386057632, -2.375766922042533036 ) ) ;
#20827 = CARTESIAN_POINT ( 'NONE',  ( 0.01887828017110892292, 156.5412816204240301, -0.9447463363288812754 ) ) ;
#20828 = CARTESIAN_POINT ( 'NONE',  ( -29.81357423954495189, 70.62209452652477637, -1.524000000000007349 ) ) ;
#20829 = CARTESIAN_POINT ( 'NONE',  ( -44.83891394770468963, 21.39113109692259940, 3.507332325251830252 ) ) ;
#20830 = AXIS2_PLACEMENT_3D ( 'NONE', #22693, #25700, #16316 ) ;
#20831 = CARTESIAN_POINT ( 'NONE',  ( -41.05190940396061450, 23.09449711908037983, 1.270000000023963960 ) ) ;
#20832 = CARTESIAN_POINT ( 'NONE',  ( -15.26787271661999235, 148.0267594272436895, -0.1054338715682280742 ) ) ;
#20833 = CARTESIAN_POINT ( 'NONE',  ( 4.850929972935443146, 117.7610086971114356, 0.9074237114610381738 ) ) ;
#20834 = CARTESIAN_POINT ( 'NONE',  ( 20.30524341716966319, 152.5255278361454145, 1.346157490925044664 ) ) ;
#20835 = CARTESIAN_POINT ( 'NONE',  ( 5.177913976931209916, 65.30181249999998272, -5.372099999999993436 ) ) ;
#20837 = CARTESIAN_POINT ( 'NONE',  ( 21.17434475962598484, 141.7209635633906259, -1.395834004474946655 ) ) ;
#20836 = CARTESIAN_POINT ( 'NONE',  ( 3.411949332026259274, -14.94726182254324520, 2.206293558762954188 ) ) ;
#20838 = CARTESIAN_POINT ( 'NONE',  ( -11.50356673920490991, 154.6851215890897038, 1.708948620147628938 ) ) ;
#20839 = CARTESIAN_POINT ( 'NONE',  ( -0.9685753864191435358, -11.31243604255521085, 0.1179740209226832204 ) ) ;
#20840 = CARTESIAN_POINT ( 'NONE',  ( -11.45183593531622535, 118.8698716516685465, -0.7694570404682199438 ) ) ;
#20841 = CARTESIAN_POINT ( 'NONE',  ( 0.3309596775784566236, 20.21946177965197222, 0.9160044982600296093 ) ) ;
#20842 = ORIENTED_EDGE ( 'NONE', *, *, #40560, .F. ) ;
#20843 = CARTESIAN_POINT ( 'NONE',  ( -48.39470387610976587, 16.07729130905085313, 1.622931888101216691 ) ) ;
#20844 = CONTEXT_DEPENDENT_SHAPE_REPRESENTATION ( #14260, #20815 ) ;
#20845 = CARTESIAN_POINT ( 'NONE',  ( -12.13795026801536814, 151.9817061558079274, 0.5567646394148116906 ) ) ;
#20846 = CARTESIAN_POINT ( 'NONE',  ( 4.964329757808820354, -12.46733462535230785, 1.954119038396571417 ) ) ;
#20847 = CARTESIAN_POINT ( 'NONE',  ( 17.00008652715106194, 148.0818255213264365, -1.363822447394348991 ) ) ;
#20848 = ORIENTED_EDGE ( 'NONE', *, *, #38908, .F. ) ;
#20849 = CARTESIAN_POINT ( 'NONE',  ( 3.612019075414997893, 115.7029516305954360, 1.621388860772168039 ) ) ;
#20850 = CARTESIAN_POINT ( 'NONE',  ( 2.739926266261139887, -12.91893237176182296, 0.2921503600690461555 ) ) ;
#20851 = CARTESIAN_POINT ( 'NONE',  ( -4.806730152592563421, 117.4761099757325269, -1.179797647331112698 ) ) ;
#20852 = CARTESIAN_POINT ( 'NONE',  ( 7.800806202324914729, 154.6345575486818404, 0.04849676858278741121 ) ) ;
#20853 = ORIENTED_EDGE ( 'NONE', *, *, #9662, .F. ) ;
#20854 = CARTESIAN_POINT ( 'NONE',  ( 8.895965109948861027, 157.0267672960688969, 2.032209471265452816 ) ) ;
#20855 = CARTESIAN_POINT ( 'NONE',  ( 3.155936729621069858, 108.2677041351691543, 4.292818659978050455 ) ) ;
#20856 = AXIS2_PLACEMENT_3D ( 'NONE', #38062, #37423, #14621 ) ;
#20857 = CARTESIAN_POINT ( 'NONE',  ( -2.958531772299361595, 50.13146620154573441, -1.329372033065077119 ) ) ;
#20858 = EDGE_CURVE ( 'NONE', #36274, #26682, #9437, .T. ) ;
#20859 = DIRECTION ( 'NONE',  ( 3.035386659626960118E-16, -0.000000000000000000, 1.000000000000000000 ) ) ;
#20860 = AXIS2_PLACEMENT_3D ( 'NONE', #13712, #19879, #32893 ) ;
#20861 = CARTESIAN_POINT ( 'NONE',  ( 15.44479738614495901, 120.7004057517279989, 0.1507993925391201140 ) ) ;
#20862 = DIRECTION ( 'NONE',  ( 9.627370216492862708E-17, 1.000000000000000000, -0.000000000000000000 ) ) ;
#20863 = CARTESIAN_POINT ( 'NONE',  ( 1.931211713635406113, -15.24862219501368976, 5.987091862552307298 ) ) ;
#20864 = FACE_OUTER_BOUND ( 'NONE', #24458, .T. ) ;
#20865 = CARTESIAN_POINT ( 'NONE',  ( 1.957912617769093755, 35.96399040732271857, -0.5992445403938203574 ) ) ;
#20866 = EDGE_CURVE ( 'NONE', #4252, #31622, #31879, .T. ) ;
#20867 = CARTESIAN_POINT ( 'NONE',  ( 4.699679879530964222, 158.1906701298835856, 1.765476639684188109 ) ) ;
#20868 = EDGE_LOOP ( 'NONE', ( #41826, #2216, #41441, #27180 ) ) ;
#20869 = CARTESIAN_POINT ( 'NONE',  ( 8.424193198035354158, 17.36166136180145259, -0.6763034115371487909 ) ) ;
#20870 = CARTESIAN_POINT ( 'NONE',  ( -5.483011483344768955, 117.5783348333330594, -0.9732951423285314263 ) ) ;
#20871 = CARTESIAN_POINT ( 'NONE',  ( -3.014030426305907895, 115.9530684888725460, -1.587286815012125984 ) ) ;
#20872 = FACE_OUTER_BOUND ( 'NONE', #22102, .T. ) ;
#20873 = DIRECTION ( 'NONE',  ( -0.8745520943968220218, 0.4849315768086588374, -4.268512490100437040E-16 ) ) ;
#20874 = CARTESIAN_POINT ( 'NONE',  ( -6.374728672999452917E-14, 124.9344662015457317, 7.707042028354222152E-17 ) ) ;
#20875 = CIRCLE ( 'NONE', #13443, 0.2540000000000022795 ) ;
#20876 = CARTESIAN_POINT ( 'NONE',  ( -3.640175008984333882, 11.51306413504884318, -2.862805987297033727 ) ) ;
#20877 = PLANE ( 'NONE',  #23057 ) ;
#20878 = CARTESIAN_POINT ( 'NONE',  ( -4.772317898405468384, 118.5264896598256854, 0.8398864596484367784 ) ) ;
#20879 = CARTESIAN_POINT ( 'NONE',  ( 3.771727509258866906, -13.52648377956064429, 3.452274064300702605 ) ) ;
#20880 = CARTESIAN_POINT ( 'NONE',  ( 3.226952561781350592, 118.4615047536228047, -0.6622324852003673712 ) ) ;
#20881 = PRODUCT_DEFINITION ( 'UNKNOWN', '', #18925, #13765 ) ;
#20882 = CARTESIAN_POINT ( 'NONE',  ( -1.879194370357706756, 31.42354579518680424, 3.981814511614891305 ) ) ;
#20883 = DIRECTION ( 'NONE',  ( -0.9454731675810330582, 0.3256999990547864710, -3.976957304636361482E-16 ) ) ;
#20884 = AXIS2_PLACEMENT_3D ( 'NONE', #3984, #33573, #17565 ) ;
#20885 = ORIENTED_EDGE ( 'NONE', *, *, #25293, .T. ) ;
#20886 = CARTESIAN_POINT ( 'NONE',  ( -4.754641576874411690, 104.6144662015456959, -0.8423218056084632588 ) ) ;
#20887 = CARTESIAN_POINT ( 'NONE',  ( 4.918985584458519966, -15.36470173770705649, 0.08744857223284302483 ) ) ;
#20888 = CARTESIAN_POINT ( 'NONE',  ( -0.01147819631912393862, 118.5605975114896609, 0.5744158801423954186 ) ) ;
#20889 = CARTESIAN_POINT ( 'NONE',  ( -0.9542339719106045504, 13.68595756868040603, 0.2091889690632084686 ) ) ;
#20890 = EDGE_CURVE ( 'NONE', #26382, #5685, #33257, .T. ) ;
#20891 = ORIENTED_EDGE ( 'NONE', *, *, #691, .T. ) ;
#20892 = EDGE_LOOP ( 'NONE', ( #19483, #841, #24568, #26076, #40984 ) ) ;
#20893 = FACE_OUTER_BOUND ( 'NONE', #35697, .T. ) ;
#20894 = AXIS2_PLACEMENT_3D ( 'NONE', #2843, #3053, #9632 ) ;
#20895 = CARTESIAN_POINT ( 'NONE',  ( 4.585195778441632619, 124.9344662015457459, 0.09162312381275027062 ) ) ;
#20896 = CARTESIAN_POINT ( 'NONE',  ( -0.006810764310395450195, 120.3493709785083183, 0.3408384964863782063 ) ) ;
#20897 = CARTESIAN_POINT ( 'NONE',  ( -5.348924234571056147, 56.51499999999999346, 4.492130288940740179 ) ) ;
#20898 = EDGE_CURVE ( 'NONE', #35171, #32704, #29839, .T. ) ;
#20899 = CARTESIAN_POINT ( 'NONE',  ( 4.692195371935813597, 117.9823393671588434, -0.6749937859069751189 ) ) ;
#20900 = CARTESIAN_POINT ( 'NONE',  ( 11.57150582532048411, 123.3156264706956478, -1.212837404772455052 ) ) ;
#20901 = CARTESIAN_POINT ( 'NONE',  ( -20.10299018766040291, 141.3454246894093274, -2.438971827487009136 ) ) ;
#20902 = DIRECTION ( 'NONE',  ( -0.8745520943968245753, 0.4849315768086539524, -5.691349986800526185E-16 ) ) ;
#20903 = EDGE_CURVE ( 'NONE', #11738, #32240, #6053, .T. ) ;
#20904 = ORIENTED_EDGE ( 'NONE', *, *, #28211, .T. ) ;
#20905 = CARTESIAN_POINT ( 'NONE',  ( 4.250116660506480848, 118.2249359311486643, -0.3102634091937140348 ) ) ;
#20906 = CARTESIAN_POINT ( 'NONE',  ( 3.676778326629012827, 120.9289264519876070, -0.1742216996082329161 ) ) ;
#20907 = ORIENTED_EDGE ( 'NONE', *, *, #38026, .F. ) ;
#20908 = CARTESIAN_POINT ( 'NONE',  ( 2.670684053127368784, -15.04618456763519241, 4.548342027319769443 ) ) ;
#20909 = FACE_OUTER_BOUND ( 'NONE', #11610, .T. ) ;
#20910 = AXIS2_PLACEMENT_3D ( 'NONE', #26567, #36587, #23349 ) ;
#20911 = CARTESIAN_POINT ( 'NONE',  ( -58.44182880578495087, -0.4131463110825606133, 0.3217794782789726860 ) ) ;
#20912 = CARTESIAN_POINT ( 'NONE',  ( -3.074427775304182209, -11.96646105551300643, -3.469969274305642060 ) ) ;
#20913 = CARTESIAN_POINT ( 'NONE',  ( 2.572680461994239831, 120.1437993944865354, 0.5932419562244882760 ) ) ;
#20914 = CARTESIAN_POINT ( 'NONE',  ( -3.521407940696402505, 28.96769372650263819, 2.403306918834325678 ) ) ;
#20915 = CARTESIAN_POINT ( 'NONE',  ( -5.259129974998975499, 118.7524313932052991, 0.4270625282899582764 ) ) ;
#20916 = CARTESIAN_POINT ( 'NONE',  ( 2.551540157903699146, -0.3564265548712530207, -3.854280124997286450 ) ) ;
#20917 = CARTESIAN_POINT ( 'NONE',  ( 7.796516423212079161, 154.6345575486818404, 0.2631748570402916432 ) ) ;
#20918 = CARTESIAN_POINT ( 'NONE',  ( -11.42297701379735564, 55.88459609804033335, 4.463034230327252772 ) ) ;
#20919 = CARTESIAN_POINT ( 'NONE',  ( -57.76865908382304582, 0.8624112519253351872, -0.3783812474403069337 ) ) ;
#20920 = CARTESIAN_POINT ( 'NONE',  ( 8.795815767003183794, 117.7122569620870962, 0.001127142753954061974 ) ) ;
#20921 = DIRECTION ( 'NONE',  ( -0.8745520943968235761, 0.4849315768086558398, -4.268512490100410909E-16 ) ) ;
#20922 = CARTESIAN_POINT ( 'NONE',  ( -46.95911617132933458, 24.98948415085536823, -1.986615011824472088 ) ) ;
#20923 = CARTESIAN_POINT ( 'NONE',  ( -0.1064799869811723365, 105.7853621660184444, 5.332934571178563843 ) ) ;
#20924 = LINE ( 'NONE', #4778, #27022 ) ;
#20925 = CARTESIAN_POINT ( 'NONE',  ( 8.109546976224176973, 7.201272144248561879, 2.403482862635152539 ) ) ;
#20926 = DIRECTION ( 'NONE',  ( -0.8745520943968243532, 0.4849315768086547296, -5.361993529360573944E-16 ) ) ;
#20927 = PLANE ( 'NONE',  #31397 ) ;
#20928 = CARTESIAN_POINT ( 'NONE',  ( -57.89852354142710311, 2.261894840748110536, 1.235920526244124851 ) ) ;
#20929 = CARTESIAN_POINT ( 'NONE',  ( 0.0006472084742222537247, 124.6436471961814476, -0.03238895860161178364 ) ) ;
#20930 = CARTESIAN_POINT ( 'NONE',  ( -23.16228472148477380, 149.2833505036244048, 0.1324855245534191928 ) ) ;
#20931 = ORIENTED_EDGE ( 'NONE', *, *, #30286, .T. ) ;
#20932 = CARTESIAN_POINT ( 'NONE',  ( -56.17386367503594613, 7.314326147911789811, -0.9214986423944944161 ) ) ;
#20933 = ADVANCED_FACE ( 'NONE', ( #7746 ), #16907, .T. ) ;
#20934 = ORIENTED_EDGE ( 'NONE', *, *, #17108, .T. ) ;
#20935 = FACE_OUTER_BOUND ( 'NONE', #2124, .T. ) ;
#20936 = CARTESIAN_POINT ( 'NONE',  ( -2.836071964827412639, 121.0300505300837415, -0.05667146733340956699 ) ) ;
#20937 = CARTESIAN_POINT ( 'NONE',  ( 4.377062889037126148, -14.98224217357194199, 4.840108967533193862 ) ) ;
#20938 = CARTESIAN_POINT ( 'NONE',  ( -12.83522892222240053, 121.3369795956499928, 1.134461614517290551 ) ) ;
#20939 =( GEOMETRIC_REPRESENTATION_CONTEXT ( 3 ) GLOBAL_UNCERTAINTY_ASSIGNED_CONTEXT ( ( #26548 ) ) GLOBAL_UNIT_ASSIGNED_CONTEXT ( ( #7512, #1549, #17079 ) ) REPRESENTATION_CONTEXT ( 'NONE', 'WORKASPACE' ) );
#20940 = CARTESIAN_POINT ( 'NONE',  ( 14.56950268504896151, 121.1548589120785095, -0.7262516135598524603 ) ) ;
#20941 = CARTESIAN_POINT ( 'NONE',  ( -33.00685850039228342, 50.69800224577189596, 1.270000000006296537 ) ) ;
#20942 = CARTESIAN_POINT ( 'NONE',  ( -13.56676737375339137, 119.6371495169912436, -0.4909217195147885238 ) ) ;
#20943 = CARTESIAN_POINT ( 'NONE',  ( -50.91190571670057352, 14.80147821656241369, -4.713324810010480981 ) ) ;
#20944 = ORIENTED_EDGE ( 'NONE', *, *, #14881, .F. ) ;
#20945 = CARTESIAN_POINT ( 'NONE',  ( 6.059261036834406866, 56.51500000000000057, 4.547742611252461487 ) ) ;
#20946 = CARTESIAN_POINT ( 'NONE',  ( -6.603469437764838190, 120.5225452898634728, 0.8609044167644233081 ) ) ;
#20947 = CARTESIAN_POINT ( 'NONE',  ( -48.87447604115916988, 17.97958907615011981, -5.093074433551099567 ) ) ;
#20948 = ADVANCED_FACE ( 'NONE', ( #20495 ), #41430, .T. ) ;
#20949 = CARTESIAN_POINT ( 'NONE',  ( 18.66004122726566195, 149.2887123452801745, -1.736808470001686810 ) ) ;
#20950 = CARTESIAN_POINT ( 'NONE',  ( -14.23594795111950084, 121.8555783441548073, -1.592150851459066319 ) ) ;
#20951 = CARTESIAN_POINT ( 'NONE',  ( -48.98489377192316852, 18.65252824715059177, -5.272350768541925525 ) ) ;
#20952 = VECTOR ( 'NONE', #16565, 1000.000000000000000 ) ;
#20953 = EDGE_CURVE ( 'NONE', #20294, #1007, #23912, .T. ) ;
#20954 = CARTESIAN_POINT ( 'NONE',  ( 2.657114488131237628, 120.4390018212493914, -0.3871174720959879578 ) ) ;
#20955 = CARTESIAN_POINT ( 'NONE',  ( 7.788927721206574617, 122.5994874646387984, 0.3062633923827431381 ) ) ;
#20956 = ORIENTED_EDGE ( 'NONE', *, *, #8411, .T. ) ;
#20957 = CARTESIAN_POINT ( 'NONE',  ( -11.70444740893367275, 123.2143981803894093, -1.719255905491489544 ) ) ;
#20958 = CARTESIAN_POINT ( 'NONE',  ( 4.348370292662268710, -15.56902811939260545, 2.317716755344581880 ) ) ;
#20959 = ADVANCED_FACE ( 'NONE', ( #33944 ), #1989, .T. ) ;
#20960 = DIRECTION ( 'NONE',  ( -4.017660918040594346E-17, 1.000000000000000000, 2.376309959284832031E-19 ) ) ;
#20961 = CARTESIAN_POINT ( 'NONE',  ( -4.266443719422126968, 118.2131497807364724, -0.5314359833645941888 ) ) ;
#20962 = CARTESIAN_POINT ( 'NONE',  ( -55.65298819915649631, 5.540485941798511504, -2.823722248809264368 ) ) ;
#20963 = CARTESIAN_POINT ( 'NONE',  ( -4.975714317725813629, 117.5352226273689240, 0.7922778689861946777 ) ) ;
#20964 = CARTESIAN_POINT ( 'NONE',  ( 16.10024230344501461, 135.1141785778430346, 2.240991319914668711 ) ) ;
#20965 = CARTESIAN_POINT ( 'NONE',  ( -23.75665686005077504, 76.91945007112674659, -1.270000000000005125 ) ) ;
#20966 = CARTESIAN_POINT ( 'NONE',  ( 18.81756541077860589, 125.3161215262879580, 0.3201835051929645126 ) ) ;
#20967 = B_SPLINE_CURVE_WITH_KNOTS ( 'NONE', 3,
 ( #39095, #6717, #19686, #32917, #16920, #29920, #32702, #17960, #24775, #8388, #18373, #21352, #27351, #14341, #36952, #5002, #11159, #40983, #27562, #37359, #24144, #27973, #33968, #40569, #8178, #40775, #34174, #37152, #17544, #4796, #27764, #2009, #1597, #7772, #40154, #5418, #5210, #40364, #7975, #37773, #14972, #31168, #1383, #31381, #14763, #23935, #18165, #17747, #21145, #20943, #30960, #11785, #11367, #24558, #20735, #1800, #8598, #21561, #34589, #30747, #11572, #33759, #37562, #2224, #27141, #34377, #10946, #4585, #30545, #14554, #24354, #2851, #12628, #25616, #22607, #2644, #21988, #18796, #15397, #38420, #29017, #5842, #9232, #2436, #19008, #16018, #15604, #38627, #8814, #22191, #3061, #12833, #42037, #41407, #35221, #28609, #37990, #32012, #35639, #19219, #6046, #21773, #12214, #28402, #25204, #41618, #22399, #6250, #38208, #41192, #34799, #19427, #32230, #15812, #31807, #28819, #25821, #35021, #9025, #5632, #6454, #38829, #18590, #35423, #9639, #12427, #25419, #41834, #24990, #9430, #32433, #15184, #28188, #11996, #31599, #39251, #19629, #39679, #6874, #23451, #26031, #16224, #32644, #7094, #36478, #13679, #73, #6666, #7298, #4115, #708, #26242, #23239, #33285, #285, #36273, #10058, #17075, #13258, #10481, #19846, #13041, #3480, #36059, #16440, #39040, #499, #20258, #20055, #3264, #16868, #29446, #23029, #9847, #26460, #32860, #29231, #13472, #10266, #3691, #39464, #16652, #33074 ),
 .UNSPECIFIED., .F., .F.,
 ( 4, 2, 2, 2, 1, 1, 2, 2, 2, 2, 1, 1, 1, 1, 1, 2, 2, 2, 2, 1, 1, 1, 1, 2, 2, 2, 1, 2, 2, 2, 1, 1, 1, 1, 2, 2, 2, 1, 1, 1, 1, 2, 2, 2, 2, 1, 1, 1, 1, 1, 2, 2, 2, 2, 2, 2, 1, 1, 1, 2, 2, 2, 2, 2, 1, 2, 1, 2, 2, 2, 2, 2, 2, 2, 1, 2, 2, 2, 2, 2, 2, 2, 1, 1, 2, 2, 2, 2, 2, 2, 1, 1, 2, 2, 2, 2, 2, 2, 2, 2, 2, 2, 2, 2, 2, 2, 2, 2, 4 ),
 ( 0.000000000000000000, 0.03125000000131424038, 0.04687500000197108996, 0.05468750000229992414, 0.05859375000246411225, 0.06054687500254619936, 0.06152343750258739558, 0.06250000000262859179, 0.09375000000393932109, 0.1093750000045946719, 0.1171875000049223542, 0.1210937500050864452, 0.1230468750051682963, 0.1240234375052087917, 0.1245117187552288313, 0.1247558593802386151, 0.1250000000052483851, 0.1406250000051884608, 0.1484375000051583182, 0.1523437500051430804, 0.1542968750051351978, 0.1552734375051311733, 0.1557617187551290361, 0.1560058593801280924, 0.1562500000051271210, 0.1718750000050420779, 0.1796875000049995841, 0.1835937500049780735, 0.1875000000049565629, 0.2187500000047861992, 0.2343750000047007953, 0.2421875000046579685, 0.2460937500046365689, 0.2480468750046257720, 0.2490234375046203597, 0.2500000000046149751, 0.3125000000042688630, 0.3437500000040961678, 0.3593750000040099035, 0.3671875000039666603, 0.3710937500039451775, 0.3730468750039344084, 0.3750000000039236947, 0.4375000000035705328, 0.4687500000033941183, 0.4843750000033057446, 0.4921875000032616687, 0.4960937500032398528, 0.4980468750032286951, 0.4990234375032232550, 0.4995117187532203684, 0.5000000000032174263, 0.6250000000024309443, 0.6875000000020378144, 0.7187500000018411939, 0.7343750000017429391, 0.7421875000016938673, 0.7460937500016691093, 0.7480468750016567858, 0.7490234375016504575, 0.7500000000016441293, 0.8125000000012420065, 0.8437500000010410561, 0.8593750000009408030, 0.8671875000008907319, 0.8710937500008657519, 0.8730468750008532064, 0.8740234375008467671, 0.8750000000008402168, 0.9062500000006236123, 0.9218750000005151435, 0.9296875000004609646, 0.9335937500004340972, 0.9355468750004206635, 0.9365234375004140022, 0.9370117187504105605, 0.9375000000004071188, 0.9531250000003018696, 0.9609375000002491340, 0.9648437500002227107, 0.9687500000001961764, 0.9726562500001697531, 0.9746093750001566525, 0.9755859375001501022, 0.9760742187501468825, 0.9765625000001436629, 0.9804687500001181277, 0.9824218750001054712, 0.9843750000000928146, 0.9863281250000801581, 0.9873046875000739409, 0.9877929687500708322, 0.9880371093750691669, 0.9882812500000676126, 0.9892578125000615064, 0.9897460937500585088, 0.9902343750000555112, 0.9907226562500525135, 0.9912109375000495159, 0.9914550781250479616, 0.9916992187500465183, 0.9919433593750449640, 0.9921875000000435207, 0.9941406250000325295, 0.9951171875000270894, 0.9960937500000216493, 0.9970703125000162093, 0.9980468750000107692, 1.000000000000000000 ),
 .UNSPECIFIED. ) ;
#20968 = CARTESIAN_POINT ( 'NONE',  ( 6.048790893839320226, 16.06121166075865148, 5.875566521300903844 ) ) ;
#20969 = CARTESIAN_POINT ( 'NONE',  ( 14.79492108907963477, 148.8567844064068026, 0.8802232212986721427 ) ) ;
#20970 = CARTESIAN_POINT ( 'NONE',  ( -4.085839532347240066, 71.06758511999679229, -1.269999999999994023 ) ) ;
#20971 = CIRCLE ( 'NONE', #26429, 6.350000000000004974 ) ;
#20972 = CARTESIAN_POINT ( 'NONE',  ( 5.241362157049057835, 57.14999999999998437, 5.310945289804168468 ) ) ;
#20973 = CIRCLE ( 'NONE', #31880, 0.5080000000000002292 ) ;
#20974 = DIRECTION ( 'NONE',  ( -6.353134868986659519E-16, 1.000000000000000000, 0.000000000000000000 ) ) ;
#20975 = CARTESIAN_POINT ( 'NONE',  ( -58.02159823468433331, 0.4660483771539991604, 0.8824573672536664137 ) ) ;
#20976 = CARTESIAN_POINT ( 'NONE',  ( -9.807059279560077059, 117.9968303279965340, -0.1034500883390724879 ) ) ;
#20977 = VERTEX_POINT ( 'NONE', #40548 ) ;
#20978 = CARTESIAN_POINT ( 'NONE',  ( -47.59483747600737047, 24.73124547893296921, -0.7500189231788918498 ) ) ;
#20979 = CARTESIAN_POINT ( 'NONE',  ( 7.917148831097427397, 122.0549026337326808, -0.5915961107884312176 ) ) ;
#20980 = FACE_BOUND ( 'NONE', #26313, .T. ) ;
#20981 = ORIENTED_EDGE ( 'NONE', *, *, #17060, .F. ) ;
#20982 = CARTESIAN_POINT ( 'NONE',  ( 0.5726544197577119188, 115.7031858585135637, -1.740669147351574075 ) ) ;
#20983 = CARTESIAN_POINT ( 'NONE',  ( -15.75631923737921092, 146.9135488020124001, -0.6449975968329648701 ) ) ;
#20984 = CARTESIAN_POINT ( 'NONE',  ( 4.871446434089309108, -12.86987818651588711, 2.618604111146097591 ) ) ;
#20985 = CARTESIAN_POINT ( 'NONE',  ( -7.412489149516535036, 158.3992165788449711, 1.135539963648920070 ) ) ;
#20986 = CARTESIAN_POINT ( 'NONE',  ( 1.627035472719924547, 117.3993836203816556, -1.397827203978000865 ) ) ;
#20987 = CARTESIAN_POINT ( 'NONE',  ( 2.764936593379123675, 116.5678055239024644, 0.1631480333911173308 ) ) ;
#20988 = CARTESIAN_POINT ( 'NONE',  ( 8.739549413732950356, 123.6764625261342587, 0.2181624419688201200 ) ) ;
#20989 = EDGE_LOOP ( 'NONE', ( #19539, #801, #38778, #18494 ) ) ;
#20990 = CARTESIAN_POINT ( 'NONE',  ( 0.2723526006440308844, 25.78125159710042169, 0.9401034630801221592 ) ) ;
#20991 = CARTESIAN_POINT ( 'NONE',  ( -23.11076619426189538, 149.9001102426712748, -0.4874744954944869590 ) ) ;
#20992 = CARTESIAN_POINT ( 'NONE',  ( -43.26072192867658117, 21.85338993931741669, -2.263361967372762074 ) ) ;
#20993 = ORIENTED_EDGE ( 'NONE', *, *, #34710, .F. ) ;
#20994 = LINE ( 'NONE', #40206, #27195 ) ;
#20995 = EDGE_LOOP ( 'NONE', ( #25128, #14404 ) ) ;
#20996 = CARTESIAN_POINT ( 'NONE',  ( -8.335421588164685147, 120.0665240995501364, 1.118669443656532758 ) ) ;
#20997 = CARTESIAN_POINT ( 'NONE',  ( 4.571311019248293306, -6.119132638730012452, 0.7325351754658009362 ) ) ;
#20998 = CARTESIAN_POINT ( 'NONE',  ( 13.94627971010872614, 121.2764344996515717, 1.482775695869144705 ) ) ;
#20999 = CARTESIAN_POINT ( 'NONE',  ( -57.40739589891802552, 2.334961046654995709, -1.895125133214725199 ) ) ;
#21000 = CARTESIAN_POINT ( 'NONE',  ( 1.145842520592908365, 158.4310823543925721, -1.558676969884219332 ) ) ;
#21001 = CARTESIAN_POINT ( 'NONE',  ( 2.990331240142678482, -7.206181497205274233, 3.547999066060627094 ) ) ;
#21002 = CARTESIAN_POINT ( 'NONE',  ( -6.860783072103511238, 117.8105958006179890, -0.8866969874100999460 ) ) ;
#21003 = CARTESIAN_POINT ( 'NONE',  ( 4.975302499479774987, 117.5352015494678142, -0.7925089078733521530 ) ) ;
#21004 = EDGE_CURVE ( 'NONE', #24227, #36646, #26466, .T. ) ;
#21005 = VERTEX_POINT ( 'NONE', #24122 ) ;
#21006 = CARTESIAN_POINT ( 'NONE',  ( -9.747124062405315925, 124.8671652961716489, 0.04776528062357104226 ) ) ;
#21007 = EDGE_CURVE ( 'NONE', #2275, #4943, #14951, .T. ) ;
#21008 = CARTESIAN_POINT ( 'NONE',  ( 2.113928706699719218, -15.46215275738946282, 5.949113654003534535 ) ) ;
#21009 = CARTESIAN_POINT ( 'NONE',  ( 13.85159022459153988, 16.51000000000000156, -5.016499999999999737 ) ) ;
#21010 = DIRECTION ( 'NONE',  ( 0.9998004120163608288, 0.000000000000000000, 0.01997839162482749342 ) ) ;
#21011 = VERTEX_POINT ( 'NONE', #8365 ) ;
#21012 = CARTESIAN_POINT ( 'NONE',  ( 4.155191945500637196, 119.0775769483117870, 1.003333751211267888 ) ) ;
#21013 = DIRECTION ( 'NONE',  ( -0.8745520943968247973, 0.4849315768086537304, -5.361993529360573944E-16 ) ) ;
#21014 = CARTESIAN_POINT ( 'NONE',  ( -33.42971872652992005, 49.93539301574497102, -1.270000000000005569 ) ) ;
#21015 = CARTESIAN_POINT ( 'NONE',  ( -3.898136962790746285, 117.1932757116604762, 0.4670938640342006676 ) ) ;
#21016 = CARTESIAN_POINT ( 'NONE',  ( 6.464508713081113633, 4.871470569706378484, -5.424950676754816570 ) ) ;
#21017 = CARTESIAN_POINT ( 'NONE',  ( 13.80305775881199537, 134.3516747369166069, 1.357216474725372768 ) ) ;
#21018 = CARTESIAN_POINT ( 'NONE',  ( 6.059261036834405978, 56.51500000000000057, 4.381499999999999950 ) ) ;
#21019 = CARTESIAN_POINT ( 'NONE',  ( 10.65151157945274996, 157.9324367681937815, -0.3596066298475817935 ) ) ;
#21020 = DIRECTION ( 'NONE',  ( 4.017660918040594346E-17, -1.000000000000000000, -2.376309959284834438E-19 ) ) ;
#21021 = CARTESIAN_POINT ( 'NONE',  ( -56.02760103399240421, 4.702919582132905951, 2.444615905383621168 ) ) ;
#21022 = CARTESIAN_POINT ( 'NONE',  ( 13.46199999999999797, 13.84300000000000175, 1.648619521012166368E-15 ) ) ;
#21023 = CARTESIAN_POINT ( 'NONE',  ( -58.37934292759150168, 0.9822739792931106662, 1.208960021102198246 ) ) ;
#21024 = CARTESIAN_POINT ( 'NONE',  ( -58.06568617868830984, 0.9193849054837686108, 1.293020708047914802 ) ) ;
#21025 = DIRECTION ( 'NONE',  ( -6.353134868986659519E-16, 1.000000000000000000, 0.000000000000000000 ) ) ;
#21026 = CARTESIAN_POINT ( 'NONE',  ( -4.122399503745135974, 118.2429491485453497, 0.1816704820238574380 ) ) ;
#21027 = CARTESIAN_POINT ( 'NONE',  ( 3.324910422824467915, 108.2677041351605141, -4.163315910313021284 ) ) ;
#21028 = EDGE_LOOP ( 'NONE', ( #25216, #1300 ) ) ;
#21029 = CARTESIAN_POINT ( 'NONE',  ( -54.47970570282438274, 8.083255770631444292, 3.476097746275891076 ) ) ;
#21030 = VECTOR ( 'NONE', #11004, 1000.000000000000000 ) ;
#21031 = CARTESIAN_POINT ( 'NONE',  ( -4.092897794381019416, 119.2344987732284807, -0.9253235121601953717 ) ) ;
#21032 = AXIS2_PLACEMENT_3D ( 'NONE', #20456, #17480, #14278 ) ;
#21033 = CARTESIAN_POINT ( 'NONE',  ( 0.1065646865915093611, 105.8844662015456777, -5.332932678536313809 ) ) ;
#21034 = CARTESIAN_POINT ( 'NONE',  ( 4.441684112726699496, 118.1590229626581419, 0.6063474506374556539 ) ) ;
#21035 = CARTESIAN_POINT ( 'NONE',  ( -9.461503173624157270, 123.8597080710187015, -0.7891915900027407504 ) ) ;
#21036 = CARTESIAN_POINT ( 'NONE',  ( 0.3668836553635324571, 118.1651003658195833, -0.8808146135302142854 ) ) ;
#21037 = ORIENTED_EDGE ( 'NONE', *, *, #22706, .F. ) ;
#21038 = CARTESIAN_POINT ( 'NONE',  ( 3.211436584971100849, 28.15539441671475274, -3.345526564039049688 ) ) ;
#21039 = CARTESIAN_POINT ( 'NONE',  ( -2.605661685743515310, 120.2926465633240127, -0.5460719465365780900 ) ) ;
#21040 = FACE_OUTER_BOUND ( 'NONE', #20213, .T. ) ;
#21041 = DIRECTION ( 'NONE',  ( 3.035386659626960118E-16, -0.000000000000000000, 1.000000000000000000 ) ) ;
#21042 = CARTESIAN_POINT ( 'NONE',  ( -48.28978369826177186, 19.63653578263565436, 5.206999999995388428 ) ) ;
#21043 = CARTESIAN_POINT ( 'NONE',  ( -8.838968381400917451, 123.8898104212950670, -0.04432116756960934739 ) ) ;
#21044 = CARTESIAN_POINT ( 'NONE',  ( -6.263959367015712765, 28.84083519579221999, 0.1566845698765544637 ) ) ;
#21045 = CARTESIAN_POINT ( 'NONE',  ( 9.626009506019130413, 118.2334930433176652, 0.7695227696168691622 ) ) ;
#21046 = DIRECTION ( 'NONE',  ( -0.1906721105965186736, 0.9816537812491066273, 0.000000000000000000 ) ) ;
#21048 = CARTESIAN_POINT ( 'NONE',  ( 3.062634247293183787, 117.6993298527280984, -0.6308921261198919828 ) ) ;
#21047 = CARTESIAN_POINT ( 'NONE',  ( 2.350639260211558668, -15.10312717587823705, 4.966175652281853203 ) ) ;
#21049 = CARTESIAN_POINT ( 'NONE',  ( -5.904616261062859195, 156.9788419092994047, 1.696979819435221470 ) ) ;
#21050 = CARTESIAN_POINT ( 'NONE',  ( 0.4928529169951482158, -8.289340824275994279, 0.8415213476199340237 ) ) ;
#21051 = CARTESIAN_POINT ( 'NONE',  ( -8.152918552588374723, 117.7057695168643932, -0.6423243676978416250 ) ) ;
#21052 = CARTESIAN_POINT ( 'NONE',  ( 0.4517697234110209514, 20.42248995698831493, 0.8659212905253524939 ) ) ;
#21053 = ORIENTED_EDGE ( 'NONE', *, *, #8699, .T. ) ;
#21054 = CARTESIAN_POINT ( 'NONE',  ( -48.16508968810064317, 19.01313136326714925, 5.219744232931978978 ) ) ;
#21055 = CARTESIAN_POINT ( 'NONE',  ( -9.439557112687712248, 123.9587481073520223, 0.3264598115655272248 ) ) ;
#21056 = CARTESIAN_POINT ( 'NONE',  ( 2.266344692909419312, -15.23424214381746644, 5.932772278557574275 ) ) ;
#21057 = CARTESIAN_POINT ( 'NONE',  ( 5.874057931648818176, 120.5744318282211651, -0.7168624585904721513 ) ) ;
#21058 = VERTEX_POINT ( 'NONE', #8155 ) ;
#21059 = CARTESIAN_POINT ( 'NONE',  ( 2.094145466755243934, 115.7021055795812572, 1.712902155792607406 ) ) ;
#21060 = CARTESIAN_POINT ( 'NONE',  ( 3.215637690559757456, -14.25221971482225314, 3.321654998001884795 ) ) ;
#21061 = CARTESIAN_POINT ( 'NONE',  ( -4.781726760622166061, 117.4742263818998680, -1.189410900997683651 ) ) ;
#21062 = CARTESIAN_POINT ( 'NONE',  ( 7.567922279963275045, 122.4257779438054285, 0.07478732235760103542 ) ) ;
#21063 = AXIS2_PLACEMENT_3D ( 'NONE', #35386, #39005, #6836 ) ;
#21064 = VERTEX_POINT ( 'NONE', #37132 ) ;
#21065 = CARTESIAN_POINT ( 'NONE',  ( 10.23541510771056906, 120.3038588096988803, 1.551695437301547242 ) ) ;
#21066 = CARTESIAN_POINT ( 'NONE',  ( 4.038844528162431224, 111.0901538136610611, 3.207827241414232144 ) ) ;
#21067 = CIRCLE ( 'NONE', #15623, 0.6350000000000001199 ) ;
#21068 = FACE_OUTER_BOUND ( 'NONE', #3279, .T. ) ;
#21069 = CARTESIAN_POINT ( 'NONE',  ( -6.426369768295692736E-14, 159.6054662015457382, 1.032716915552223178E-16 ) ) ;
#21070 = CARTESIAN_POINT ( 'NONE',  ( 16.83721787035668171, 155.2408147041404050, 0.1288212628531383852 ) ) ;
#21071 = DIRECTION ( 'NONE',  ( -1.000000000000000000, 0.000000000000000000, 0.000000000000000000 ) ) ;
#21072 = CARTESIAN_POINT ( 'NONE',  ( 1.720506426491690055, -15.42054776992238274, 5.887968618877454041 ) ) ;
#21073 = LINE ( 'NONE', #8100, #14032 ) ;
#21074 = CARTESIAN_POINT ( 'NONE',  ( -2.938663822924134639, 31.60055309655552946, 0.8891835726407014695 ) ) ;
#21075 = CARTESIAN_POINT ( 'NONE',  ( -4.818183171710055390, 117.8426606599154667, 0.7484465901436401225 ) ) ;
#21076 = ORIENTED_EDGE ( 'NONE', *, *, #72, .T. ) ;
#21077 = CARTESIAN_POINT ( 'NONE',  ( 5.586884702347363785, 104.6144662015457243, 0.1116392523995368424 ) ) ;
#21078 = EDGE_CURVE ( 'NONE', #27616, #38171, #12860, .T. ) ;
#21079 = CARTESIAN_POINT ( 'NONE',  ( -5.733800310741941963, 118.6806198687866214, -1.226522746645787088 ) ) ;
#21080 = CARTESIAN_POINT ( 'NONE',  ( -0.8148005656458301438, 107.7619142660649203, -4.566897024910153924 ) ) ;
#21081 = CARTESIAN_POINT ( 'NONE',  ( 4.940360603511367188, 117.5341859490524996, 0.9905126371005529284 ) ) ;
#21082 = DIRECTION ( 'NONE',  ( -0.000000000000000000, -0.000000000000000000, -1.000000000000000000 ) ) ;
#21083 = CARTESIAN_POINT ( 'NONE',  ( -0.01046636458954068247, 120.7331730230139755, 0.5237796829256087250 ) ) ;
#21084 = CARTESIAN_POINT ( 'NONE',  ( 4.523211737919912601, 7.414965188139293950, 0.9565071382433593117 ) ) ;
#21085 = CARTESIAN_POINT ( 'NONE',  ( -49.01671973967525275, 18.67808020721671625, 5.174630477995037836 ) ) ;
#21086 = CARTESIAN_POINT ( 'NONE',  ( -5.031308904535771731, 113.7220012594890619, -1.867310441168415158 ) ) ;
#21087 = B_SPLINE_CURVE_WITH_KNOTS ( 'NONE', 3,
 ( #6767, #13578, #3799, #32755, #19322, #35742, #32326, #6146, #3155, #16761, #29768 ),
 .UNSPECIFIED., .F., .F.,
 ( 4, 1, 1, 1, 1, 1, 1, 1, 4 ),
 ( 0.000000000000000000, 0.1250000000000006939, 0.2500000000000013878, 0.3750000000000020539, 0.5000000000000027756, 0.6250000000000061062, 0.7499999999999986677, 0.8750000000000019984, 1.000000000000000000 ),
 .UNSPECIFIED. ) ;
#21088 = CARTESIAN_POINT ( 'NONE',  ( 3.509037099356659084, -13.47856448578629873, 2.732507022889707038 ) ) ;
#21089 = CARTESIAN_POINT ( 'NONE',  ( 3.375001179497614689, 119.3320731715853782, -0.4843141097021076980 ) ) ;
#21090 = CARTESIAN_POINT ( 'NONE',  ( 2.383981540283352629, 36.81846344528510429, 1.803752045214197297 ) ) ;
#21091 = CARTESIAN_POINT ( 'NONE',  ( -0.7849891123721223218, 115.7029491485453434, 1.726829941792507483 ) ) ;
#21092 = ORIENTED_EDGE ( 'NONE', *, *, #32590, .T. ) ;
#21093 = CARTESIAN_POINT ( 'NONE',  ( -17.32429653712378936, 61.56493206124108042, 1.269999999999999796 ) ) ;
#21094 = CARTESIAN_POINT ( 'NONE',  ( 1.925067723532086994, -15.61332249492565438, 5.452854070638914585 ) ) ;
#21095 = CARTESIAN_POINT ( 'NONE',  ( -1.091998727716720241, 158.1148137021529578, 1.603323485041850294 ) ) ;
#21096 = CARTESIAN_POINT ( 'NONE',  ( 0.4504873307288463358, 16.48674109716143477, 0.8651787211232140340 ) ) ;
#21097 = ADVANCED_FACE ( 'NONE', ( #30520 ), #26956, .F. ) ;
#21098 = EDGE_LOOP ( 'NONE', ( #17609, #27715, #1332, #19144 ) ) ;
#21099 = ORIENTED_EDGE ( 'NONE', *, *, #21410, .T. ) ;
#21100 = CARTESIAN_POINT ( 'NONE',  ( -4.112981969563189288, 27.92417664812854738, 0.5059177812967017296 ) ) ;
#21101 = CARTESIAN_POINT ( 'NONE',  ( 2.258874542396673846, 118.3648483361698851, 0.8858652710056679203 ) ) ;
#21102 = CARTESIAN_POINT ( 'NONE',  ( -16.33516936551327703, 148.1602266505728380, 1.109112510451941924 ) ) ;
#21103 = DIRECTION ( 'NONE',  ( -1.000000000000000000, 1.044409991968846932E-16, 0.000000000000000000 ) ) ;
#21104 = CARTESIAN_POINT ( 'NONE',  ( 4.732466489211092586, 117.9644445172183538, -0.6135672020651322667 ) ) ;
#21105 = CARTESIAN_POINT ( 'NONE',  ( 7.569905091580497292, 156.0351187175861867, -1.610277000873165054 ) ) ;
#21106 = CARTESIAN_POINT ( 'NONE',  ( -15.97272115206789955, 153.3736753708079732, -2.320099718173297187 ) ) ;
#21107 = CARTESIAN_POINT ( 'NONE',  ( 11.04921058900168518, 56.51500000000000057, 4.436160551868583823 ) ) ;
#21108 = AXIS2_PLACEMENT_3D ( 'NONE', #36846, #8072, #21046 ) ;
#21109 = CARTESIAN_POINT ( 'NONE',  ( 4.248835768063355722, 118.2248660469010559, -0.3116667286827642380 ) ) ;
#21110 = CARTESIAN_POINT ( 'NONE',  ( 13.73699108721713458, 150.2158912636999730, -0.3005180155469768244 ) ) ;
#21111 = EDGE_LOOP ( 'NONE', ( #35959, #7611, #37184, #5551 ) ) ;
#21112 = CARTESIAN_POINT ( 'NONE',  ( 2.349528287245666647, -15.15257587461875310, 4.947206973663434759 ) ) ;
#21113 = CARTESIAN_POINT ( 'NONE',  ( 10.54112285291057916, 57.14999999999387370, -5.016500000000000625 ) ) ;
#21114 = CARTESIAN_POINT ( 'NONE',  ( -57.89036626108653394, 0.7933261799628198441, 1.256022413937592175 ) ) ;
#21115 = CARTESIAN_POINT ( 'NONE',  ( -4.603752034695621553, -0.9465464349810851497, 0.4006815057252178236 ) ) ;
#21116 = CARTESIAN_POINT ( 'NONE',  ( 12.90748236152450623, 128.4900567078429390, 1.625332807165861260 ) ) ;
#21117 = CARTESIAN_POINT ( 'NONE',  ( 2.971218050981001113, 39.20946620154573736, 0.6944987714346865237 ) ) ;
#21118 = CARTESIAN_POINT ( 'NONE',  ( -4.048024155119399836, 117.4230540797109938, 0.8140401526052126746 ) ) ;
#21119 = CARTESIAN_POINT ( 'NONE',  ( -3.426874451426485724, 1.805113900313119357, -3.130497002818263930 ) ) ;
#21120 = CARTESIAN_POINT ( 'NONE',  ( 11.85559104777363082, 130.3381101163291760, 0.2804367443601422649 ) ) ;
#21121 = CARTESIAN_POINT ( 'NONE',  ( -11.66725022230187214, 55.42194143536246287, 5.016499999999784798 ) ) ;
#21122 = EDGE_CURVE ( 'NONE', #18118, #20396, #27853, .T. ) ;
#21123 = CARTESIAN_POINT ( 'NONE',  ( -57.55293229875817218, 1.419684655164468623, -1.132508401016395716 ) ) ;
#21124 = CARTESIAN_POINT ( 'NONE',  ( 2.170629307524321927, 116.6785980183682625, -0.3802400742865192917 ) ) ;
#21125 = DIRECTION ( 'NONE',  ( -0.7770581983690864059, 0.6294287539884000360, -8.537024980200833651E-16 ) ) ;
#21126 = DIRECTION ( 'NONE',  ( -0.1906721105965186736, 0.9816537812491066273, 0.000000000000000000 ) ) ;
#21127 = CARTESIAN_POINT ( 'NONE',  ( 1.824656174747253168, -15.25388738520313225, 5.420764384989097628 ) ) ;
#21128 = CARTESIAN_POINT ( 'NONE',  ( 4.559522851259544041, 6.111780172613243245, 7.100340242056582873 ) ) ;
#21129 = CARTESIAN_POINT ( 'NONE',  ( 5.332923298845091864, 115.7029491485453150, 0.1071700043820369153 ) ) ;
#21130 = CARTESIAN_POINT ( 'NONE',  ( -24.49496359545907964, 76.94162913054094588, 1.269999999999993578 ) ) ;
#21131 = CARTESIAN_POINT ( 'NONE',  ( 2.102813808753936087, -15.18136450426021256, 5.202461169095355942 ) ) ;
#21132 = CARTESIAN_POINT ( 'NONE',  ( 0.07831152689291247249, 109.4728569552520838, -3.919029035233798641 ) ) ;
#21133 = CARTESIAN_POINT ( 'NONE',  ( -0.9570688389944551622, 116.7004868406603322, 0.2253703713229212591 ) ) ;
#21134 = VERTEX_POINT ( 'NONE', #31047 ) ;
#21135 = DIRECTION ( 'NONE',  ( 0.1469470846586743706, 9.335746474409589170E-17, -0.9891443546370348727 ) ) ;
#21136 = ORIENTED_EDGE ( 'NONE', *, *, #36077, .T. ) ;
#21137 = CARTESIAN_POINT ( 'NONE',  ( -45.93641268020883928, 20.77718376653855614, -4.359287402722206828 ) ) ;
#21139 = CARTESIAN_POINT ( 'NONE',  ( -10.39928917620371784, 153.1223395828141918, -0.2078025466733117443 ) ) ;
#21138 = CIRCLE ( 'NONE', #19769, 0.6350000000000006750 ) ;
#21140 = CARTESIAN_POINT ( 'NONE',  ( 3.037190435423921642, -15.45437603076259236, 5.639675387367293347 ) ) ;
#21141 = CARTESIAN_POINT ( 'NONE',  ( -2.760819571866494293, 158.5977336698458089, 1.488126253378572406 ) ) ;
#21142 = CARTESIAN_POINT ( 'NONE',  ( 21.83270838041246975, 150.5404744109896171, -0.8586010584139893709 ) ) ;
#21143 = CARTESIAN_POINT ( 'NONE',  ( -4.191205975170537279, 21.45845178295031630, -1.961646697876042511 ) ) ;
#21144 = CARTESIAN_POINT ( 'NONE',  ( -13.43369120214920365, 119.6710471929552000, -0.6668731667128946494 ) ) ;
#21145 = CARTESIAN_POINT ( 'NONE',  ( -50.78742080704162731, 15.01002293501888118, -4.744323022696246284 ) ) ;
#21146 = EDGE_LOOP ( 'NONE', ( #4003, #33710, #34346, #4019 ) ) ;
#21147 = CARTESIAN_POINT ( 'NONE',  ( 6.059261036834405978, 56.51500000000000057, 4.381499999999999950 ) ) ;
#21148 = CARTESIAN_POINT ( 'NONE',  ( -23.91048590848665611, 81.84235438443283783, -1.524000000000006239 ) ) ;
#21149 = CARTESIAN_POINT ( 'NONE',  ( -5.873575024772843101, 120.4133487461328826, 0.7716123655894260303 ) ) ;
#21150 = CARTESIAN_POINT ( 'NONE',  ( 5.078986093043053707, 98.39146620154573952, 0.1014902294541244060 ) ) ;
#21151 = CARTESIAN_POINT ( 'NONE',  ( 6.044862153450403675, 157.1185343457808301, -1.711190705598350403 ) ) ;
#21152 = CARTESIAN_POINT ( 'NONE',  ( -1.092003032498587212, 117.6437429425539420, -0.5722403007656916563 ) ) ;
#21153 = CARTESIAN_POINT ( 'NONE',  ( -46.89970385779243855, 22.02655025333852379, -4.237790764466935478 ) ) ;
#21154 = ADVANCED_FACE ( 'NONE', ( #1886 ), #6071, .F. ) ;
#21155 = CARTESIAN_POINT ( 'NONE',  ( 10.90887028606290876, 153.1125297277760069, -0.8016274872379887118 ) ) ;
#21156 = VERTEX_POINT ( 'NONE', #38082 ) ;
#21157 = CARTESIAN_POINT ( 'NONE',  ( -11.19992112824931496, 154.5781333488962446, -2.119767339128325823 ) ) ;
#21158 = CARTESIAN_POINT ( 'NONE',  ( 4.206901174280650579, -15.33509931759592604, 0.05204670666830889247 ) ) ;
#21159 = CARTESIAN_POINT ( 'NONE',  ( -4.444388996687162141, 118.1581009083410976, -0.6033315295914259968 ) ) ;
#21160 = CARTESIAN_POINT ( 'NONE',  ( -57.50953982388014651, 1.662011999372992044, -1.631050346940590812 ) ) ;
#21161 = CARTESIAN_POINT ( 'NONE',  ( -4.971548125946218200, 117.4753602155310404, 0.8635831801788802498 ) ) ;
#21162 = CARTESIAN_POINT ( 'NONE',  ( 11.03566430468803361, 123.0430266451958232, 1.599512106649902510 ) ) ;
#21163 = EDGE_CURVE ( 'NONE', #30281, #24814, #8097, .T. ) ;
#21164 = FACE_OUTER_BOUND ( 'NONE', #41645, .T. ) ;
#21165 = CIRCLE ( 'NONE', #6245, 16.60960244842765832 ) ;
#21166 = CARTESIAN_POINT ( 'NONE',  ( 23.11179153581189993, 149.9001102426712748, 0.4361622115260940236 ) ) ;
#21167 = CARTESIAN_POINT ( 'NONE',  ( -3.982871878373832164, -5.105173558950587775, 7.419718595111914894 ) ) ;
#21168 = CARTESIAN_POINT ( 'NONE',  ( 9.239529650026105045, 153.8817031120973411, 0.7017441744976311568 ) ) ;
#21169 = DIRECTION ( 'NONE',  ( -0.01731298258487590572, 0.9998501190848636533, -3.136208412989023577E-15 ) ) ;
#21170 = EDGE_CURVE ( 'NONE', #38620, #33803, #29875, .T. ) ;
#21171 = CARTESIAN_POINT ( 'NONE',  ( -42.88395384449221126, 21.55219572468337219, -1.583305067638075769 ) ) ;
#21172 = CARTESIAN_POINT ( 'NONE',  ( -2.802975543813512882, 117.9394509414842531, 1.218220532187687999 ) ) ;
#21173 = TOROIDAL_SURFACE ( 'NONE', #21032, 0.3810000000000001719, 0.2540000000000000036 ) ;
#21174 = CARTESIAN_POINT ( 'NONE',  ( 3.946153427423682469, 118.7629491485453741, 1.103408776148272930 ) ) ;
#21175 = ADVANCED_FACE ( 'NONE', ( #34467 ), #315, .T. ) ;
#21176 = CARTESIAN_POINT ( 'NONE',  ( -58.03414100541873211, 0.4564111095344824953, 0.9708715263941498641 ) ) ;
#21177 = CARTESIAN_POINT ( 'NONE',  ( -53.84631020981186822, 15.55534180636754193, -1.017045832751381207E-14 ) ) ;
#21178 = CARTESIAN_POINT ( 'NONE',  ( -15.18069129733363098, 156.1124880001465556, -0.1695137023582057034 ) ) ;
#21179 = ORIENTED_EDGE ( 'NONE', *, *, #12597, .F. ) ;
#21180 = CARTESIAN_POINT ( 'NONE',  ( -49.23607562092252721, 19.66429951101446960, -3.974467759520302401 ) ) ;
#21181 = CARTESIAN_POINT ( 'NONE',  ( 7.883489662030576994, 122.2086137271560062, -0.4845574022495899302 ) ) ;
#21182 = CARTESIAN_POINT ( 'NONE',  ( -8.060916924639437653, 121.3839393899242936, 0.8986322262797288296 ) ) ;
#21183 = CARTESIAN_POINT ( 'NONE',  ( 0.02551629667430791934, 118.7629491485454025, -1.276939826302095682 ) ) ;
#21184 = CARTESIAN_POINT ( 'NONE',  ( -12.03016689884997525, 130.4833683797432684, -0.5359549021282030701 ) ) ;
#21185 = CARTESIAN_POINT ( 'NONE',  ( 2.867264926914522949, -14.81558118910870903, 5.578245215537346979 ) ) ;
#21186 = CIRCLE ( 'NONE', #2867, 0.7620000000000015650 ) ;
#21187 = CARTESIAN_POINT ( 'NONE',  ( -5.164160201466208022, 158.7070047875298826, 1.240540739692759020 ) ) ;
#21188 = FACE_OUTER_BOUND ( 'NONE', #6933, .T. ) ;
#21189 = AXIS2_PLACEMENT_3D ( 'NONE', #41276, #24429, #12082 ) ;
#21190 = CARTESIAN_POINT ( 'NONE',  ( 9.792313404876027860, 118.0024801742749929, 0.3345192158099828950 ) ) ;
#21191 = CARTESIAN_POINT ( 'NONE',  ( 15.52593806990746472, 147.5347896062808957, 0.3770146343057313443 ) ) ;
#21192 = CARTESIAN_POINT ( 'NONE',  ( 6.984999999999963904, 56.51500000000000057, 8.554157892044261576E-16 ) ) ;
#21193 = CARTESIAN_POINT ( 'NONE',  ( -0.9394305312890779414, 22.53537758578342931, -0.2615529312561373776 ) ) ;
#21194 = CARTESIAN_POINT ( 'NONE',  ( -1.421330246821875587, 159.6054662015457666, -0.04208995589191817654 ) ) ;
#21195 = CARTESIAN_POINT ( 'NONE',  ( -47.85244527695891037, 19.39403540832952544, -5.219971639306605127 ) ) ;
#21196 = ORIENTED_EDGE ( 'NONE', *, *, #17162, .T. ) ;
#21197 = DIRECTION ( 'NONE',  ( 0.000000000000000000, 0.000000000000000000, -1.000000000000000000 ) ) ;
#21198 = EDGE_CURVE ( 'NONE', #26767, #12920, #9459, .T. ) ;
#21199 = ORIENTED_EDGE ( 'NONE', *, *, #1448, .F. ) ;
#21200 = CARTESIAN_POINT ( 'NONE',  ( -3.563367352916122499, 117.8600736429027478, 0.7435805097010282916 ) ) ;
#21201 = CARTESIAN_POINT ( 'NONE',  ( -5.327983418387242764, 105.1224763138612843, 0.2702714856519077280 ) ) ;
#21202 = CARTESIAN_POINT ( 'NONE',  ( 21.61975215418284790, 149.3076860495818323, 2.139488579489919218 ) ) ;
#21203 = CARTESIAN_POINT ( 'NONE',  ( -56.37342374758011232, 3.980281407817629180, -2.237022232195863936 ) ) ;
#21204 = CARTESIAN_POINT ( 'NONE',  ( 20.06821085608255473, 149.3093937917295762, -1.664735353294634068 ) ) ;
#21205 = CARTESIAN_POINT ( 'NONE',  ( -5.272568914482754998, 19.56627864152888208, 6.568537450970175939 ) ) ;
#21206 = CARTESIAN_POINT ( 'NONE',  ( -22.55218723263380909, 148.5212373274837319, -1.758973660241909487 ) ) ;
#21207 = CARTESIAN_POINT ( 'NONE',  ( 4.933441418498765607, 117.6566197977928852, -0.7552850541079862978 ) ) ;
#21208 = ORIENTED_EDGE ( 'NONE', *, *, #13651, .F. ) ;
#21209 = CARTESIAN_POINT ( 'NONE',  ( -15.77919907218852025, 145.7191243368997675, 0.01646358168407728237 ) ) ;
#21210 = CARTESIAN_POINT ( 'NONE',  ( 6.028374245061780989, -14.54558069259788411, 1.726931113533916040 ) ) ;
#21211 = CARTESIAN_POINT ( 'NONE',  ( 13.85159022459154876, 16.68226173831723003, -5.016499999999999737 ) ) ;
#21212 = ADVANCED_FACE ( 'NONE', ( #24437 ), #8263, .F. ) ;
#21213 = DIRECTION ( 'NONE',  ( -0.8745520943968250194, 0.4849315768086535083, -5.361993529360574930E-16 ) ) ;
#21214 = ORIENTED_EDGE ( 'NONE', *, *, #39678, .T. ) ;
#21215 = CARTESIAN_POINT ( 'NONE',  ( 6.656653968793884601, 119.6463993818898359, 1.283952750486249794 ) ) ;
#21216 = DIRECTION ( 'NONE',  ( -0.8745520943967910465, 0.4849315768087146816, -5.424246918827960064E-16 ) ) ;
#21217 = CARTESIAN_POINT ( 'NONE',  ( -3.682264917456323783, 85.18346620154574111, -0.07358041635423968885 ) ) ;
#21218 = CARTESIAN_POINT ( 'NONE',  ( -3.315449255180983545, 124.9344662015457743, -0.06625056644921972770 ) ) ;
#21219 = CARTESIAN_POINT ( 'NONE',  ( -5.217102898550305845, -11.97038331068927342, -6.647077075081065267 ) ) ;
#21220 = CARTESIAN_POINT ( 'NONE',  ( 9.561025033427959841, 123.8224200044116827, 0.8726585919039498984 ) ) ;
#21221 = CARTESIAN_POINT ( 'NONE',  ( -4.787902336757507094, 118.5930653697794384, -0.9393770334760460639 ) ) ;
#21222 = CARTESIAN_POINT ( 'NONE',  ( 15.31827776641168271, 121.1074504348956964, -0.3839962087354598652 ) ) ;
#21223 = CARTESIAN_POINT ( 'NONE',  ( -17.97610982144389524, 83.97333317030323485, -1.270000000000003348 ) ) ;
#21224 = CARTESIAN_POINT ( 'NONE',  ( -58.04761505321778259, 0.4012412707330069161, 0.7940720734374372425 ) ) ;
#21225 = CARTESIAN_POINT ( 'NONE',  ( -33.20758249455312239, 49.81222039523557044, -1.524000000000005572 ) ) ;
#21226 = EDGE_CURVE ( 'NONE', #30442, #26111, #639, .T. ) ;
#21227 = CARTESIAN_POINT ( 'NONE',  ( -49.39499541695917628, 17.24413359080933006, 5.048280001787422755 ) ) ;
#21228 = CARTESIAN_POINT ( 'NONE',  ( -6.538677740023618411E-14, 75.27746620154573520, -7.356392042280733227E-18 ) ) ;
#21229 = CARTESIAN_POINT ( 'NONE',  ( -4.270517806291405982, 118.2236137968261716, 0.2873848592035506688 ) ) ;
#21230 = AXIS2_PLACEMENT_3D ( 'NONE', #5229, #8618, #37377 ) ;
#21231 = CARTESIAN_POINT ( 'NONE',  ( -4.476425760464393555, 71.61790547347303004, -1.269999999999994245 ) ) ;
#21232 = ORIENTED_EDGE ( 'NONE', *, *, #40967, .T. ) ;
#21233 = CARTESIAN_POINT ( 'NONE',  ( -54.77668461537430034, 8.146287316968315650, 3.518595155146524434 ) ) ;
#21234 = CARTESIAN_POINT ( 'NONE',  ( -6.140969379225402314, 119.6263759229288155, -1.248624756452694884 ) ) ;
#21235 = CARTESIAN_POINT ( 'NONE',  ( -23.69188486464780752, 78.08202335040543574, -1.524000000000005350 ) ) ;
#21236 = CARTESIAN_POINT ( 'NONE',  ( 4.226304903563289805, 118.2242387644281365, 0.4878455849994780547 ) ) ;
#21237 = CARTESIAN_POINT ( 'NONE',  ( -6.479597433594425304, 121.6155390319085683, -0.5171962410403524446 ) ) ;
#21238 = DIRECTION ( 'NONE',  ( -9.627370216492862708E-17, -1.000000000000000000, 0.000000000000000000 ) ) ;
#21239 = DIRECTION ( 'NONE',  ( 1.000000000000000000, -1.011795553208986377E-16, 0.000000000000000000 ) ) ;
#21240 = ORIENTED_EDGE ( 'NONE', *, *, #12698, .F. ) ;
#21241 = CARTESIAN_POINT ( 'NONE',  ( -0.3239230800893593276, 29.42979164457532804, -4.628216972995994993 ) ) ;
#21242 = CARTESIAN_POINT ( 'NONE',  ( -16.69533394573253915, 146.9696287467501179, -1.777152765835339654 ) ) ;
#21243 = DIRECTION ( 'NONE',  ( 0.3256999990547865265, 0.9454731675810330582, 7.920142172900908730E-15 ) ) ;
#21244 = FACE_OUTER_BOUND ( 'NONE', #41182, .T. ) ;
#21245 = CARTESIAN_POINT ( 'NONE',  ( -48.12235166104741779, 19.54369616526484776, 5.380337212813706138 ) ) ;
#21246 = CARTESIAN_POINT ( 'NONE',  ( 6.071556415024221387, 121.4181341445724911, 0.3301129433361331689 ) ) ;
#21247 = CARTESIAN_POINT ( 'NONE',  ( -0.2796867633624597893, 20.41853924017881283, 4.627572958784220702 ) ) ;
#21248 = CARTESIAN_POINT ( 'NONE',  ( 15.26873630740953480, 121.3917326167944708, 1.149126527656483265 ) ) ;
#21249 = DIRECTION ( 'NONE',  ( 0.000000000000000000, -0.000000000000000000, 1.000000000000000000 ) ) ;
#21251 = CARTESIAN_POINT ( 'NONE',  ( 21.00062727315619782, 150.0074445146613584, -1.385517290469731044 ) ) ;
#21250 = CARTESIAN_POINT ( 'NONE',  ( 2.856221160286674277, -14.96258862872340600, 4.237710179968991575 ) ) ;
#21252 = CARTESIAN_POINT ( 'NONE',  ( -11.86655615995746693, 122.9427978038690270, 1.277170931065712667 ) ) ;
#21253 = CARTESIAN_POINT ( 'NONE',  ( -4.137704358559117779, 17.39492794009094823, -2.099109474953318788 ) ) ;
#21254 = CARTESIAN_POINT ( 'NONE',  ( -1.924101685567954689, 116.8467566806161386, -0.3833193769953582852 ) ) ;
#21255 = CIRCLE ( 'NONE', #31452, 0.2539999999999992819 ) ;
#21256 = CARTESIAN_POINT ( 'NONE',  ( -0.01433812918766144522, 10.07226683256953947, 0.9740319587662029654 ) ) ;
#21257 = ORIENTED_EDGE ( 'NONE', *, *, #27362, .F. ) ;
#21258 = CARTESIAN_POINT ( 'NONE',  ( -50.52646075385809610, 14.05410990099204049, 2.888145277534006627 ) ) ;
#21259 = CARTESIAN_POINT ( 'NONE',  ( -1.677891416185295803, 156.3096136994911092, 0.5101806352362401320 ) ) ;
#21260 = CARTESIAN_POINT ( 'NONE',  ( 5.886196856236641572, -12.36517754215322995, 0.8550893866892870232 ) ) ;
#21261 = CARTESIAN_POINT ( 'NONE',  ( 17.27635908418598021, 147.1820577694790018, -1.364000445115660654 ) ) ;
#21262 = VERTEX_POINT ( 'NONE', #9731 ) ;
#21263 = CARTESIAN_POINT ( 'NONE',  ( 1.783695439853289377, 115.7029489856815019, 1.723415406732235811 ) ) ;
#21264 = AXIS2_PLACEMENT_3D ( 'NONE', #6748, #35298, #32952 ) ;
#21265 = VERTEX_POINT ( 'NONE', #38710 ) ;
#21266 = CARTESIAN_POINT ( 'NONE',  ( 3.381076509412870301, -13.31623885458479961, 2.121725202727857695 ) ) ;
#21267 = CARTESIAN_POINT ( 'NONE',  ( -4.830385371082315693, 117.7605833166150404, -0.9792491193852199682 ) ) ;
#21268 = CARTESIAN_POINT ( 'NONE',  ( 0.6421132086018013219, 120.9975462804897433, -0.01250379197263685321 ) ) ;
#21269 = VECTOR ( 'NONE', #30825, 1000.000000000000227 ) ;
#21270 = ORIENTED_EDGE ( 'NONE', *, *, #31562, .T. ) ;
#21271 = CARTESIAN_POINT ( 'NONE',  ( 7.739031927414979251, 119.2688035297948659, 1.343379870322972458 ) ) ;
#21272 = CYLINDRICAL_SURFACE ( 'NONE', #32665, 0.2540000000000030012 ) ;
#21273 = DIRECTION ( 'NONE',  ( 0.000000000000000000, -1.000000000000000000, 0.000000000000000000 ) ) ;
#21274 = CARTESIAN_POINT ( 'NONE',  ( 0.004910662370358964517, 159.5928157220454295, -0.2457496255665020946 ) ) ;
#21275 = CARTESIAN_POINT ( 'NONE',  ( 5.806485631242116696, 116.9771394561422539, -0.05772921648981169107 ) ) ;
#21276 = CARTESIAN_POINT ( 'NONE',  ( -10.93398011767285283, 82.89560043784887000, -1.523999999999999577 ) ) ;
#21277 = AXIS2_PLACEMENT_3D ( 'NONE', #20002, #36002, #26188 ) ;
#21278 = CARTESIAN_POINT ( 'NONE',  ( 1.643874335733584768, -15.34739276353720783, 5.606459198667521626 ) ) ;
#21279 = DIRECTION ( 'NONE',  ( -0.000000000000000000, -0.000000000000000000, -1.000000000000000000 ) ) ;
#21280 = DIRECTION ( 'NONE',  ( 5.463695987328526437E-16, -1.000000000000000000, -1.672774450599033775E-31 ) ) ;
#21281 = CARTESIAN_POINT ( 'NONE',  ( -4.706055329038499657, 117.9791134883193848, 0.6571109466785158837 ) ) ;
#21282 = ORIENTED_EDGE ( 'NONE', *, *, #38382, .T. ) ;
#21283 = ORIENTED_EDGE ( 'NONE', *, *, #11250, .T. ) ;
#21284 = FACE_OUTER_BOUND ( 'NONE', #8169, .T. ) ;
#21285 = CARTESIAN_POINT ( 'NONE',  ( 8.584051096561029937, 118.8309510801975932, -0.8814915625618818806 ) ) ;
#21286 = CARTESIAN_POINT ( 'NONE',  ( -4.467639297143111143, 123.9529229959338608, -0.1358511699341444778 ) ) ;
#21287 = CARTESIAN_POINT ( 'NONE',  ( 4.868692240912165126, 117.7191721330082572, 0.9439216475803462458 ) ) ;
#21288 = DIRECTION ( 'NONE',  ( -6.146657985744592735E-16, 3.905054717696928257E-31, 1.000000000000000000 ) ) ;
#21289 = CARTESIAN_POINT ( 'NONE',  ( -0.7907195946117820951, 120.5370721568272216, 0.4966358104988965461 ) ) ;
#21290 = AXIS2_PLACEMENT_3D ( 'NONE', #2503, #21213, #15039 ) ;
#21291 = CARTESIAN_POINT ( 'NONE',  ( -0.8472427164685307766, -8.777537934218566207, -4.544909406875613733 ) ) ;
#21292 = CARTESIAN_POINT ( 'NONE',  ( 4.997288873896878592, 117.4043910709748104, -0.8233982764724142589 ) ) ;
#21293 = DIRECTION ( 'NONE',  ( -0.8745520943968235761, 0.4849315768086558398, -4.268512490100410909E-16 ) ) ;
#21294 = CARTESIAN_POINT ( 'NONE',  ( 3.107604131292615257, -12.52806217606054773, 0.6782401946156415562 ) ) ;
#21295 = CARTESIAN_POINT ( 'NONE',  ( 2.433495328593811902, 107.4436264546101967, -4.557236999380250175 ) ) ;
#21296 = CARTESIAN_POINT ( 'NONE',  ( -0.9149567752697735923, 32.47697140010484418, 3.785418454572507141 ) ) ;
#21297 = CARTESIAN_POINT ( 'NONE',  ( -0.6166778457948044467, 115.7029855731295811, 1.738056368063223944 ) ) ;
#21298 = CARTESIAN_POINT ( 'NONE',  ( 3.400481176189167343, 25.78150505744974552, 3.158589348000393482 ) ) ;
#21299 = ORIENTED_EDGE ( 'NONE', *, *, #11563, .T. ) ;
#21300 = CARTESIAN_POINT ( 'NONE',  ( -5.282606327573863503, 104.6144662015414184, -0.7587477978234113962 ) ) ;
#21301 = CARTESIAN_POINT ( 'NONE',  ( 3.676215660907734328, -15.61639409997438221, 3.572853394304201569 ) ) ;
#21302 = CARTESIAN_POINT ( 'NONE',  ( -17.46034360794361007, 151.5007859583534753, 1.733980983366192552 ) ) ;
#21303 = CARTESIAN_POINT ( 'NONE',  ( 0.7683055643446228267, 21.07255974867073078, 0.6014680952941496850 ) ) ;
#21304 = CARTESIAN_POINT ( 'NONE',  ( -0.6395729929254629909, 24.25746453972198680, 0.7366970655621520869 ) ) ;
#21305 = ORIENTED_EDGE ( 'NONE', *, *, #12262, .T. ) ;
#21306 = ORIENTED_EDGE ( 'NONE', *, *, #38625, .T. ) ;
#21307 = CARTESIAN_POINT ( 'NONE',  ( 0.7055264248721295761, 108.7514562038770976, 4.178308661695779413 ) ) ;
#21308 = CARTESIAN_POINT ( 'NONE',  ( -6.522410937005572507, 121.2869106855140018, 0.5334890203407733900 ) ) ;
#21309 = CARTESIAN_POINT ( 'NONE',  ( -30.37855815223275258, 71.48694267763936239, -1.270000000000007567 ) ) ;
#21310 = CARTESIAN_POINT ( 'NONE',  ( 4.687054664522481318, 118.0074822305351319, -0.5902932124156423654 ) ) ;
#21311 = CARTESIAN_POINT ( 'NONE',  ( 14.27712035414119107, 128.5469532985352714, -1.439506347022430299 ) ) ;
#21312 = AXIS2_PLACEMENT_3D ( 'NONE', #12255, #25248, #22034 ) ;
#21313 = CARTESIAN_POINT ( 'NONE',  ( -20.07331991451315645, 148.0303212619860744, -2.505472171123445335 ) ) ;
#21314 = DIRECTION ( 'NONE',  ( 0.9876665170007974393, -0.1565721916417901483, 8.537024980200831679E-16 ) ) ;
#21315 = CARTESIAN_POINT ( 'NONE',  ( -6.441001096823943506, 29.32969738650800551, -0.01017983961634279927 ) ) ;
#21316 = AXIS2_PLACEMENT_3D ( 'NONE', #7416, #33399, #20170 ) ;
#21317 = CARTESIAN_POINT ( 'NONE',  ( 9.493134470504843492, 124.1929984354129175, -0.2364027771656554699 ) ) ;
#21318 = ORIENTED_EDGE ( 'NONE', *, *, #27411, .F. ) ;
#21319 = CARTESIAN_POINT ( 'NONE',  ( 3.028202472743143581, -14.11696900735987015, 1.123381337427139526 ) ) ;
#21320 = CARTESIAN_POINT ( 'NONE',  ( 11.55299880265467571, 55.57741982016698046, -4.472382752598256239 ) ) ;
#21321 = CARTESIAN_POINT ( 'NONE',  ( -55.40724689662754088, 6.067898552042457538, 3.000206617154345778 ) ) ;
#21322 = CARTESIAN_POINT ( 'NONE',  ( 4.264856162967361364, -5.269518785209044154, -1.792273654951743067 ) ) ;
#21323 = CARTESIAN_POINT ( 'NONE',  ( 3.288791919378179163, 156.3062290909284116, 1.149731754608032785 ) ) ;
#21324 = CARTESIAN_POINT ( 'NONE',  ( -2.690315046239569075, 30.48488075981191159, 3.827843980145978264 ) ) ;
#21325 = CARTESIAN_POINT ( 'NONE',  ( -4.642736441617746124, 114.7252160460498516, 1.690332539979629622 ) ) ;
#21326 = AXIS2_PLACEMENT_3D ( 'NONE', #33000, #29146, #22735 ) ;
#21327 = CARTESIAN_POINT ( 'NONE',  ( -3.998286381996895233, 3.741657206818807424, 2.332027183294827832 ) ) ;
#21328 = CARTESIAN_POINT ( 'NONE',  ( 6.499560145427067503, 121.7799842514348541, 0.1589113151347880393 ) ) ;
#21329 = CARTESIAN_POINT ( 'NONE',  ( 8.368836169178564433, 3.587476746713724740, 1.217019533931793074 ) ) ;
#21330 = CARTESIAN_POINT ( 'NONE',  ( -57.57967628038989005, 1.451576601202167360, -1.494865757154152153 ) ) ;
#21331 = CARTESIAN_POINT ( 'NONE',  ( 5.529029624460691572, 116.9734914006921684, -0.4280831465535851477 ) ) ;
#21332 = DIRECTION ( 'NONE',  ( 5.188838149069472160E-16, -1.699382548006136559E-16, -1.000000000000000000 ) ) ;
#21333 = DIRECTION ( 'NONE',  ( -0.8745520943968235761, 0.4849315768086558953, -5.361993529360570985E-16 ) ) ;
#21334 = CARTESIAN_POINT ( 'NONE',  ( 5.274109024393328404, 115.7029491485453150, -0.8140283081321303404 ) ) ;
#21335 = CARTESIAN_POINT ( 'NONE',  ( 3.595709101656964890, 5.917279480223868404, 7.636340781540109646 ) ) ;
#21336 = CARTESIAN_POINT ( 'NONE',  ( 2.526652830164346053, 118.1588881379252456, 0.8392714833404777419 ) ) ;
#21337 = DIRECTION ( 'NONE',  ( -0.9998036453533934997, -0.0004114442613340082121, -0.01981164939336589603 ) ) ;
#21338 = CARTESIAN_POINT ( 'NONE',  ( -58.83227707057485389, -0.08366279997994163775, -1.543118586181777983E-14 ) ) ;
#21339 = CARTESIAN_POINT ( 'NONE',  ( 1.058771226886385586, 124.8229041592835387, 0.01153269281271733331 ) ) ;
#21340 = CARTESIAN_POINT ( 'NONE',  ( -15.29680631459152806, 120.8527393138689376, 0.2092734171533192633 ) ) ;
#21341 = ORIENTED_EDGE ( 'NONE', *, *, #22509, .F. ) ;
#21342 = DIRECTION ( 'NONE',  ( -4.017660918040594346E-17, 1.000000000000000000, 2.376309959284834438E-19 ) ) ;
#21343 = ORIENTED_EDGE ( 'NONE', *, *, #2757, .F. ) ;
#21344 = CARTESIAN_POINT ( 'NONE',  ( -47.22690022493117112, 20.09066223305544341, -5.151063612126583813 ) ) ;
#21345 = CARTESIAN_POINT ( 'NONE',  ( -9.538359384048678891, 124.8019839352694476, -0.1905991205270209377 ) ) ;
#21346 = CARTESIAN_POINT ( 'NONE',  ( 4.127870218248371970, -15.50624122109489633, 4.747786349039386344 ) ) ;
#21347 = CARTESIAN_POINT ( 'NONE',  ( -13.89335097268686070, 122.2371923977168109, 1.173247377384143642 ) ) ;
#21348 = AXIS2_PLACEMENT_3D ( 'NONE', #29141, #7009, #3823 ) ;
#21349 = CARTESIAN_POINT ( 'NONE',  ( 21.93433297169870144, 150.0588410196355937, -0.9994452811612329901 ) ) ;
#21350 = CARTESIAN_POINT ( 'NONE',  ( -3.854280124997887746, 21.23357344512866973, -2.551540157904111261 ) ) ;
#21351 = CARTESIAN_POINT ( 'NONE',  ( -15.70536794749891385, 121.0099257824619627, -0.6352152019007782924 ) ) ;
#21352 = CARTESIAN_POINT ( 'NONE',  ( -48.71344905023164529, 18.25307053356915787, -5.161295349598031379 ) ) ;
#21353 = CARTESIAN_POINT ( 'NONE',  ( -5.563975647486109288, 116.7001730204267460, -0.05417444520887694515 ) ) ;
#21354 = PLANE ( 'NONE',  #38637 ) ;
#21355 = CARTESIAN_POINT ( 'NONE',  ( -0.009931517865296061315, 119.6374844068871397, 0.4970137656763587430 ) ) ;
#21356 = DIRECTION ( 'NONE',  ( -0.9469626219732538708, -0.3213437296502617002, -2.048706518008236507E-16 ) ) ;
#21357 = CARTESIAN_POINT ( 'NONE',  ( 9.796729639280824742, 120.9522862504114897, -1.196371290339073079 ) ) ;
#21358 = CARTESIAN_POINT ( 'NONE',  ( -19.95554629013501469, 150.7967616730061593, -2.267143661507363017 ) ) ;
#21359 = CARTESIAN_POINT ( 'NONE',  ( -54.12303657725384198, 9.464413707472848714, -3.807237671326768602 ) ) ;
#21360 = CARTESIAN_POINT ( 'NONE',  ( 0.01341678693497577735, 156.4123495908283985, -0.6714308817992609146 ) ) ;
#21361 = ORIENTED_EDGE ( 'NONE', *, *, #34966, .F. ) ;
#21362 = CARTESIAN_POINT ( 'NONE',  ( -4.244755607818407661, 119.7015364213435333, -0.9259100998607278088 ) ) ;
#21363 = CARTESIAN_POINT ( 'NONE',  ( 4.529877808639974468, -15.43662617131508163, 0.9000745948097405025 ) ) ;
#21364 = CIRCLE ( 'NONE', #27440, 0.3810000000000015041 ) ;
#21365 = CARTESIAN_POINT ( 'NONE',  ( -4.458822442788735074, 118.1301844220468240, -0.7147248541670323529 ) ) ;
#21366 = CARTESIAN_POINT ( 'NONE',  ( -58.23017998949752183, 0.6774554162835566551, -1.209604144815722426 ) ) ;
#21367 = CARTESIAN_POINT ( 'NONE',  ( -4.838325046627658388, 117.5445662390599466, 0.9681270212778525508 ) ) ;
#21368 = CARTESIAN_POINT ( 'NONE',  ( 17.88897823598637160, 147.4621342421176848, 2.293131556269223381 ) ) ;
#21369 = CARTESIAN_POINT ( 'NONE',  ( -17.08598887363762131, 83.79821757228496892, 1.269999999999997131 ) ) ;
#21370 = EDGE_CURVE ( 'NONE', #16441, #31622, #24412, .T. ) ;
#21371 = CARTESIAN_POINT ( 'NONE',  ( -8.418590987418564708, -6.603242653765095227, 0.8142584484527041200 ) ) ;
#21372 = CARTESIAN_POINT ( 'NONE',  ( 8.994301780669024637, 123.6974368934138226, 0.4925676131310584571 ) ) ;
#21373 = DIRECTION ( 'NONE',  ( -1.000000000000000000, 0.000000000000000000, 0.000000000000000000 ) ) ;
#21375 = VERTEX_POINT ( 'NONE', #25501 ) ;
#21374 = CARTESIAN_POINT ( 'NONE',  ( -41.87797633265722652, 22.30863410810708558, -1.617563149257741140 ) ) ;
#21376 = CARTESIAN_POINT ( 'NONE',  ( -1.621065714518569623, 117.9394518546463075, 1.312504281541743367 ) ) ;
#21377 = CARTESIAN_POINT ( 'NONE',  ( 1.565376701539133553, 118.7629491485454025, 1.245871636779464886 ) ) ;
#21378 = CARTESIAN_POINT ( 'NONE',  ( -57.89731077922513691, 0.5615449381113218896, -1.013091259465030497E-14 ) ) ;
#21379 = CARTESIAN_POINT ( 'NONE',  ( -51.68405183839315242, 20.46365084185837446, 0.3671080129528856428 ) ) ;
#21380 = EDGE_CURVE ( 'NONE', #28325, #28199, #12737, .T. ) ;
#21381 = CARTESIAN_POINT ( 'NONE',  ( -15.16801640535331153, 156.1230782244120121, -0.1031879763837424829 ) ) ;
#21382 = VERTEX_POINT ( 'NONE', #32523 ) ;
#21383 = CARTESIAN_POINT ( 'NONE',  ( -49.54051387650593341, 20.87470723125096228, -2.270501476849551725 ) ) ;
#21384 = CARTESIAN_POINT ( 'NONE',  ( 6.895111204100116353, 121.6823721895668058, -0.3746929160640417034 ) ) ;
#21385 = CARTESIAN_POINT ( 'NONE',  ( -8.614520148391088483, 118.6763556054875863, 0.8198081090888234002 ) ) ;
#21386 = ORIENTED_EDGE ( 'NONE', *, *, #15412, .F. ) ;
#21387 = CARTESIAN_POINT ( 'NONE',  ( 0.08719654901811217662, 115.7029491485439507, -1.760460446363953047 ) ) ;
#21388 = CARTESIAN_POINT ( 'NONE',  ( -8.617107517140190964, 123.3364012560002578, -0.3915851211929421982 ) ) ;
#21389 = CARTESIAN_POINT ( 'NONE',  ( 4.239944546232853106, -14.55591092887127758, 4.867068800921800609 ) ) ;
#21390 = CARTESIAN_POINT ( 'NONE',  ( -4.918710253155017753, 117.7409041207840090, 0.6764595669667289313 ) ) ;
#21391 = DIRECTION ( 'NONE',  ( -0.1565721916418034709, -0.9876665170007954409, 8.659954811667512579E-17 ) ) ;
#21392 = CARTESIAN_POINT ( 'NONE',  ( 21.54627550604352493, 132.6250929350426020, 0.6335863061179136668 ) ) ;
#21393 = CARTESIAN_POINT ( 'NONE',  ( 2.845126842128428812, 121.0294355418728998, 0.09108657199543482297 ) ) ;
#21394 = CARTESIAN_POINT ( 'NONE',  ( -5.036492167631829275, 117.3993844946803478, 0.5480994846027128498 ) ) ;
#21395 = CARTESIAN_POINT ( 'NONE',  ( -0.3664848240473963514, 30.73350494673895739, -0.9073219246443798847 ) ) ;
#21396 = CARTESIAN_POINT ( 'NONE',  ( -15.65298122355244637, 120.8241032224722176, -0.4173319239378794898 ) ) ;
#21397 = CARTESIAN_POINT ( 'NONE',  ( -41.23752580366542020, 23.26788267949596190, -1.523999999999987587 ) ) ;
#21398 = LINE ( 'NONE', #28658, #23101 ) ;
#21399 = ORIENTED_EDGE ( 'NONE', *, *, #15940, .F. ) ;
#21400 = CARTESIAN_POINT ( 'NONE',  ( 6.192180060147616238, 119.1566478384643375, 1.251899301844930035 ) ) ;
#21401 = CARTESIAN_POINT ( 'NONE',  ( -5.332935397695336199, 105.1224662015457199, -0.1065647409268299373 ) ) ;
#21402 = CARTESIAN_POINT ( 'NONE',  ( 21.42793111275534201, 141.8478887571778273, 2.143904907781018387 ) ) ;
#21403 = CARTESIAN_POINT ( 'NONE',  ( -50.47813777547885650, 15.38220854283423122, -4.696510882186583302 ) ) ;
#21404 = CARTESIAN_POINT ( 'NONE',  ( 4.766456943369734134, 158.1906701298835856, -1.576320697809042715 ) ) ;
#21405 = CARTESIAN_POINT ( 'NONE',  ( -0.09930934064637705894, -13.04092083763876175, -4.623607705436294957 ) ) ;
#21406 = CARTESIAN_POINT ( 'NONE',  ( -19.72970310060717480, 132.0165317526581816, -1.843001364771305717 ) ) ;
#21407 = CARTESIAN_POINT ( 'NONE',  ( 4.907479179103392930, 117.6706796365961054, -0.8186149998474543388 ) ) ;
#21408 = ADVANCED_BREP_SHAPE_REPRESENTATION ( '', ( #38952, #3275 ), #40037 ) ;
#21409 = CARTESIAN_POINT ( 'NONE',  ( 2.923657115617320112, 107.8178375082508609, 4.476818208047827596 ) ) ;
#21410 = EDGE_CURVE ( 'NONE', #36274, #7253, #16103, .T. ) ;
#21411 = ORIENTED_EDGE ( 'NONE', *, *, #33934, .T. ) ;
#21412 = CARTESIAN_POINT ( 'NONE',  ( -15.66469409602200891, 147.2250547476223801, -0.08357164438766989667 ) ) ;
#21413 = CARTESIAN_POINT ( 'NONE',  ( -14.20181026158660309, 125.7140216354555804, -2.028863013303968899 ) ) ;
#21414 = EDGE_CURVE ( 'NONE', #5996, #18324, #38921, .T. ) ;
#21415 = CARTESIAN_POINT ( 'NONE',  ( 3.829091000068871598, -15.41100336169511031, 5.152250049158875633 ) ) ;
#21416 = DIRECTION ( 'NONE',  ( 0.1715592850456333085, -0.1224830539174543292, -0.9775302108976914317 ) ) ;
#21417 = EDGE_CURVE ( 'NONE', #41007, #3899, #35305, .T. ) ;
#21418 = CARTESIAN_POINT ( 'NONE',  ( -0.5318626099109079464, 118.1651004811886594, -0.8919322041951796010 ) ) ;
#21419 = ORIENTED_EDGE ( 'NONE', *, *, #36060, .T. ) ;
#21420 = CARTESIAN_POINT ( 'NONE',  ( 8.179471065859045709, 156.5149677146980309, 2.065073912022258984 ) ) ;
#21421 = DIRECTION ( 'NONE',  ( -4.017660918040594346E-17, 1.000000000000000000, 2.376309959284834438E-19 ) ) ;
#21422 = CARTESIAN_POINT ( 'NONE',  ( -4.761160981199589415, 118.7629491485453599, -0.9360238318275121427 ) ) ;
#21423 = CARTESIAN_POINT ( 'NONE',  ( -2.822804308802561835, 121.9077826007922312, 0.1826741318641921241 ) ) ;
#21424 = CARTESIAN_POINT ( 'NONE',  ( 6.742867120194277142, -6.769607736128188336, 5.057590804256700601 ) ) ;
#21425 = CARTESIAN_POINT ( 'NONE',  ( 16.29504633872591768, 146.4745453488731357, 1.441742819671184783 ) ) ;
#21426 = CARTESIAN_POINT ( 'NONE',  ( -4.787809760100155465, 118.5930653697794384, -0.9398806957526995021 ) ) ;
#21427 = CARTESIAN_POINT ( 'NONE',  ( 22.26937170471349603, 150.7043692363948537, -0.4001190995498105640 ) ) ;
#21428 = B_SPLINE_CURVE_WITH_KNOTS ( 'NONE', 3,
 ( #15773, #22356, #41790, #22777, #12588, #28974, #12790, #35808, #6623, #3433 ),
 .UNSPECIFIED., .F., .F.,
 ( 4, 2, 2, 2, 4 ),
 ( 0.000000000000000000, 0.0001574456952392459016, 0.0003148913904784918032, 0.0004723370857177376777, 0.0006297827809569836064 ),
 .UNSPECIFIED. ) ;
#21429 = DIRECTION ( 'NONE',  ( -0.8745520943968256855, 0.4849315768086519540, -5.691349986800502519E-16 ) ) ;
#21430 = CARTESIAN_POINT ( 'NONE',  ( -58.35670767547218674, -0.2641613275777771053, 0.1431915459989163142 ) ) ;
#21431 = CARTESIAN_POINT ( 'NONE',  ( -31.58045816419041074, 52.93464387131874815, -1.524000000000004684 ) ) ;
#21432 = CARTESIAN_POINT ( 'NONE',  ( -43.82859865241511699, 24.63416949198730421, 1.523999999999992916 ) ) ;
#21433 = CARTESIAN_POINT ( 'NONE',  ( -4.308292265359691342, 118.2138082877722240, 0.3344837457086672350 ) ) ;
#21434 = CARTESIAN_POINT ( 'NONE',  ( -1.794468298957929475, 116.4672891243423578, -0.03585774721038182539 ) ) ;
#21435 = ORIENTED_EDGE ( 'NONE', *, *, #32887, .T. ) ;
#21436 = CARTESIAN_POINT ( 'NONE',  ( -48.04822308881583126, 19.89521662531995005, 5.294633059834397137 ) ) ;
#21437 = CARTESIAN_POINT ( 'NONE',  ( 8.304983337102498808, 120.2147944736314713, -1.116985254693862784 ) ) ;
#21438 = DIRECTION ( 'NONE',  ( 5.206863593109713661E-17, -1.000000000000000000, 1.077750396879097183E-30 ) ) ;
#21439 = CARTESIAN_POINT ( 'NONE',  ( 4.342787850355605883, 118.1821923640319625, 0.6217834867231702978 ) ) ;
#21440 = CARTESIAN_POINT ( 'NONE',  ( -15.99655225346421972, 147.0154580547469152, -1.170958206671063762 ) ) ;
#21441 = CARTESIAN_POINT ( 'NONE',  ( 1.589478822742971486E-15, 16.51000000000000156, 0.000000000000000000 ) ) ;
#21442 = CARTESIAN_POINT ( 'NONE',  ( 4.713631738767327661, 116.7564862437112794, 0.09418957996065571714 ) ) ;
#21443 = ORIENTED_EDGE ( 'NONE', *, *, #31856, .T. ) ;
#21444 = CARTESIAN_POINT ( 'NONE',  ( -3.957843245660688680, 22.95775517496322848, 2.395914033147342970 ) ) ;
#21445 = DIRECTION ( 'NONE',  ( 5.188838149069472160E-16, -1.699382548006136559E-16, -1.000000000000000000 ) ) ;
#21446 = CARTESIAN_POINT ( 'NONE',  ( 5.177913976931196594, 78.94499979771845233, -5.372100000000001430 ) ) ;
#21447 = EDGE_CURVE ( 'NONE', #3703, #36577, #5117, .T. ) ;
#21448 = CARTESIAN_POINT ( 'NONE',  ( 5.078986093043054595, 68.92746620154572668, 0.1014902294541237815 ) ) ;
#21449 = CARTESIAN_POINT ( 'NONE',  ( -7.806212186347956106, 122.5473094838618522, 0.09301756479190019522 ) ) ;
#21450 = DIRECTION ( 'NONE',  ( 0.6294287539884133587, 0.7770581983690755257, 0.000000000000000000 ) ) ;
#21451 = CARTESIAN_POINT ( 'NONE',  ( 21.82912119472381107, 136.8312970274703844, 1.482621438090450328 ) ) ;
#21452 = CARTESIAN_POINT ( 'NONE',  ( -2.763989507385018918, 104.6144662015456817, -3.966747042067132245 ) ) ;
#21454 = CARTESIAN_POINT ( 'NONE',  ( 9.525696296010659481, 157.4068808874136209, -1.471446521238429117 ) ) ;
#21453 = CARTESIAN_POINT ( 'NONE',  ( 2.755344442395651683, -14.11966664619605716, -0.1083093155031689958 ) ) ;
#21455 = CARTESIAN_POINT ( 'NONE',  ( -3.942276470047367809, 157.0187206368471209, 1.592783893122187378 ) ) ;
#21456 = CARTESIAN_POINT ( 'NONE',  ( -4.488006035213030209, 18.49445617864287073, 1.146732334616328286 ) ) ;
#21457 = CARTESIAN_POINT ( 'NONE',  ( -15.72348727998161877, 121.4292885696920621, -0.9291061361373527117 ) ) ;
#21458 = CARTESIAN_POINT ( 'NONE',  ( -0.7860673829865619799, 16.32342451650498916, -0.5763570944834206511 ) ) ;
#21459 = ORIENTED_EDGE ( 'NONE', *, *, #33247, .F. ) ;
#21460 = CARTESIAN_POINT ( 'NONE',  ( -56.90063064090522715, 2.680628813859151194, 1.231466298089183953 ) ) ;
#21461 = CIRCLE ( 'NONE', #18734, 0.6350000000000014522 ) ;
#21462 = CARTESIAN_POINT ( 'NONE',  ( -6.226794683659868213, 155.3658059236344684, 0.5518929715360438859 ) ) ;
#21463 = CARTESIAN_POINT ( 'NONE',  ( 4.651167782940357931, -13.82644354294225408, 4.017274338905189701 ) ) ;
#21464 = CARTESIAN_POINT ( 'NONE',  ( 5.207149668175573787, 156.3268443366877989, -1.412139582428342033 ) ) ;
#21465 = ORIENTED_EDGE ( 'NONE', *, *, #877, .T. ) ;
#21466 = CARTESIAN_POINT ( 'NONE',  ( 2.487003399377340163, 115.7030328857400150, 1.696587098641219926 ) ) ;
#21467 = EDGE_CURVE ( 'NONE', #34241, #26546, #7809, .T. ) ;
#21468 = VERTEX_POINT ( 'NONE', #14378 ) ;
#21469 = CARTESIAN_POINT ( 'NONE',  ( 3.171691571413298050, -13.57474810710837509, 1.775319381694977716 ) ) ;
#21470 = CARTESIAN_POINT ( 'NONE',  ( -4.670922868269323125, 117.8935129453105759, -0.9879990057292081795 ) ) ;
#21471 = CARTESIAN_POINT ( 'NONE',  ( 5.940729632618738876, 121.5467800236367424, 0.09028238529180381000 ) ) ;
#21472 = ORIENTED_EDGE ( 'NONE', *, *, #27686, .F. ) ;
#21473 = CARTESIAN_POINT ( 'NONE',  ( 4.596153127770110203, 158.0471523224993859, 1.806220157282541372 ) ) ;
#21474 = CARTESIAN_POINT ( 'NONE',  ( -26.42106975583004314, 72.48669692073261217, -1.524000000000005794 ) ) ;
#21475 = DIRECTION ( 'NONE',  ( 5.188838149069472160E-16, -1.699382548006136559E-16, -1.000000000000000000 ) ) ;
#21476 = CARTESIAN_POINT ( 'NONE',  ( 0.03066982525775523508, 157.3074135339440147, -1.534843470138540278 ) ) ;
#21477 = CARTESIAN_POINT ( 'NONE',  ( 2.803048170062486300, 116.6385632091030544, -0.1397181956995449670 ) ) ;
#21478 = CARTESIAN_POINT ( 'NONE',  ( -46.60530155212503445, 26.17382724835477958, -1.524000000000008459 ) ) ;
#21479 = CARTESIAN_POINT ( 'NONE',  ( 1.713575183690340786, -15.32738180877292500, 5.454580614592902776 ) ) ;
#21480 = CARTESIAN_POINT ( 'NONE',  ( -6.589702033682734540E-14, 87.97746620154572383, -4.338478393988997516E-18 ) ) ;
#21481 = CARTESIAN_POINT ( 'NONE',  ( -11.73534362491072258, 82.73994711668952107, 1.269999999999998241 ) ) ;
#21482 = AXIS2_PLACEMENT_3D ( 'NONE', #25510, #15699, #15497 ) ;
#21483 = CARTESIAN_POINT ( 'NONE',  ( -4.645946495889221595, 117.9566612795834999, 0.7540674584965481042 ) ) ;
#21484 = VECTOR ( 'NONE', #42072, 1000.000000000000000 ) ;
#21485 = EDGE_LOOP ( 'NONE', ( #41310, #788, #32521, #1641, #10773, #5660, #28093, #6676, #25193 ) ) ;
#21486 = ORIENTED_EDGE ( 'NONE', *, *, #7115, .F. ) ;
#21487 = CARTESIAN_POINT ( 'NONE',  ( -0.5121017581959355081, 118.7629491485454025, 1.259106457356409470 ) ) ;
#21488 = VECTOR ( 'NONE', #19816, 1000.000000000000000 ) ;
#21489 = CARTESIAN_POINT ( 'NONE',  ( -5.628064490234534922, 118.3591030996166751, -1.176039089841854235 ) ) ;
#21490 = CARTESIAN_POINT ( 'NONE',  ( -1.876195077988602078, 107.8038693663528278, -4.521701016168464093 ) ) ;
#21491 = CARTESIAN_POINT ( 'NONE',  ( 4.781282322697058440, 117.4742075776832309, 1.189488429716421658 ) ) ;
#21492 = LINE ( 'NONE', #17680, #18090 ) ;
#21493 = CARTESIAN_POINT ( 'NONE',  ( -0.7818436192038892285, 120.2878791493615296, 0.5419007644741468122 ) ) ;
#21494 = DIRECTION ( 'NONE',  ( -5.188838149069471174E-16, 1.699382548006136313E-16, 1.000000000000000000 ) ) ;
#21495 = CARTESIAN_POINT ( 'NONE',  ( -58.83227707057483968, -0.08366279997992775996, 0.2458995907044888019 ) ) ;
#21496 = DIRECTION ( 'NONE',  ( -0.9998004120163610509, -4.016384292689131511E-17, -0.01997839162482749689 ) ) ;
#21497 = CARTESIAN_POINT ( 'NONE',  ( 2.740927916200229131, -14.67636064986481337, 4.771625012207401539 ) ) ;
#21498 = CARTESIAN_POINT ( 'NONE',  ( 6.089625701343383213, 119.5347744825833871, -0.2725575997743531209 ) ) ;
#21499 = CARTESIAN_POINT ( 'NONE',  ( 7.784012320790350437, 122.6313477007501689, 0.1555430920740328848 ) ) ;
#21500 = CARTESIAN_POINT ( 'NONE',  ( -6.335520854202698615, 28.81365682905730097, 0.1643347731004514700 ) ) ;
#21501 = CARTESIAN_POINT ( 'NONE',  ( -0.9196057312421086483, 115.7029491485453718, 1.717296384394745079 ) ) ;
#21502 = CARTESIAN_POINT ( 'NONE',  ( 2.229080734463354307, 9.364070591990056869, -4.050418370856919914 ) ) ;
#21504 = EDGE_LOOP ( 'NONE', ( #17579, #19595, #9980, #11019 ) ) ;
#21503 = CARTESIAN_POINT ( 'NONE',  ( 15.60595500976382333, 121.0226940419799462, 0.7351363234501834265 ) ) ;
#21505 = CARTESIAN_POINT ( 'NONE',  ( 2.600103240316629538, 104.6144662015457243, -4.075503436606891405 ) ) ;
#21506 = CARTESIAN_POINT ( 'NONE',  ( 3.404406166340397277, -15.64019586361782643, 4.053891870528842922 ) ) ;
#21507 = CARTESIAN_POINT ( 'NONE',  ( -2.527692779614401086, 158.0185616612000956, 1.624164342510255210 ) ) ;
#21508 = CARTESIAN_POINT ( 'NONE',  ( -0.7014129483091587902, 16.11884676413550466, -0.6771123631929140130 ) ) ;
#21509 = CARTESIAN_POINT ( 'NONE',  ( -0.9370761106581132482, 23.39645565634240043, 0.2812775048015344614 ) ) ;
#21510 = ORIENTED_EDGE ( 'NONE', *, *, #5258, .T. ) ;
#21511 = VERTEX_POINT ( 'NONE', #34001 ) ;
#21512 = DIRECTION ( 'NONE',  ( 0.8745520943968249084, -0.4849315768086533418, 5.311926654347176508E-16 ) ) ;
#21513 = CARTESIAN_POINT ( 'NONE',  ( 1.155499320159395937, 111.9985432423065959, 2.960082065640199822 ) ) ;
#21514 =( NAMED_UNIT ( * ) SI_UNIT ( $, .STERADIAN. ) SOLID_ANGLE_UNIT ( ) );
#21515 = CARTESIAN_POINT ( 'NONE',  ( -4.803469898345708700, 156.0326374431741385, 1.047298710704739344 ) ) ;
#21516 = FACE_OUTER_BOUND ( 'NONE', #29797, .T. ) ;
#21517 = EDGE_CURVE ( 'NONE', #12283, #11359, #13550, .T. ) ;
#21518 = CARTESIAN_POINT ( 'NONE',  ( 3.214659515886821861, -12.19625089790456229, 0.4983212145216010525 ) ) ;
#21519 = CARTESIAN_POINT ( 'NONE',  ( 17.58824906652080600, 148.8653046532945723, -1.619734885946522596 ) ) ;
#21520 = CARTESIAN_POINT ( 'NONE',  ( -3.174067013697543072, 118.4902560533893592, -0.8904294910640481175 ) ) ;
#21521 = DIRECTION ( 'NONE',  ( 0.6559537821943282054, -0.7548010569845248208, 8.537024980200704475E-16 ) ) ;
#21522 = EDGE_CURVE ( 'NONE', #6398, #27753, #1421, .T. ) ;
#21523 = CARTESIAN_POINT ( 'NONE',  ( 4.074910602682932925, 118.2429491485453354, -0.1454311599470142491 ) ) ;
#21524 = CARTESIAN_POINT ( 'NONE',  ( 9.391698128491960063, 124.2036136473707018, -0.1363215471561607384 ) ) ;
#21525 = AXIS2_PLACEMENT_3D ( 'NONE', #29320, #25908, #19508 ) ;
#21526 = ORIENTED_EDGE ( 'NONE', *, *, #14406, .F. ) ;
#21527 = CARTESIAN_POINT ( 'NONE',  ( 2.768784035434307178, -15.00486597294339930, 4.394545281259884639 ) ) ;
#21528 = CARTESIAN_POINT ( 'NONE',  ( -6.578476689077728991E-14, 85.18346620154574111, -5.002419396613184919E-18 ) ) ;
#21529 = CARTESIAN_POINT ( 'NONE',  ( -57.74919803515417271, 1.101601998901911683, 1.404840701338397002 ) ) ;
#21530 = CARTESIAN_POINT ( 'NONE',  ( 3.857898856315107761, -6.768822978661375167, 2.551181839177400601 ) ) ;
#21531 = CARTESIAN_POINT ( 'NONE',  ( 5.849275934571454449, 120.8872308857076519, 0.8185814695607154245 ) ) ;
#21532 = CARTESIAN_POINT ( 'NONE',  ( -2.900060555911446070, 29.50094634256690540, 2.476086984555808002 ) ) ;
#21533 = CARTESIAN_POINT ( 'NONE',  ( -5.086085965935806641, 114.3657942991566472, 1.756424186875608751 ) ) ;
#21534 = VECTOR ( 'NONE', #2395, 1000.000000000000000 ) ;
#21535 = AXIS2_PLACEMENT_3D ( 'NONE', #38194, #11557, #31155 ) ;
#21536 = CARTESIAN_POINT ( 'NONE',  ( -2.406711483539481389, 4.503775517365914638, 3.979180414515509412 ) ) ;
#21537 = CARTESIAN_POINT ( 'NONE',  ( 0.6438746309740379647, 120.9974662015465867, 0.01286614746332127857 ) ) ;
#21538 = CARTESIAN_POINT ( 'NONE',  ( 0.6424836204703546771, -8.070646579680392563, 8.395564330620057802 ) ) ;
#21539 = CARTESIAN_POINT ( 'NONE',  ( -57.84361080044246251, 0.8513586351276830611, -1.093731309501911886 ) ) ;
#21540 = CARTESIAN_POINT ( 'NONE',  ( -8.754227852576507374, 117.8550674546482071, -0.6168156700147224836 ) ) ;
#21541 = CIRCLE ( 'NONE', #30410, 5.080000000000006288 ) ;
#21542 = CARTESIAN_POINT ( 'NONE',  ( -0.1664298668079876309, 110.3683645023726427, -3.586750284817682211 ) ) ;
#21543 = DIRECTION ( 'NONE',  ( 0.8745520943968472238, -0.4849315768086133738, 2.585085348184235087E-15 ) ) ;
#21544 = CARTESIAN_POINT ( 'NONE',  ( 4.537321141924904211, 26.63107350737006840, 0.8823464973398146283 ) ) ;
#21545 = CARTESIAN_POINT ( 'NONE',  ( 0.6963533560661814281, 117.3993842961302363, 1.488888644047975607 ) ) ;
#21546 = CARTESIAN_POINT ( 'NONE',  ( -6.538176131568015962E-14, 82.13546620154573930, -1.207165459078370276E-19 ) ) ;
#21547 = CARTESIAN_POINT ( 'NONE',  ( 15.15189561879764746, 77.97492127061565270, -1.904999999999999583 ) ) ;
#21548 = CARTESIAN_POINT ( 'NONE',  ( 0.3790891741044132290, 120.5507043431651510, -0.5490176968301535565 ) ) ;
#21549 = CARTESIAN_POINT ( 'NONE',  ( -21.14621813959900010, 132.3956117394162106, 0.2431941713936564553 ) ) ;
#21550 = VECTOR ( 'NONE', #6030, 1000.000000000000000 ) ;
#21551 = ORIENTED_EDGE ( 'NONE', *, *, #15701, .F. ) ;
#21552 = CARTESIAN_POINT ( 'NONE',  ( -58.77954282417582732, 0.05649391281087323691, -0.1080441935232595435 ) ) ;
#21553 = ORIENTED_EDGE ( 'NONE', *, *, #25593, .F. ) ;
#21554 = CARTESIAN_POINT ( 'NONE',  ( -14.73199999999999932, 12.96416000000000146, 0.000000000000000000 ) ) ;
#21555 = CARTESIAN_POINT ( 'NONE',  ( -5.945776936743828678, 121.5465042053001667, -0.1188107733588233128 ) ) ;
#21556 = CARTESIAN_POINT ( 'NONE',  ( 4.355571528211143573, -15.30747929803376373, 4.711715777764150737 ) ) ;
#21557 = CARTESIAN_POINT ( 'NONE',  ( -15.93384955644688183, 125.3951846505478329, 1.286024093939968305 ) ) ;
#21558 = CARTESIAN_POINT ( 'NONE',  ( 22.39452804842985500, 149.5981344557702641, -0.8550856607202135251 ) ) ;
#21559 = CARTESIAN_POINT ( 'NONE',  ( -4.631227783250409402, 22.10816835407601744, -0.05711764529929251599 ) ) ;
#21560 = CARTESIAN_POINT ( 'NONE',  ( -4.777924661806649986, 116.8922783744782379, -0.3800144224740276133 ) ) ;
#21561 = CARTESIAN_POINT ( 'NONE',  ( -51.88968468915965104, 13.12277401453617820, -4.448989927898648666 ) ) ;
#21562 = EDGE_LOOP ( 'NONE', ( #29488, #33708, #39054, #14328 ) ) ;
#21563 = CARTESIAN_POINT ( 'NONE',  ( 8.795381777531829925, 117.6899729038807720, 0.2515276502602432074 ) ) ;
#21564 = DIRECTION ( 'NONE',  ( -5.188838149069471174E-16, 1.699382548006136313E-16, 1.000000000000000000 ) ) ;
#21565 = CARTESIAN_POINT ( 'NONE',  ( -5.108784305046479624, 120.0747842884402132, 0.7604166522187121302 ) ) ;
#21566 = CARTESIAN_POINT ( 'NONE',  ( -53.67394638921515337, 9.465966177595170450, -3.594732514767734255 ) ) ;
#21567 = CARTESIAN_POINT ( 'NONE',  ( 16.46135582144558285, 131.4813445454897192, -1.641276044305394866 ) ) ;
#21568 = CARTESIAN_POINT ( 'NONE',  ( -4.008523173341965951, 118.0179939250997023, -0.8984863180294770935 ) ) ;
#21569 = CARTESIAN_POINT ( 'NONE',  ( -54.47970570282438274, 8.083255770631444292, -3.476097746275910172 ) ) ;
#21570 = STYLED_ITEM ( 'NONE', ( #16656 ), #22381 ) ;
#21571 = ADVANCED_FACE ( 'NONE', ( #27388 ), #30582, .F. ) ;
#21572 = CARTESIAN_POINT ( 'NONE',  ( 8.258026456251805314, 154.6505398758502849, -0.7900859392159012007 ) ) ;
#21573 = ORIENTED_EDGE ( 'NONE', *, *, #4113, .F. ) ;
#21574 = CARTESIAN_POINT ( 'NONE',  ( -10.13131171838204203, 122.2967958330617648, -1.512676856611740561 ) ) ;
#21575 = CARTESIAN_POINT ( 'NONE',  ( 3.762885361805711870, -15.68952731832974656, 3.843115198823321865 ) ) ;
#21576 = CARTESIAN_POINT ( 'NONE',  ( -4.112774970794720986, 118.2429491485453070, -0.3453283136715148416 ) ) ;
#21577 = CARTESIAN_POINT ( 'NONE',  ( -58.55221842960730783, 0.5754175076986972615, -0.9757793345693789311 ) ) ;
#21578 = DIRECTION ( 'NONE',  ( -5.188838149069472160E-16, 1.699382548006136559E-16, 1.000000000000000000 ) ) ;
#21579 = CARTESIAN_POINT ( 'NONE',  ( 17.92322948971676766, 147.1528319293316542, 2.295422193410857847 ) ) ;
#21580 = CARTESIAN_POINT ( 'NONE',  ( -10.18297664959815663, 77.66688486464208552, -1.523999999999998245 ) ) ;
#21581 = CARTESIAN_POINT ( 'NONE',  ( -2.033853377119958061, -8.777475726645231902, -8.175041553700232555 ) ) ;
#21582 = CARTESIAN_POINT ( 'NONE',  ( 0.6270554149910597674, 120.8998192842950488, 0.1385313962210439065 ) ) ;
#21583 = CARTESIAN_POINT ( 'NONE',  ( -58.70413935429054675, 0.2332485698458008905, -0.6626129746612972049 ) ) ;
#21585 = ORIENTED_EDGE ( 'NONE', *, *, #991, .F. ) ;
#21584 = CARTESIAN_POINT ( 'NONE',  ( -41.05189575270517821, 23.09451173561983950, -1.524000000000004462 ) ) ;
#21586 = CARTESIAN_POINT ( 'NONE',  ( 0.1066493941974573784, 105.7853621660184444, -5.332931186019219005 ) ) ;
#21587 = CARTESIAN_POINT ( 'NONE',  ( -7.839438867670176059, 122.3085338874637671, -0.7152514657530811837 ) ) ;
#21588 =( GEOMETRIC_REPRESENTATION_CONTEXT ( 3 ) GLOBAL_UNCERTAINTY_ASSIGNED_CONTEXT ( ( #23544 ) ) GLOBAL_UNIT_ASSIGNED_CONTEXT ( ( #41838, #3065, #35427 ) ) REPRESENTATION_CONTEXT ( 'NONE', 'WORKASPACE' ) );
#21589 = CARTESIAN_POINT ( 'NONE',  ( -5.241362157049148429, 77.01756249999996840, -5.310945289804168468 ) ) ;
#21590 = CARTESIAN_POINT ( 'NONE',  ( -51.08083271936510528, 17.88738476406025057, 2.973263991802279183 ) ) ;
#21591 = CARTESIAN_POINT ( 'NONE',  ( -1.417759636995488570, 159.6040221172770259, 0.05833233067434092506 ) ) ;
#21592 = VERTEX_POINT ( 'NONE', #36370 ) ;
#21593 = CARTESIAN_POINT ( 'NONE',  ( -48.34142060212425207, 20.97662605846759831, -3.847193496378360056 ) ) ;
#21594 = CARTESIAN_POINT ( 'NONE',  ( 7.864380575010578411, 122.2948005240338603, -0.4127209565927187351 ) ) ;
#21595 = ADVANCED_FACE ( 'NONE', ( #1006 ), #13117, .T. ) ;
#21596 = CARTESIAN_POINT ( 'NONE',  ( -7.886551735270039387, 122.1946728851204398, 0.4945421293698979981 ) ) ;
#21597 = VERTEX_POINT ( 'NONE', #26766 ) ;
#21598 = CARTESIAN_POINT ( 'NONE',  ( 4.375075790391449004, 118.7629491485369613, -0.8820669128659245350 ) ) ;
#21599 = CARTESIAN_POINT ( 'NONE',  ( -8.927705404389175925, 123.7033391712731145, -0.4040904458349091621 ) ) ;
#21600 = CARTESIAN_POINT ( 'NONE',  ( 5.886196856236641572, -12.36517754215322995, 0.8550893866892870232 ) ) ;
#21601 = CARTESIAN_POINT ( 'NONE',  ( -21.83857928711807261, 148.7205309135917730, 1.274413580488712450 ) ) ;
#21602 = CARTESIAN_POINT ( 'NONE',  ( -29.91360363449003756, 70.04874496952835727, 1.269999999999992468 ) ) ;
#21603 = CARTESIAN_POINT ( 'NONE',  ( 22.82515744214346753, 150.4067493646842593, 0.6093393687072348186 ) ) ;
#21604 = CARTESIAN_POINT ( 'NONE',  ( 5.317159844422477910, 121.3518965702581340, 0.1425998613045213748 ) ) ;
#21605 = DIRECTION ( 'NONE',  ( -0.8745520943968243532, 0.4849315768086547296, -5.361993529360573944E-16 ) ) ;
#21606 = CARTESIAN_POINT ( 'NONE',  ( 0.8793282038724897776, 27.06027571872007442, 0.4248793764785103177 ) ) ;
#21607 = CARTESIAN_POINT ( 'NONE',  ( -22.98214253804999530, 150.1595482613961110, -0.5361612621683793378 ) ) ;
#21608 = CARTESIAN_POINT ( 'NONE',  ( -42.67774629359277583, 22.12976331235084970, -1.921043605742120519 ) ) ;
#21609 = ADVANCED_FACE ( 'NONE', ( #33370 ), #33169, .T. ) ;
#21610 = CARTESIAN_POINT ( 'NONE',  ( -5.460472493305379871, 56.51500000000001478, -4.448254263655326390 ) ) ;
#21611 = ORIENTED_EDGE ( 'NONE', *, *, #35816, .F. ) ;
#21612 = CARTESIAN_POINT ( 'NONE',  ( 3.990160187250827217, 118.2607540442166680, 0.9787250380842466013 ) ) ;
#21613 = CARTESIAN_POINT ( 'NONE',  ( -6.513165593194060347E-14, 68.92746620154572668, -8.865348866426607246E-18 ) ) ;
#21614 = CARTESIAN_POINT ( 'NONE',  ( 6.827620370265914396, 118.1252062928739832, 1.028125137227138275 ) ) ;
#21615 = CARTESIAN_POINT ( 'NONE',  ( 16.30903692877109279, 153.4734386769207504, -1.632589361097313230 ) ) ;
#21616 = CARTESIAN_POINT ( 'NONE',  ( -6.181412921142831252, 19.34218365691531361, 5.729511908899769246 ) ) ;
#21617 = CARTESIAN_POINT ( 'NONE',  ( -17.71751426720061318, 153.9999837190418930, -1.728000864493653754 ) ) ;
#21618 = CARTESIAN_POINT ( 'NONE',  ( 4.737242769783595264, 117.7521409222561601, -0.9001186629912181214 ) ) ;
#21619 = ADVANCED_FACE ( 'NONE', ( #20980, #17578 ), #36989, .F. ) ;
#21620 = CARTESIAN_POINT ( 'NONE',  ( 6.094139411021942898, 119.5248422734510427, 0.5163842741021833493 ) ) ;
#21621 = ORIENTED_EDGE ( 'NONE', *, *, #1928, .T. ) ;
#21622 = CARTESIAN_POINT ( 'NONE',  ( -9.234582554329520576, 124.2544328994657405, -0.09881537413615858190 ) ) ;
#21623 = CARTESIAN_POINT ( 'NONE',  ( -11.65353862096132609, 154.7938929448963279, -2.201148936174281534 ) ) ;
#21624 = CARTESIAN_POINT ( 'NONE',  ( 5.208953926857062378, -15.24612122244077561, 3.266433406317167165 ) ) ;
#21625 = DIRECTION ( 'NONE',  ( -0.8745520943968241312, 0.4849315768086548406, -5.691349986800536046E-16 ) ) ;
#21626 = COLOUR_RGB ( '', 0.40784314, 0.44705882, 0.49803922) ;
#21627 = CARTESIAN_POINT ( 'NONE',  ( -11.43668055974971764, 78.14103736854400495, 1.270000000000000018 ) ) ;
#21628 = EDGE_CURVE ( 'NONE', #31017, #39680, #24383, .T. ) ;
#21629 = ORIENTED_EDGE ( 'NONE', *, *, #12063, .T. ) ;
#21630 = CARTESIAN_POINT ( 'NONE',  ( 18.70459055478403343, 148.4604323410545987, 2.472120825861215732 ) ) ;
#21631 = DIRECTION ( 'NONE',  ( -0.6294287539884133587, -0.7770581983690755257, 0.000000000000000000 ) ) ;
#21632 = CARTESIAN_POINT ( 'NONE',  ( -4.812426554072069429, 118.7629491485389650, -0.6571134116375234591 ) ) ;
#21633 = CARTESIAN_POINT ( 'NONE',  ( -0.2204105866772946287, 106.6745790697264056, 5.009819746185714351 ) ) ;
#21634 = CARTESIAN_POINT ( 'NONE',  ( 7.953355231451894269, -5.272462086923463076, -2.798479926915725891 ) ) ;
#21635 = CARTESIAN_POINT ( 'NONE',  ( 9.704918697729759458, 124.0009531390599591, 0.8840593909831664376 ) ) ;
#21636 = CARTESIAN_POINT ( 'NONE',  ( -5.239701418611189432, 115.6909491485453003, -1.023982712389454930 ) ) ;
#21637 = CARTESIAN_POINT ( 'NONE',  ( 8.157450159232084275, 117.7673425867732249, -0.3794901880580578424 ) ) ;
#21638 = EDGE_CURVE ( 'NONE', #32351, #18952, #38027, .T. ) ;
#21639 = CARTESIAN_POINT ( 'NONE',  ( 6.059261036834405978, 56.51500000000000057, -4.381499999999999950 ) ) ;
#21640 = AXIS2_PLACEMENT_3D ( 'NONE', #9412, #6854, #32840 ) ;
#21641 = CARTESIAN_POINT ( 'NONE',  ( -58.30092733718098685, -0.1459886894293531967, 0.3347744076924483725 ) ) ;
#21642 = CARTESIAN_POINT ( 'NONE',  ( -4.499111063581361591, 31.49064988344817806, -0.6933409209711203225 ) ) ;
#21643 = ADVANCED_FACE ( 'NONE', ( #34837 ), #40808, .T. ) ;
#21644 = DIRECTION ( 'NONE',  ( 1.000000000000000000, -1.162840169671635117E-16, 0.000000000000000000 ) ) ;
#21645 = CARTESIAN_POINT ( 'NONE',  ( -4.280837819800595412, 118.2124897020258771, 0.3640674451363055120 ) ) ;
#21646 = CARTESIAN_POINT ( 'NONE',  ( -9.822473411059320370, 117.9943479623217399, -0.1962763949404990327 ) ) ;
#21647 = ORIENTED_EDGE ( 'NONE', *, *, #18057, .F. ) ;
#21648 = CARTESIAN_POINT ( 'NONE',  ( -51.81113891419111894, 13.24950054771400332, 4.495723625053109629 ) ) ;
#21649 = CARTESIAN_POINT ( 'NONE',  ( -8.223115700291321772, 120.3649693293168639, -1.438891654778712281 ) ) ;
#21650 = CARTESIAN_POINT ( 'NONE',  ( 5.329288917532060132, 116.0444662015457453, 0.2890495193807575691 ) ) ;
#21651 = CARTESIAN_POINT ( 'NONE',  ( 0.004916276843087831992, 120.6356583033945782, -0.2460305967400713556 ) ) ;
#21652 = CARTESIAN_POINT ( 'NONE',  ( 4.973935731622961320, 117.4065895991867734, -0.8875407820844548601 ) ) ;
#21653 = CARTESIAN_POINT ( 'NONE',  ( 0.02808993187329204833, 117.9496053154548321, -1.405735122999207887 ) ) ;
#21654 = EDGE_CURVE ( 'NONE', #25, #38897, #8804, .T. ) ;
#21655 = ORIENTED_EDGE ( 'NONE', *, *, #14924, .T. ) ;
#21656 = CARTESIAN_POINT ( 'NONE',  ( -2.614655561276646889, 23.60746518810343986, 3.812863311767609620 ) ) ;
#21657 = CARTESIAN_POINT ( 'NONE',  ( -7.019433301159665461, 78.79326733250417192, 2.552382320839211349 ) ) ;
#21658 = CARTESIAN_POINT ( 'NONE',  ( -41.09670346151854403, 23.04688172093030829, -1.270085369932534958 ) ) ;
#21659 = DIRECTION ( 'NONE',  ( 1.000000000000000000, 0.000000000000000000, -5.975917486140574681E-16 ) ) ;
#21660 = CARTESIAN_POINT ( 'NONE',  ( -48.27156028472870020, 19.62643105735276450, 5.256042649956950363 ) ) ;
#21661 = CARTESIAN_POINT ( 'NONE',  ( -7.793391099074982620, 122.5980884063560836, -0.02750199203433729284 ) ) ;
#21662 = CIRCLE ( 'NONE', #12840, 0.2540000000000012248 ) ;
#21663 = CARTESIAN_POINT ( 'NONE',  ( -0.9239673467531356321, 25.61616486456964736, -4.531977062890359065 ) ) ;
#21664 = CARTESIAN_POINT ( 'NONE',  ( 0.9938236163260620870, 116.9791385580615781, 0.3849800449318574458 ) ) ;
#21665 = CARTESIAN_POINT ( 'NONE',  ( -3.891925687308367632, 104.6144662015454401, -2.872084872932638699 ) ) ;
#21667 = CARTESIAN_POINT ( 'NONE',  ( 14.09802512849270073, 121.9525460547650226, -1.083329899170117461 ) ) ;
#21666 = CARTESIAN_POINT ( 'NONE',  ( 2.908198840139253338, -13.99431844974620454, 0.6722015529863232253 ) ) ;
#21668 = CARTESIAN_POINT ( 'NONE',  ( -5.624295920984248909, 156.7050554705274408, 1.628980406729419350 ) ) ;
#21669 = VECTOR ( 'NONE', #37817, 1000.000000000000227 ) ;
#21670 = CARTESIAN_POINT ( 'NONE',  ( 4.353980591602404360, 23.44215234368072487, -1.583070106892425111 ) ) ;
#21671 = CARTESIAN_POINT ( 'NONE',  ( -13.19686234056499430, 119.7880570645780978, -0.9111371353940662665 ) ) ;
#21672 = CARTESIAN_POINT ( 'NONE',  ( 0.5639076275445228381, 13.94848098472073161, -0.7944722417661187475 ) ) ;
#21673 = ORIENTED_EDGE ( 'NONE', *, *, #31398, .T. ) ;
#21674 = CARTESIAN_POINT ( 'NONE',  ( -55.72901529264892417, 4.991126730481368234, 1.691135755076699665 ) ) ;
#21675 = CARTESIAN_POINT ( 'NONE',  ( -15.59522120955195845, 147.8873989650969918, 0.4103944809294446383 ) ) ;
#21676 = CARTESIAN_POINT ( 'NONE',  ( 3.183750377336629356, -15.03749083096926675, 5.611903928707999256 ) ) ;
#21677 = CARTESIAN_POINT ( 'NONE',  ( 10.11798836042633454, 123.5826510519420509, -0.8100524519737970497 ) ) ;
#21678 = ORIENTED_EDGE ( 'NONE', *, *, #8732, .T. ) ;
#21679 = CARTESIAN_POINT ( 'NONE',  ( 0.5848834147048422860, 115.7029859896981634, 1.760412536671860817 ) ) ;
#21680 = CARTESIAN_POINT ( 'NONE',  ( -4.851553261282356644, 117.6732321342373524, -1.041740536389639482 ) ) ;
#21681 = CARTESIAN_POINT ( 'NONE',  ( 2.829134042005047256, 121.0305217392013759, 0.03030232591675486795 ) ) ;
#21682 = EDGE_LOOP ( 'NONE', ( #19790, #2597, #6505, #39158 ) ) ;
#21683 = CARTESIAN_POINT ( 'NONE',  ( 9.988019213705062072, 120.6268241347409855, 1.591717657363032723 ) ) ;
#21684 = DIRECTION ( 'NONE',  ( 5.188838149069472160E-16, -1.699382548006136559E-16, -1.000000000000000000 ) ) ;
#21685 = CARTESIAN_POINT ( 'NONE',  ( -6.583861033951825950E-14, 91.02546620154572565, 1.480257718193877056E-29 ) ) ;
#21686 = CARTESIAN_POINT ( 'NONE',  ( 0.03153870137009017610, 158.4432089348667319, -1.578325583784927932 ) ) ;
#21687 = ADVANCED_FACE ( 'NONE', ( #2260 ), #12033, .T. ) ;
#21688 = CARTESIAN_POINT ( 'NONE',  ( 22.95349865178509674, 150.1476136049543868, 0.1290964995630298762 ) ) ;
#21689 = VECTOR ( 'NONE', #28116, 1000.000000000000000 ) ;
#21690 = CARTESIAN_POINT ( 'NONE',  ( 6.059261036833980540, 78.87450423423040036, -5.016499999999999737 ) ) ;
#21691 = CARTESIAN_POINT ( 'NONE',  ( 2.073162808081137509, -15.12483991451984977, 5.841363716764139902 ) ) ;
#21692 = FACE_OUTER_BOUND ( 'NONE', #16710, .T. ) ;
#21693 = DIRECTION ( 'NONE',  ( 4.017660918040594346E-17, -1.000000000000000000, -2.376309959284834438E-19 ) ) ;
#21694 = CARTESIAN_POINT ( 'NONE',  ( -4.783754133273223630, 117.8482099188709071, 0.7929052515055885486 ) ) ;
#21695 = ORIENTED_EDGE ( 'NONE', *, *, #5067, .T. ) ;
#21696 = ORIENTED_EDGE ( 'NONE', *, *, #36960, .T. ) ;
#21697 = DIRECTION ( 'NONE',  ( -4.017660918040594346E-17, 1.000000000000000000, 2.376309959284832031E-19 ) ) ;
#21698 = EDGE_CURVE ( 'NONE', #4116, #6518, #5671, .T. ) ;
#21699 = CARTESIAN_POINT ( 'NONE',  ( -5.828253901312384855, 118.9244088370469257, -1.251152115012297728 ) ) ;
#21700 = CARTESIAN_POINT ( 'NONE',  ( -6.983605877934339290, 124.9344662015457175, -0.1395490654994193946 ) ) ;
#21701 = CARTESIAN_POINT ( 'NONE',  ( 4.857949651814833736, 117.7455164169167290, 0.9241763922800549924 ) ) ;
#21702 = DIRECTION ( 'NONE',  ( -1.000000000000000000, 0.000000000000000000, 0.000000000000000000 ) ) ;
#21703 = CARTESIAN_POINT ( 'NONE',  ( -0.08519874065577472122, 108.5751225745497948, 4.263693374914214296 ) ) ;
#21704 = CARTESIAN_POINT ( 'NONE',  ( 0.6989348986720191892, -4.029744825116962303, 4.573446973323917142 ) ) ;
#21705 = ADVANCED_FACE ( 'NONE', ( #12249 ), #39172, .T. ) ;
#21706 = CARTESIAN_POINT ( 'NONE',  ( 4.958342374402591624, 117.4102150217221237, -0.9055978162701078249 ) ) ;
#21707 = DIRECTION ( 'NONE',  ( 1.000000000000000000, -9.627370216492862708E-17, 0.000000000000000000 ) ) ;
#21708 = CARTESIAN_POINT ( 'NONE',  ( 3.494528270914563528, -13.06595970051097133, 2.012497701936279082 ) ) ;
#21709 = CARTESIAN_POINT ( 'NONE',  ( 7.426015305410854417, 123.6670498955208473, 0.1137005639190687006 ) ) ;
#21710 = CARTESIAN_POINT ( 'NONE',  ( -1.409834354326183314, 119.9358631726476574, -0.5453972335014173334 ) ) ;
#21711 = CARTESIAN_POINT ( 'NONE',  ( -6.065589077789664607, 121.4348142148880214, -0.1208730379670850952 ) ) ;
#21712 = CARTESIAN_POINT ( 'NONE',  ( -5.871471797037544071, 31.01275966357848901, 2.875548327037550589 ) ) ;
#21713 = CARTESIAN_POINT ( 'NONE',  ( -0.6339378988202717391, 115.7029520820172905, 1.736981566562831425 ) ) ;
#21714 = CARTESIAN_POINT ( 'NONE',  ( 4.076717266748975277, 8.489475128091552136, -2.202413229635628689 ) ) ;
#21716 = ORIENTED_EDGE ( 'NONE', *, *, #39652, .F. ) ;
#21715 = CARTESIAN_POINT ( 'NONE',  ( 18.42221188220377215, 125.1790410860780298, 0.8413473246917885229 ) ) ;
#21717 = CARTESIAN_POINT ( 'NONE',  ( 4.563830193338946017, 104.6144662015380931, -2.766517067423098553 ) ) ;
#21718 = CARTESIAN_POINT ( 'NONE',  ( 4.512298201359578265, -15.31825885905126228, -0.4677400858729020006 ) ) ;
#21719 = CARTESIAN_POINT ( 'NONE',  ( -2.466025220844247468, 157.8629595415303584, 1.630325060746250720 ) ) ;
#21720 = CARTESIAN_POINT ( 'NONE',  ( 0.7508863055360318617, -11.68651920905074348, 0.6198408032357946018 ) ) ;
#21721 = CARTESIAN_POINT ( 'NONE',  ( -0.6963090749671848600, 14.53960050853193842, 0.6834203841726373962 ) ) ;
#21722 = ORIENTED_EDGE ( 'NONE', *, *, #13329, .T. ) ;
#21723 = AXIS2_PLACEMENT_3D ( 'NONE', #6114, #19077, #32082 ) ;
#21724 = ORIENTED_EDGE ( 'NONE', *, *, #37282, .T. ) ;
#21725 = DIRECTION ( 'NONE',  ( -4.017660918040594346E-17, 1.000000000000000000, 2.376309959284834438E-19 ) ) ;
#21726 = CARTESIAN_POINT ( 'NONE',  ( 2.208446607403821371, 108.4767889311100362, 4.246804138318780453 ) ) ;
#21727 = PRESENTATION_STYLE_ASSIGNMENT (( #15134 ) ) ;
#21728 = CARTESIAN_POINT ( 'NONE',  ( -16.31827467517383923, 146.7930872653447523, 0.7884962901916311440 ) ) ;
#21729 = DIRECTION ( 'NONE',  ( 0.9998004120163609398, 0.000000000000000000, 0.01997839162482749689 ) ) ;
#21730 = AXIS2_PLACEMENT_3D ( 'NONE', #23343, #25713, #3150 ) ;
#21731 = CARTESIAN_POINT ( 'NONE',  ( 2.390819523577490280, -14.89105559343156848, 5.112470274569719919 ) ) ;
#21732 = CARTESIAN_POINT ( 'NONE',  ( 12.98417868877897163, 125.9520529675768898, -1.303718779035868192 ) ) ;
#21733 = CARTESIAN_POINT ( 'NONE',  ( -7.694773992301706222, 119.4405053107883958, -1.366649582720010025 ) ) ;
#21734 = CARTESIAN_POINT ( 'NONE',  ( -18.32410244842765934, 8.844871939465427602, 0.000000000000000000 ) ) ;
#21735 = CARTESIAN_POINT ( 'NONE',  ( -15.78437780952707215, 146.2378312303354448, -0.3154094333657934679 ) ) ;
#21736 = CARTESIAN_POINT ( 'NONE',  ( -6.536164027931061327, 29.86201144190116707, 0.1241447379370549109 ) ) ;
#21737 = CARTESIAN_POINT ( 'NONE',  ( 5.244198393876475350, 121.2166884500396833, -0.1799464770355447274 ) ) ;
#21738 = EDGE_LOOP ( 'NONE', ( #21931, #14822, #40893, #13084 ) ) ;
#21739 = CARTESIAN_POINT ( 'NONE',  ( 2.350639260211558668, -15.10312717587823705, 4.966175652281853203 ) ) ;
#21740 = DIRECTION ( 'NONE',  ( -0.9998004120163608288, 0.000000000000000000, -0.01997839162482749342 ) ) ;
#21741 = CARTESIAN_POINT ( 'NONE',  ( 4.855108373332432947, 117.7629957853780667, 0.8790759234368952235 ) ) ;
#21742 = CARTESIAN_POINT ( 'NONE',  ( -56.80696390458998479, 3.604343092604281207, 2.316781442554533665 ) ) ;
#21743 = CARTESIAN_POINT ( 'NONE',  ( -0.6580430243309095539, -8.493043821084315326, 4.585212396833119541 ) ) ;
#21744 = CARTESIAN_POINT ( 'NONE',  ( 6.788801044988693967, 155.5980657034081105, 1.487835262196284036 ) ) ;
#21745 = CYLINDRICAL_SURFACE ( 'NONE', #4289, 0.5080000000000000071 ) ;
#21746 = CARTESIAN_POINT ( 'NONE',  ( -0.3628555246835991066, 105.8844662015457629, 5.327769491516690437 ) ) ;
#21747 = CARTESIAN_POINT ( 'NONE',  ( -4.187759052228169132, -5.978784877027076838, 2.003160513425938483 ) ) ;
#21748 = CARTESIAN_POINT ( 'NONE',  ( -7.220045317357707698E-14, 120.9974662015457341, -1.901466176754077691E-16 ) ) ;
#21749 = CARTESIAN_POINT ( 'NONE',  ( 6.390864997528122871, 2.724353428444007630, 5.482255947279437436 ) ) ;
#21750 = CARTESIAN_POINT ( 'NONE',  ( -57.60038635073813396, 1.097546858218847898, -0.08229580080366473427 ) ) ;
#21751 = CARTESIAN_POINT ( 'NONE',  ( -5.498207759818521723, 117.0463165232320364, -0.7052634562340454050 ) ) ;
#21752 = CARTESIAN_POINT ( 'NONE',  ( -0.3633380039126155592, 121.5961256765096152, -0.3912981906941392363 ) ) ;
#21753 = DIRECTION ( 'NONE',  ( -0.7308269722843147020, 0.6825627711659504326, -8.537024980200894788E-16 ) ) ;
#21754 = CARTESIAN_POINT ( 'NONE',  ( -6.158966240078259879, 30.49883854570459718, 2.286114001711006871 ) ) ;
#21755 = CARTESIAN_POINT ( 'NONE',  ( 1.580769961479467911, 28.79261460129497863, -4.363931058323818668 ) ) ;
#21756 = ADVANCED_FACE ( 'NONE', ( #13462 ), #32051, .F. ) ;
#21757 = DIRECTION ( 'NONE',  ( 0.000000000000000000, 0.000000000000000000, 1.000000000000000000 ) ) ;
#21758 = CARTESIAN_POINT ( 'NONE',  ( -41.23752580366542730, 23.26788267949596190, 1.523999999999994248 ) ) ;
#21759 = CARTESIAN_POINT ( 'NONE',  ( -17.14499999999999957, 71.11999999999999034, 5.016499999999999737 ) ) ;
#21760 = CARTESIAN_POINT ( 'NONE',  ( 0.3809694336148531368, 120.1716774721349168, -0.6201936767135831641 ) ) ;
#21761 = CARTESIAN_POINT ( 'NONE',  ( -13.37627446016234600, 119.7032035076741465, 0.2201875619950501017 ) ) ;
#21762 = ORIENTED_EDGE ( 'NONE', *, *, #16452, .T. ) ;
#21763 = CARTESIAN_POINT ( 'NONE',  ( -58.32144855246983184, 1.173557705256414341, -1.098103182356013230 ) ) ;
#21764 = ORIENTED_EDGE ( 'NONE', *, *, #4010, .F. ) ;
#21765 = DIRECTION ( 'NONE',  ( -0.1906721105965052399, 0.9816537812491094028, 7.161032787277034991E-15 ) ) ;
#21766 = CARTESIAN_POINT ( 'NONE',  ( -15.72520672816718523, 146.8976288387275133, -0.2472165429730639463 ) ) ;
#21767 = CARTESIAN_POINT ( 'NONE',  ( 6.028374245061780989, -14.54558069259788411, 1.726931113533916040 ) ) ;
#21768 = CARTESIAN_POINT ( 'NONE',  ( -14.64490033095734134, 154.5799843816573684, 1.633817034445554039 ) ) ;
#21769 = AXIS2_PLACEMENT_3D ( 'NONE', #22817, #33076, #36687 ) ;
#21770 = CARTESIAN_POINT ( 'NONE',  ( 17.54374246740519538, 153.9260871938423065, -1.166327135487699618 ) ) ;
#21771 = CARTESIAN_POINT ( 'NONE',  ( -4.012847786888796620, 11.73797844546971270, -2.294585225469591983 ) ) ;
#21772 = CARTESIAN_POINT ( 'NONE',  ( -8.183336086940967036, 117.5993832199734328, -0.5018928202873275124 ) ) ;
#21773 = CARTESIAN_POINT ( 'NONE',  ( -57.56413824804958068, 1.999148952895605014, -1.762603608441677183 ) ) ;
#21774 = ORIENTED_EDGE ( 'NONE', *, *, #24468, .T. ) ;
#21775 = CARTESIAN_POINT ( 'NONE',  ( -5.563655970165373610, 116.7104814527052667, 0.001055824976130279166 ) ) ;
#21776 = CARTESIAN_POINT ( 'NONE',  ( -6.550797450135577910E-14, 84.67546620154573134, 2.164564701558966795E-29 ) ) ;
#21777 = CARTESIAN_POINT ( 'NONE',  ( -9.926448497735856691, 122.5082557396031291, 1.019319756893169338 ) ) ;
#21778 = CARTESIAN_POINT ( 'NONE',  ( -16.60960244842765832, 9.026346327358517385, 2.034089647357696937E-15 ) ) ;
#21779 = CARTESIAN_POINT ( 'NONE',  ( 2.404146712672410757, 157.7073581658784178, -1.626633079703769136 ) ) ;
#21780 = AXIS2_PLACEMENT_3D ( 'NONE', #13697, #26688, #40116 ) ;
#21781 = CARTESIAN_POINT ( 'NONE',  ( -19.67869083727186919, 136.1149058410947532, -2.266608711299009649 ) ) ;
#21782 = CARTESIAN_POINT ( 'NONE',  ( -49.59816314059867182, 17.91649583374774224, -5.069000701391666475 ) ) ;
#21783 = CARTESIAN_POINT ( 'NONE',  ( 8.389933090069224164, 122.6561726160659731, -0.4454891811124966350 ) ) ;
#21784 = ORIENTED_EDGE ( 'NONE', *, *, #34150, .F. ) ;
#21785 = CARTESIAN_POINT ( 'NONE',  ( -1.354060893033618429, 119.5584937100158243, -0.6194060083641331760 ) ) ;
#21786 = CARTESIAN_POINT ( 'NONE',  ( 4.220783105811589664, -15.35787857112312693, 0.3368293509108917783 ) ) ;
#21787 = CARTESIAN_POINT ( 'NONE',  ( -4.144796762172593851, 118.2390927319115832, -0.4001549744010635123 ) ) ;
#21788 = CIRCLE ( 'NONE', #23844, 5.080000000000006288 ) ;
#21789 = CARTESIAN_POINT ( 'NONE',  ( -58.37241122568488549, -0.2962816677227753104, -1.034007718770489626E-14 ) ) ;
#21790 = CARTESIAN_POINT ( 'NONE',  ( -4.932064943850939187, 117.4109299206517818, 0.9378731322835484052 ) ) ;
#21791 = CARTESIAN_POINT ( 'NONE',  ( 11.09706570755277788, 123.3376105302527037, 1.576947150105312501 ) ) ;
#21792 = DIRECTION ( 'NONE',  ( -0.7517731442105912709, 0.6594218222380281436, -8.537024980200781389E-16 ) ) ;
#21793 =( BOUNDED_SURFACE ( )  B_SPLINE_SURFACE ( 3, 2, ( 
 ( #3719, #29682, #14314 ),
 ( #28530, #41746, #31936 ),
 ( #30722, #14529, #11342 ),
 ( #15526, #15312, #24328 ),
 ( #41535, #37128, #31722 ),
 ( #37334, #31507, #41326 ),
 ( #38121, #40545, #20918 ),
 ( #2354, #33941, #11132 ),
 ( #22314, #21121, #2771 ),
 ( #27538, #28733, #18924 ) ),
 .UNSPECIFIED., .F., .F., .T. ) 
 B_SPLINE_SURFACE_WITH_KNOTS ( ( 4, 2, 2, 2, 4 ),
 ( 3, 3 ),
 ( 1.570796326794897002, 1.963495408493620920, 2.356194490192344837, 2.748893571891068532, 3.141592653589792672 ),
 ( 0.000000000000000000, 1.000000000000000000 ),
 .UNSPECIFIED. ) 
 GEOMETRIC_REPRESENTATION_ITEM ( )  RATIONAL_B_SPLINE_SURFACE ( (
 ( 1.000000000000000000, 0.7071067811865475727, 1.000000000000000000),
 ( 1.000000000000000000, 0.7139102541735814489, 1.000000000000000000),
 ( 1.000000000000000000, 0.7206031636706378141, 1.000000000000000000),
 ( 1.000000000000000000, 0.7328301610699465840, 1.000000000000000000),
 ( 1.000000000000000000, 0.7383589052090805405, 1.000000000000000000),
 ( 1.000000000000000000, 0.7475127447242121415, 1.000000000000000000),
 ( 1.000000000000000000, 0.7511365686956648080, 1.000000000000000000),
 ( 1.000000000000000000, 0.7560206254140624527, 1.000000000000000000),
 ( 1.000000000000000000, 0.7572851909592275277, 1.000000000000000000),
 ( 1.000000000000000000, 0.7572803591334833495, 1.000000000000000000) ) ) 
 REPRESENTATION_ITEM ( '' )  SURFACE ( )  );
#21794 = AXIS2_PLACEMENT_3D ( 'NONE', #30852, #14652, #27656 ) ;
#21795 = CARTESIAN_POINT ( 'NONE',  ( -8.432237393326710517, 2.893158626077577900, 0.2611430682616783239 ) ) ;
#21796 = CARTESIAN_POINT ( 'NONE',  ( -0.004910621514806326471, 156.3161161488371533, 0.2457475809811482670 ) ) ;
#21797 = CARTESIAN_POINT ( 'NONE',  ( 2.722315517715700572, 118.0959538166519849, -0.8461704532092527709 ) ) ;
#21799 = ORIENTED_EDGE ( 'NONE', *, *, #8325, .T. ) ;
#21798 = DIRECTION ( 'NONE',  ( -0.9998004120163609398, 0.000000000000000000, -0.01997839162482749689 ) ) ;
#21800 = CARTESIAN_POINT ( 'NONE',  ( -0.2177282545546737058, 118.1588900835526914, 0.9015745107222330468 ) ) ;
#21801 = CIRCLE ( 'NONE', #6217, 0.2540000000000000036 ) ;
#21802 = CARTESIAN_POINT ( 'NONE',  ( -58.37241122568488549, -0.2962816677227753104, -1.034007718770489626E-14 ) ) ;
#21803 = CARTESIAN_POINT ( 'NONE',  ( -7.784012322544769269, 122.6313477034873074, -0.1555430911242075831 ) ) ;
#21804 = CARTESIAN_POINT ( 'NONE',  ( -5.177913976931302287, 77.01756249999996840, -5.372099999999996989 ) ) ;
#21805 = CARTESIAN_POINT ( 'NONE',  ( -49.29989578322635424, 20.38947471906982756, 3.123819567266189257 ) ) ;
#21806 = CARTESIAN_POINT ( 'NONE',  ( -22.98049992366342309, 150.1579452496398801, -0.3057203305217676137 ) ) ;
#21807 = B_SPLINE_CURVE_WITH_KNOTS ( 'NONE', 3,
 ( #27380, #10979, #7801, #29743, #33161, #8002 ),
 .UNSPECIFIED., .F., .F.,
 ( 4, 2, 4 ),
 ( 0.01688307072824751093, 0.01716653801739397023, 0.01745000530654042953 ),
 .UNSPECIFIED. ) ;
#21808 = ORIENTED_EDGE ( 'NONE', *, *, #36085, .T. ) ;
#21809 = CARTESIAN_POINT ( 'NONE',  ( -51.10637697011796377, 21.44594517096482633, -1.085271236684668311E-14 ) ) ;
#21810 = CARTESIAN_POINT ( 'NONE',  ( 6.041926471666161369, 121.4447802455698877, 0.08406784148116053235 ) ) ;
#21811 = CARTESIAN_POINT ( 'NONE',  ( -7.920006352636957736, 122.0419191725281678, 0.5993308652498723355 ) ) ;
#21812 = VERTEX_POINT ( 'NONE', #699 ) ;
#21813 = CARTESIAN_POINT ( 'NONE',  ( 0.8976087670000849617, 115.7028554113044123, -1.718884712376715251 ) ) ;
#21814 = CARTESIAN_POINT ( 'NONE',  ( -7.577119205441469774, 122.4179301937671767, -0.2905534069474315917 ) ) ;
#21815 = CARTESIAN_POINT ( 'NONE',  ( 2.821817058828279823, -15.16010343277639194, 5.768636546787819341 ) ) ;
#21816 = CARTESIAN_POINT ( 'NONE',  ( -13.46300103848319196, 120.9245410081625209, 0.9131080906212013515 ) ) ;
#21817 = CARTESIAN_POINT ( 'NONE',  ( 5.477532837487817829, 78.92140300690502386, -5.132221182818687666 ) ) ;
#21818 = CARTESIAN_POINT ( 'NONE',  ( 15.78464309758866690, 121.0087326939336378, 0.5477818752361017784 ) ) ;
#21819 = CARTESIAN_POINT ( 'NONE',  ( 9.098285506954120194, 153.9557200233357435, 0.2398147890565895668 ) ) ;
#21820 = DIRECTION ( 'NONE',  ( 5.188838149069472160E-16, -1.699382548006136559E-16, -1.000000000000000000 ) ) ;
#21821 = CARTESIAN_POINT ( 'NONE',  ( 0.9647673288271847447, 27.50405299253531410, 0.1566625405351598777 ) ) ;
#21822 = CARTESIAN_POINT ( 'NONE',  ( -1.417643301182503368, 159.6052071245950970, -0.07209812905978379982 ) ) ;
#21823 = CARTESIAN_POINT ( 'NONE',  ( -3.682264917456324227, 88.99346620154574339, -0.07358041635423923088 ) ) ;
#21824 = EDGE_LOOP ( 'NONE', ( #13420, #24654, #42111, #41499 ) ) ;
#21825 = CARTESIAN_POINT ( 'NONE',  ( 4.084276569795989964, 118.3417739162233744, 0.9965765103875263708 ) ) ;
#21826 = CARTESIAN_POINT ( 'NONE',  ( 4.135298993362768627, -14.76517611359900961, -2.065434832541708676 ) ) ;
#21827 = CARTESIAN_POINT ( 'NONE',  ( 21.74240605069414300, 146.0876064316611860, 2.155783927327832306 ) ) ;
#21828 = CARTESIAN_POINT ( 'NONE',  ( 15.41274837478107784, 125.4902479783272184, -1.384083614372567661 ) ) ;
#21829 = CARTESIAN_POINT ( 'NONE',  ( -8.411989387141455055, 18.26859176889432490, 0.3690887223902433734 ) ) ;
#21830 = CARTESIAN_POINT ( 'NONE',  ( -19.75679031132836272, 152.3633698111425758, -1.804147069793666347 ) ) ;
#21831 = CARTESIAN_POINT ( 'NONE',  ( 4.843357629187326374, 117.6435499053430931, -0.9176853102465485357 ) ) ;
#21832 = CIRCLE ( 'NONE', #34120, 0.8889999999999977920 ) ;
#21833 = CARTESIAN_POINT ( 'NONE',  ( 4.730021378956775102, 112.7831754354443348, 2.563638443952895862 ) ) ;
#21834 = CARTESIAN_POINT ( 'NONE',  ( -1.606403942294512222, 120.9755568995931156, 0.03214495494220275668 ) ) ;
#21835 = CARTESIAN_POINT ( 'NONE',  ( -4.182621382392013309, 157.4559852174668322, -1.843664507743932202 ) ) ;
#21836 = CARTESIAN_POINT ( 'NONE',  ( 4.016706779461339138, -15.37834506377831723, 5.009826762111060816 ) ) ;
#21837 = AXIS2_PLACEMENT_3D ( 'NONE', #25531, #38532, #19750 ) ;
#21838 = CARTESIAN_POINT ( 'NONE',  ( -10.28897677580358305, 56.51499999999998636, -4.381499999999999950 ) ) ;
#21839 = CARTESIAN_POINT ( 'NONE',  ( -3.159512914937968819, 117.3993812128981347, -1.388958443500331263 ) ) ;
#21840 = ORIENTED_EDGE ( 'NONE', *, *, #2521, .T. ) ;
#21841 = CARTESIAN_POINT ( 'NONE',  ( 18.41737859239631803, 149.0103496150362901, 2.461622840412570845 ) ) ;
#21842 = DIRECTION ( 'NONE',  ( 0.7770581983690854067, -0.6294287539884012572, 5.101669463485840682E-16 ) ) ;
#21843 = AXIS2_PLACEMENT_3D ( 'NONE', #41490, #36309, #2519 ) ;
#21844 = CARTESIAN_POINT ( 'NONE',  ( 17.14499999999999957, 71.11999999999999034, 5.016499999999999737 ) ) ;
#21845 = CARTESIAN_POINT ( 'NONE',  ( -0.5468943487521297220, 107.2171362991012842, 4.774625097732313250 ) ) ;
#21846 = CARTESIAN_POINT ( 'NONE',  ( 1.420544585151703343, -13.23898594424576203, -8.332176651214544094 ) ) ;
#21847 = CARTESIAN_POINT ( 'NONE',  ( -0.004916276843216625669, 120.6356583033945782, 0.2460305967400715221 ) ) ;
#21848 = DIRECTION ( 'NONE',  ( -0.8138664877804110409, -0.5810519254489896479, 0.000000000000000000 ) ) ;
#21849 = CARTESIAN_POINT ( 'NONE',  ( 15.64055365641533690, 121.4606353739761744, -0.3859511643760804023 ) ) ;
#21850 = DIRECTION ( 'NONE',  ( -0.9336303900108928744, -0.3582377630123714241, 0.000000000000000000 ) ) ;
#21851 = AXIS2_PLACEMENT_3D ( 'NONE', #13863, #40497, #26858 ) ;
#21852 = CARTESIAN_POINT ( 'NONE',  ( -58.34786123531646496, -0.2455935055575208803, 0.1844583020148576336 ) ) ;
#21853 = DIRECTION ( 'NONE',  ( -5.206863593109713661E-17, 1.000000000000000000, -1.077750396879097183E-30 ) ) ;
#21854 = AXIS2_PLACEMENT_3D ( 'NONE', #31461, #15265, #11441 ) ;
#21855 = EDGE_CURVE ( 'NONE', #10591, #34625, #40715, .T. ) ;
#21856 = EDGE_CURVE ( 'NONE', #27727, #8502, #20334, .T. ) ;
#21857 = AXIS2_PLACEMENT_3D ( 'NONE', #38096, #38514, #8911 ) ;
#21858 = CARTESIAN_POINT ( 'NONE',  ( 2.063686733023939901, -15.30319371230426917, 5.972472134935500776 ) ) ;
#21859 = CARTESIAN_POINT ( 'NONE',  ( -4.123368102914265698, 118.2429491485453354, 0.1806032781032593237 ) ) ;
#21860 = CARTESIAN_POINT ( 'NONE',  ( 5.232282628590676943, 115.9099169135977689, -1.117942969498063155 ) ) ;
#21861 = ORIENTED_EDGE ( 'NONE', *, *, #10863, .T. ) ;
#21862 = CARTESIAN_POINT ( 'NONE',  ( -48.59875010875282442, 18.41211343146811785, 5.165832069028382101 ) ) ;
#21863 = CARTESIAN_POINT ( 'NONE',  ( -8.148487026236251651, 120.7334362890933477, -1.392358570714556487 ) ) ;
#21864 = DIRECTION ( 'NONE',  ( 4.017660918040594346E-17, -1.000000000000000000, -2.376309959284834438E-19 ) ) ;
#21865 = CARTESIAN_POINT ( 'NONE',  ( -8.043896744444055003, 154.6119571123129788, -0.8805139685443125197 ) ) ;
#21866 = CARTESIAN_POINT ( 'NONE',  ( -29.91360363449004822, 70.04874496952839991, 1.523999999999992250 ) ) ;
#21867 = CARTESIAN_POINT ( 'NONE',  ( 0.01782678998956764571, 118.1651004037419881, -0.8921253700480482607 ) ) ;
#21868 = EDGE_LOOP ( 'NONE', ( #15009, #18176, #39692, #3098 ) ) ;
#21869 = CARTESIAN_POINT ( 'NONE',  ( 4.419457123578296454, 17.78516144714274105, -1.360477052881604143 ) ) ;
#21870 = CARTESIAN_POINT ( 'NONE',  ( -29.22735587859570927, 60.46978361834971594, 1.523999999999994026 ) ) ;
#21871 = DIRECTION ( 'NONE',  ( -5.188838149069471174E-16, 1.699382548006136313E-16, 1.000000000000000000 ) ) ;
#21872 = CARTESIAN_POINT ( 'NONE',  ( 6.072850655491107474, 78.87349744216250258, -4.348040511725084656 ) ) ;
#21873 = DIRECTION ( 'NONE',  ( -0.9807655518882886225, 0.1951894777626621558, -5.420735302995426205E-16 ) ) ;
#21874 = CARTESIAN_POINT ( 'NONE',  ( 6.073146511589309071, 121.4483376143599287, 0.1695659588288715436 ) ) ;
#21875 = CARTESIAN_POINT ( 'NONE',  ( -17.31476582418722643, 62.07284264934779827, -1.269999999999999130 ) ) ;
#21876 = CARTESIAN_POINT ( 'NONE',  ( 22.50793294095875652, 142.2972183020237367, 1.640122747091714128 ) ) ;
#21877 = CARTESIAN_POINT ( 'NONE',  ( -17.14500000000000313, 71.11999999999999034, -5.080000000000000959 ) ) ;
#21879 = CARTESIAN_POINT ( 'NONE',  ( 6.834340443517000985, 118.4250403807481575, -0.8562881416378697041 ) ) ;
#21878 = CARTESIAN_POINT ( 'NONE',  ( 2.460727335429193197, -15.06314154744310585, 4.845259171755021299 ) ) ;
#21880 = CARTESIAN_POINT ( 'NONE',  ( -11.06957317628273785, 122.5598569164413334, 1.209814958810230934 ) ) ;
#21881 = CARTESIAN_POINT ( 'NONE',  ( -4.282102574861781363, 27.11529131024228434, -1.748715980913516876 ) ) ;
#21882 = CARTESIAN_POINT ( 'NONE',  ( -0.3355986945388581555, 116.9201722098172382, -0.3169108175686566886 ) ) ;
#21883 = CARTESIAN_POINT ( 'NONE',  ( -0.2078495401522961472, -3.970246887572310257, -0.9510052327550873041 ) ) ;
#21884 = ORIENTED_EDGE ( 'NONE', *, *, #19063, .T. ) ;
#21885 = CARTESIAN_POINT ( 'NONE',  ( -54.22787649382022579, 6.886497292746652121, 0.2709450413640898669 ) ) ;
#21886 = CARTESIAN_POINT ( 'NONE',  ( -13.37097581265842905, 134.1388935151753401, 0.4393653360420519682 ) ) ;
#21887 = CARTESIAN_POINT ( 'NONE',  ( 4.916912942907655903, -13.49232782388964935, 3.465564004687308408 ) ) ;
#21888 = CARTESIAN_POINT ( 'NONE',  ( 2.625396581831431320, 120.2926465633240127, -0.4415429531236469418 ) ) ;
#21889 = EDGE_LOOP ( 'NONE', ( #13776, #9518, #30950, #28918 ) ) ;
#21890 = CARTESIAN_POINT ( 'NONE',  ( 1.253061391183938555, 115.7029074980223271, 1.740285132395945178 ) ) ;
#21891 = CIRCLE ( 'NONE', #3569, 5.588000000000006295 ) ;
#21892 = ORIENTED_EDGE ( 'NONE', *, *, #392, .F. ) ;
#21893 = CARTESIAN_POINT ( 'NONE',  ( -4.876515041417334828, 117.7132576400690027, -0.9240722683427993189 ) ) ;
#21894 = ADVANCED_FACE ( 'NONE', ( #20251 ), #19836, .T. ) ;
#21895 = CARTESIAN_POINT ( 'NONE',  ( 15.77133435453283461, 146.5691041611200660, 0.3151487940933137555 ) ) ;
#21896 = VERTEX_POINT ( 'NONE', #41870 ) ;
#21897 = CARTESIAN_POINT ( 'NONE',  ( 19.60096582671575405, 145.2539617268756729, 2.527680105953240552 ) ) ;
#21898 = DIRECTION ( 'NONE',  ( -5.206863593109713661E-17, 1.000000000000000000, -1.077750396879097183E-30 ) ) ;
#21899 = CARTESIAN_POINT ( 'NONE',  ( -8.594951744493886991, 74.76616009375631222, -1.523999999999996913 ) ) ;
#21900 = CARTESIAN_POINT ( 'NONE',  ( 4.996532045110951614, 117.4672001989742398, -0.7808144642989416351 ) ) ;
#21901 = CIRCLE ( 'NONE', #5651, 0.6349999999999984546 ) ;
#21902 = CARTESIAN_POINT ( 'NONE',  ( 17.03046551078681148, 122.6950552906510694, 0.003367075177501197957 ) ) ;
#21903 = CARTESIAN_POINT ( 'NONE',  ( -6.008977632366433015E-14, 69.43546620154573645, 9.241195598681324794E-17 ) ) ;
#21904 = CARTESIAN_POINT ( 'NONE',  ( -46.92969783022256536, 25.19817632415814046, 1.844736899205347891 ) ) ;
#21905 = CARTESIAN_POINT ( 'NONE',  ( -46.97515415817102280, 24.89137758704634962, 2.045406795549888468 ) ) ;
#21906 = CARTESIAN_POINT ( 'NONE',  ( 1.774262667879180411, -15.10206561957146221, 5.641947496857006250 ) ) ;
#21907 = CARTESIAN_POINT ( 'NONE',  ( -46.97515415817095175, 24.89137758704647396, 2.045406795549891577 ) ) ;
#21908 = DIRECTION ( 'NONE',  ( -1.000000000000000000, 0.000000000000000000, -6.146657985744586818E-16 ) ) ;
#21909 = EDGE_CURVE ( 'NONE', #10948, #5725, #39882, .T. ) ;
#21910 = CARTESIAN_POINT ( 'NONE',  ( -4.749506590746891632, 117.9455148129567164, 0.6338826763805054387 ) ) ;
#21911 = ORIENTED_EDGE ( 'NONE', *, *, #19130, .F. ) ;
#21912 = ORIENTED_EDGE ( 'NONE', *, *, #18882, .T. ) ;
#21913 = LINE ( 'NONE', #21077, #22699 ) ;
#21914 = CARTESIAN_POINT ( 'NONE',  ( 5.671516376864802034, 118.3593096970241305, -0.9503249289038079306 ) ) ;
#21915 = CARTESIAN_POINT ( 'NONE',  ( -3.549733929830021673, 110.1236525333376619, -3.577684766704721575 ) ) ;
#21916 = CARTESIAN_POINT ( 'NONE',  ( 4.859873572602068315, 117.5461019621290575, 1.119800123233829270 ) ) ;
#21917 = CARTESIAN_POINT ( 'NONE',  ( 2.568134854143032442, -15.02010252187911554, 4.714990346623905815 ) ) ;
#21918 = CARTESIAN_POINT ( 'NONE',  ( -0.4232488410869896800, 124.9344662015457317, -0.008457519121176893320 ) ) ;
#21919 = CIRCLE ( 'NONE', #3598, 0.6350000000000014522 ) ;
#21920 = CARTESIAN_POINT ( 'NONE',  ( -23.14542444889682216, 82.37908244650444090, 1.523999999999993582 ) ) ;
#21921 = CARTESIAN_POINT ( 'NONE',  ( -17.64290547347870941, 83.78857423953914463, 1.269999999999996909 ) ) ;
#21922 = DIRECTION ( 'NONE',  ( 5.188838149069472160E-16, -1.699382548006136559E-16, -1.000000000000000000 ) ) ;
#21923 = CARTESIAN_POINT ( 'NONE',  ( 4.093446853122521212, 111.5999093057820772, -2.867423493935855827 ) ) ;
#21924 = CARTESIAN_POINT ( 'NONE',  ( -17.41367791652951880, 147.5992144370567871, -2.159268082968857971 ) ) ;
#21925 = EDGE_CURVE ( 'NONE', #4212, #11474, #23020, .T. ) ;
#21926 = CARTESIAN_POINT ( 'NONE',  ( 7.002510704594238966, 121.9568449727899520, 0.1399268299516837899 ) ) ;
#21927 = DIRECTION ( 'NONE',  ( -0.9876665170007974393, 0.1565721916417901483, -8.537024980200831679E-16 ) ) ;
#21928 = DIRECTION ( 'NONE',  ( 0.000000000000000000, 1.000000000000000000, 0.000000000000000000 ) ) ;
#21929 = CARTESIAN_POINT ( 'NONE',  ( 4.513502956352341222, 8.064680226961385756, -0.9949261897555528034 ) ) ;
#21931 = ORIENTED_EDGE ( 'NONE', *, *, #27889, .T. ) ;
#21930 = CARTESIAN_POINT ( 'NONE',  ( 22.38168272118564062, 137.0915487549672491, 1.023064006592828479 ) ) ;
#21932 = CARTESIAN_POINT ( 'NONE',  ( 1.938810462764684051, 105.1240917556268641, -4.970498420434350528 ) ) ;
#21933 = CARTESIAN_POINT ( 'NONE',  ( 3.857521300888583582, -15.67877420849868386, 3.673684628067402702 ) ) ;
#21934 = CARTESIAN_POINT ( 'NONE',  ( -6.702632528927957800, 119.6463993818898359, 1.017002412926887533 ) ) ;
#21935 = CARTESIAN_POINT ( 'NONE',  ( -0.1630216852218501489, 24.74361041950371032, -0.9604350664704873752 ) ) ;
#21936 = CARTESIAN_POINT ( 'NONE',  ( -0.4248780512631177841, 5.470267980206036107, 0.8793239699972363876 ) ) ;
#21937 = EDGE_LOOP ( 'NONE', ( #365, #40481, #39724, #3002 ) ) ;
#21938 = AXIS2_PLACEMENT_3D ( 'NONE', #37226, #30617, #1460 ) ;
#21939 = ORIENTED_EDGE ( 'NONE', *, *, #17360, .T. ) ;
#21940 = DIRECTION ( 'NONE',  ( -0.8745520943968240202, 0.4849315768086551737, -5.361993529360572958E-16 ) ) ;
#21941 = CARTESIAN_POINT ( 'NONE',  ( 0.09082259786502508425, 105.9597790263619146, 5.306270932934927131 ) ) ;
#21942 = CARTESIAN_POINT ( 'NONE',  ( -8.467456592458740161, 122.5794309061019618, 0.5337204191277992171 ) ) ;
#21943 = FACE_OUTER_BOUND ( 'NONE', #16287, .T. ) ;
#21944 = CARTESIAN_POINT ( 'NONE',  ( 3.884801864383396808, -13.20605796264157128, 2.953397552313849150 ) ) ;
#21945 = CARTESIAN_POINT ( 'NONE',  ( 7.383627470571713758, 120.8389031223305352, -0.9130476668403028073 ) ) ;
#21946 = CARTESIAN_POINT ( 'NONE',  ( -19.91185195753441661, 145.3736917597469471, -2.515063280254572042 ) ) ;
#21947 = CARTESIAN_POINT ( 'NONE',  ( -17.14499999999999957, 71.11999999999999034, 5.016499999999999737 ) ) ;
#21948 = CARTESIAN_POINT ( 'NONE',  ( 8.557792064668554133, 118.7566837416166692, 1.194711599118532863 ) ) ;
#21949 = CARTESIAN_POINT ( 'NONE',  ( -0.8575334777045592327, 37.18052207920313634, 1.701599969488736930 ) ) ;
#21950 = ADVANCED_FACE ( 'NONE', ( #26451 ), #10678, .F. ) ;
#21951 = CARTESIAN_POINT ( 'NONE',  ( 4.305249565653697985, 155.8363458669846864, -0.2390946120805818864 ) ) ;
#21952 = ORIENTED_EDGE ( 'NONE', *, *, #12295, .F. ) ;
#21953 = CARTESIAN_POINT ( 'NONE',  ( -0.4669360306570718988, 105.9268256211375103, -5.319786075441130357 ) ) ;
#21954 = CARTESIAN_POINT ( 'NONE',  ( -6.501940248589056060E-14, 66.13346620154574396, -9.529289869050788486E-18 ) ) ;
#21955 = ADVANCED_FACE ( 'NONE', ( #15640 ), #33958, .F. ) ;
#21956 = DIRECTION ( 'NONE',  ( -0.9891443546370349837, 0.000000000000000000, 0.1469470846586743984 ) ) ;
#21957 = VECTOR ( 'NONE', #35417, 1000.000000000000227 ) ;
#21958 = ADVANCED_FACE ( 'NONE', ( #27912 ), #25897, .T. ) ;
#21959 = CARTESIAN_POINT ( 'NONE',  ( 7.984751813625430295, 22.47881364768745271, 2.830840501157275924 ) ) ;
#21960 = CARTESIAN_POINT ( 'NONE',  ( 16.88761465400175155, 147.3835828867039766, 1.922606999130501482 ) ) ;
#21961 = DIRECTION ( 'NONE',  ( -0.9998004120163609398, 0.000000000000000000, -0.01997839162482749689 ) ) ;
#21962 = CARTESIAN_POINT ( 'NONE',  ( 4.725057015249740644, 116.7592613395855352, 0.05262260997884649766 ) ) ;
#21963 = CARTESIAN_POINT ( 'NONE',  ( -6.300894124712325350, 120.0808430858776887, 0.2013153013476513264 ) ) ;
#21964 = AXIS2_PLACEMENT_3D ( 'NONE', #30827, #30409, #7429 ) ;
#21965 = FACE_OUTER_BOUND ( 'NONE', #1080, .T. ) ;
#21966 = CARTESIAN_POINT ( 'NONE',  ( 15.26262975078991779, 148.0175730704188481, 0.3049836654608578113 ) ) ;
#21967 = ADVANCED_FACE ( 'NONE', ( #18948 ), #41348, .F. ) ;
#21968 = CARTESIAN_POINT ( 'NONE',  ( 5.527521262545286085, 2.498091250051501344, 6.371381250375013572 ) ) ;
#21969 = CARTESIAN_POINT ( 'NONE',  ( 2.167983032549695821, 116.6620882976681628, -0.3727921820594300439 ) ) ;
#21970 = CARTESIAN_POINT ( 'NONE',  ( 0.05238710762246717723, 113.0327356262574341, -2.621665085262795181 ) ) ;
#21971 = CARTESIAN_POINT ( 'NONE',  ( -16.02764313970815735, 80.34763903973272647, -1.524000000000002020 ) ) ;
#21972 = CARTESIAN_POINT ( 'NONE',  ( -7.401523468229766145, -5.981721843848114339, 4.095665678060115944 ) ) ;
#21973 = CARTESIAN_POINT ( 'NONE',  ( -0.02812206864257424735, 117.9394488565463064, 1.407343427015907311 ) ) ;
#21974 = DIRECTION ( 'NONE',  ( -5.188838149069472160E-16, 1.699382548006136559E-16, 1.000000000000000000 ) ) ;
#21975 = CARTESIAN_POINT ( 'NONE',  ( -17.14500000000466784, 71.11999999999886768, -1.270000000000000684 ) ) ;
#21976 = CARTESIAN_POINT ( 'NONE',  ( 0.6988325576870501044, 114.3327162918516962, -2.155465965906839809 ) ) ;
#21977 = CARTESIAN_POINT ( 'NONE',  ( -5.638719538426442135, 159.1014311945586712, 0.3820744581509935567 ) ) ;
#21978 = ORIENTED_EDGE ( 'NONE', *, *, #34186, .T. ) ;
#21979 = CARTESIAN_POINT ( 'NONE',  ( -58.39046968809522298, 1.092456688167306567, -0.3056578461530352064 ) ) ;
#21980 = VERTEX_POINT ( 'NONE', #35360 ) ;
#21981 = CARTESIAN_POINT ( 'NONE',  ( -42.52099730114249354, 21.88661877469185413, -1.711735796961263656 ) ) ;
#21982 = CARTESIAN_POINT ( 'NONE',  ( -11.79229084918624082, 130.2874513316071443, -0.1788083452990229527 ) ) ;
#21983 = CARTESIAN_POINT ( 'NONE',  ( 2.291706021380962355, -15.53059561260056221, 5.887745402940570472 ) ) ;
#21984 = CARTESIAN_POINT ( 'NONE',  ( -16.30903692877122424, 153.4734386769207504, 1.632589361097313230 ) ) ;
#21985 = CARTESIAN_POINT ( 'NONE',  ( 3.058359628041792622, 159.2229145144301867, -0.9584471420995392954 ) ) ;
#21986 = CARTESIAN_POINT ( 'NONE',  ( 3.121479725567877228, 16.06095178295013071, 3.416230322513892137 ) ) ;
#21987 = CARTESIAN_POINT ( 'NONE',  ( 0.004910662370358964517, 159.5928157220454295, -0.2457496255665020946 ) ) ;
#21988 = CARTESIAN_POINT ( 'NONE',  ( -53.83641692055964256, 9.560737412489993758, -3.788401990392710861 ) ) ;
#21989 = AXIS2_PLACEMENT_3D ( 'NONE', #26108, #22262, #28886 ) ;
#21990 = EDGE_CURVE ( 'NONE', #39565, #35799, #18314, .T. ) ;
#21991 = VERTEX_POINT ( 'NONE', #6190 ) ;
#21992 = CARTESIAN_POINT ( 'NONE',  ( 0.3920235582991468126, 123.4679809879532542, 0.1617017839830492132 ) ) ;
#21993 = CARTESIAN_POINT ( 'NONE',  ( -6.486711254249450261E-14, 72.48346620154573827, 1.207165459670006807E-19 ) ) ;
#21994 = CARTESIAN_POINT ( 'NONE',  ( -11.97328186178021170, 153.4554508723442439, 1.471200310048991655 ) ) ;
#21995 = DIRECTION ( 'NONE',  ( 1.011795553208986377E-16, 1.000000000000000000, -0.000000000000000000 ) ) ;
#21996 = CARTESIAN_POINT ( 'NONE',  ( 19.00246547725214086, 147.5601278813269914, -1.724645192979526342 ) ) ;
#21997 = CARTESIAN_POINT ( 'NONE',  ( -21.11954758237303764, 149.1058327099893290, -2.305704729659639796 ) ) ;
#21998 = CARTESIAN_POINT ( 'NONE',  ( -49.66210360255988832, 16.76989353321783227, -4.946330335750499962 ) ) ;
#21999 = CIRCLE ( 'NONE', #36291, 9.048749999999998295 ) ;
#22000 = CARTESIAN_POINT ( 'NONE',  ( 8.995803412248823960, 123.1852847016406685, -0.4677080646552714271 ) ) ;
#22001 = ORIENTED_EDGE ( 'NONE', *, *, #21004, .F. ) ;
#22002 = CARTESIAN_POINT ( 'NONE',  ( -3.791208754741646647, 156.9018388488748883, -1.699278904607348872 ) ) ;
#22003 = CARTESIAN_POINT ( 'NONE',  ( 3.668568818830479028, -15.43917834477946727, 2.972162690469843049 ) ) ;
#22004 = CARTESIAN_POINT ( 'NONE',  ( -4.151500737348964520, 118.2394118959124114, -0.3932187221707064695 ) ) ;
#22005 = ADVANCED_FACE ( 'NONE', ( #12569 ), #14222, .T. ) ;
#22006 = EDGE_CURVE ( 'NONE', #4510, #6464, #38054, .T. ) ;
#22007 = CARTESIAN_POINT ( 'NONE',  ( -4.786196459852546603, 117.6677270402089022, 0.9346353507170748198 ) ) ;
#22008 = CARTESIAN_POINT ( 'NONE',  ( 17.39571694528370216, 144.3974720067888313, 2.245075470287479558 ) ) ;
#22009 = CARTESIAN_POINT ( 'NONE',  ( 3.009276887026298031, 39.20946620154573026, -1.210121013456480599 ) ) ;
#22010 = CIRCLE ( 'NONE', #280, 0.5080000000000002292 ) ;
#22011 = CARTESIAN_POINT ( 'NONE',  ( 7.936949992814905208, -1.433721018288910853, -2.821688713676304250 ) ) ;
#22012 = CARTESIAN_POINT ( 'NONE',  ( 1.583718294068441557, 120.9073379818811134, 0.1636693232558003586 ) ) ;
#22013 = DIRECTION ( 'NONE',  ( -0.9454731675810326141, 0.3256999990547876922, -8.537024980200857317E-16 ) ) ;
#22014 = VECTOR ( 'NONE', #22427, 1000.000000000000000 ) ;
#22015 = CARTESIAN_POINT ( 'NONE',  ( -41.98003980773050614, 22.15641273310255954, -0.9734550245785090761 ) ) ;
#22016 = CARTESIAN_POINT ( 'NONE',  ( -17.76856900107737403, 61.81127730225986738, -1.269999999999999130 ) ) ;
#22017 = CARTESIAN_POINT ( 'NONE',  ( -57.55343345497419705, 2.880119995625998630, 1.988856187846569146 ) ) ;
#22018 = CARTESIAN_POINT ( 'NONE',  ( -50.74065386479207262, 15.09046855081605898, 4.756941196807721539 ) ) ;
#22019 = CARTESIAN_POINT ( 'NONE',  ( -7.954217475012978156, 121.7102781429355076, -1.090678254656372692 ) ) ;
#22020 = AXIS2_PLACEMENT_3D ( 'NONE', #29084, #10124, #15663 ) ;
#22021 = DIRECTION ( 'NONE',  ( 9.627370216492862708E-17, 1.000000000000000000, -0.000000000000000000 ) ) ;
#22022 = CARTESIAN_POINT ( 'NONE',  ( -52.32205026661357294, 13.67230311332622072, 4.407798173677520914 ) ) ;
#22023 = CARTESIAN_POINT ( 'NONE',  ( -9.797860116730056745, 118.0024801742749929, -0.05693907317356646652 ) ) ;
#22024 = ORIENTED_EDGE ( 'NONE', *, *, #21170, .T. ) ;
#22025 = CARTESIAN_POINT ( 'NONE',  ( -50.22242345129090779, 22.76272812237061771, -1.055084478852267100E-14 ) ) ;
#22026 = CARTESIAN_POINT ( 'NONE',  ( 5.965796276062810044, 121.4109386283128771, -0.03877683265643106642 ) ) ;
#22027 = CARTESIAN_POINT ( 'NONE',  ( -7.788361016000392212, 122.6175610729407452, -0.07939682847776179109 ) ) ;
#22028 = ORIENTED_EDGE ( 'NONE', *, *, #6636, .T. ) ;
#22029 = CARTESIAN_POINT ( 'NONE',  ( 1.218872564666173997, 115.7029483217724390, -1.696103018937654028 ) ) ;
#22031 = TOROIDAL_SURFACE ( 'NONE', #3709, 0.7620000000000000107, 0.2540000000000000036 ) ;
#22030 = CARTESIAN_POINT ( 'NONE',  ( -9.288927291931168284, 124.2653519604415067, -0.3477528771403739505 ) ) ;
#22032 = CARTESIAN_POINT ( 'NONE',  ( 5.673176617818914913, -13.06232935199844114, 2.160669506476638357 ) ) ;
#22033 = CARTESIAN_POINT ( 'NONE',  ( -1.132512924677574029, 117.7697124030934077, 0.5521475598058978029 ) ) ;
#22034 = DIRECTION ( 'NONE',  ( 0.6294287539883864913, 0.7770581983690970640, 0.000000000000000000 ) ) ;
#22035 = CARTESIAN_POINT ( 'NONE',  ( 23.30750959433825287, 148.8446908248229477, 0.7975424382754977559 ) ) ;
#22036 = CARTESIAN_POINT ( 'NONE',  ( 15.37822400800898137, 147.8362807140078417, 0.4405641715785962309 ) ) ;
#22037 = CARTESIAN_POINT ( 'NONE',  ( -29.89586364642802963, 71.55302121702176521, 1.523999999999992028 ) ) ;
#22038 = CARTESIAN_POINT ( 'NONE',  ( -0.7839530942921373313, 14.33508526448824760, 0.5845576647881698396 ) ) ;
#22039 = CARTESIAN_POINT ( 'NONE',  ( -0.2950350728690642188, 116.4333835968663919, -0.04389667002116224431 ) ) ;
#22040 = DIRECTION ( 'NONE',  ( 5.206863593109713661E-17, -1.000000000000000000, 1.077750396879097183E-30 ) ) ;
#22041 = CARTESIAN_POINT ( 'NONE',  ( -41.05189575270517821, 23.09451173561986792, -5.652993304041789371E-15 ) ) ;
#22042 = ORIENTED_EDGE ( 'NONE', *, *, #25382, .T. ) ;
#22043 = CARTESIAN_POINT ( 'NONE',  ( 2.276210869248295854, 116.3688137149352571, 0.2778600029539394223 ) ) ;
#22044 = CARTESIAN_POINT ( 'NONE',  ( 3.793251108634954516, -14.54000584982637001, -2.652246991476435056 ) ) ;
#22045 = CARTESIAN_POINT ( 'NONE',  ( 2.096789228655988158, 117.6567184779878232, 0.6641637518095837578 ) ) ;
#22046 = CARTESIAN_POINT ( 'NONE',  ( 6.741493414765732162, 119.3011930948910759, -1.016225879973854607 ) ) ;
#22047 = VECTOR ( 'NONE', #970, 1000.000000000000114 ) ;
#22048 = CARTESIAN_POINT ( 'NONE',  ( -0.4402761300873825334, 6.286315195291644287, -8.460265346311377499 ) ) ;
#22049 = CARTESIAN_POINT ( 'NONE',  ( -1.049200951577276664, 117.3444111807523882, -0.5008604537731422557 ) ) ;
#22050 = CARTESIAN_POINT ( 'NONE',  ( 4.719955967559978482, 117.8401570591244507, -0.8449457312083641369 ) ) ;
#22051 = CARTESIAN_POINT ( 'NONE',  ( 5.245364206137161922, 116.4655405006298849, 1.092799426751067005 ) ) ;
#22052 = CARTESIAN_POINT ( 'NONE',  ( -11.84655969407690534, 151.9972573545839225, -0.1156591128142183539 ) ) ;
#22053 = CARTESIAN_POINT ( 'NONE',  ( -18.91595150393233027, 147.0452383304005082, -2.485053599041413985 ) ) ;
#22054 = EDGE_CURVE ( 'NONE', #35654, #30808, #39391, .T. ) ;
#22055 = CARTESIAN_POINT ( 'NONE',  ( 5.769960013412655186, -14.74427453315851899, 2.495425615322755419 ) ) ;
#22056 = SHAPE_REPRESENTATION ( 'Wing Lever', ( #3275 ), #20939 ) ;
#22057 = CARTESIAN_POINT ( 'NONE',  ( 5.239248437989107110, 115.6909491485453145, 1.024417804751308836 ) ) ;
#22058 = EDGE_CURVE ( 'NONE', #32447, #514, #1338, .T. ) ;
#22059 = FACE_OUTER_BOUND ( 'NONE', #4807, .T. ) ;
#22060 = ORIENTED_EDGE ( 'NONE', *, *, #30810, .T. ) ;
#22061 = CARTESIAN_POINT ( 'NONE',  ( 18.91595150393219882, 147.0452383304005082, 2.485053599041414429 ) ) ;
#22062 = CARTESIAN_POINT ( 'NONE',  ( -17.64950171984354199, 84.16951713491046405, -1.524000000000003130 ) ) ;
#22063 = FACE_OUTER_BOUND ( 'NONE', #31600, .T. ) ;
#22064 = CARTESIAN_POINT ( 'NONE',  ( -0.1065646865916160119, 105.8844662015457061, 5.332932678536314697 ) ) ;
#22065 = CARTESIAN_POINT ( 'NONE',  ( -8.418873817481639321, -10.66996252118913091, -0.4581590610697409693 ) ) ;
#22066 = CARTESIAN_POINT ( 'NONE',  ( 0.6009856513685500889, 120.6441756478195089, 0.2688776736664574285 ) ) ;
#22067 = CARTESIAN_POINT ( 'NONE',  ( 22.18008199020988158, 150.6715983490228723, -0.5179974990882317831 ) ) ;
#22068 = CARTESIAN_POINT ( 'NONE',  ( 4.781529118576645310, 56.51499999999997215, -4.872211946655240489 ) ) ;
#22069 = CARTESIAN_POINT ( 'NONE',  ( -58.36037295411833981, -0.2718383842223853208, 0.1210796893238285932 ) ) ;
#22070 = CARTESIAN_POINT ( 'NONE',  ( -8.795391115079340238, 117.6899447938497048, -0.2513484674950453024 ) ) ;
#22071 = CARTESIAN_POINT ( 'NONE',  ( -5.511275327887647180, 56.51499999999913371, 5.111309966001401861 ) ) ;
#22072 = CARTESIAN_POINT ( 'NONE',  ( -16.31694223957266843, 121.4173703750124531, -0.3260513381110075604 ) ) ;
#22073 = ORIENTED_EDGE ( 'NONE', *, *, #21638, .F. ) ;
#22074 = CARTESIAN_POINT ( 'NONE',  ( -4.450428981627350566, 119.5746151482181148, -0.9239258634587167451 ) ) ;
#22075 = CARTESIAN_POINT ( 'NONE',  ( -5.332935397695335311, 104.6144662015457385, -0.1065647409268299373 ) ) ;
#22076 = CARTESIAN_POINT ( 'NONE',  ( -0.6714861817528541277, 156.3445873232922736, -0.4416347707370365527 ) ) ;
#22077 = CARTESIAN_POINT ( 'NONE',  ( -29.10098582503172082, 61.33321833264426459, 1.523999999999993582 ) ) ;
#22078 = CARTESIAN_POINT ( 'NONE',  ( 21.90516586211584737, 151.4314113202728436, 0.4630247046772880681 ) ) ;
#22079 = ORIENTED_EDGE ( 'NONE', *, *, #37129, .F. ) ;
#22080 = CARTESIAN_POINT ( 'NONE',  ( 2.229080734463354307, 9.364070591990056869, -4.050418370856919914 ) ) ;
#22081 = CARTESIAN_POINT ( 'NONE',  ( -5.314278422745059238, 105.1224610256965235, 0.4583187270701644667 ) ) ;
#22082 = CYLINDRICAL_SURFACE ( 'NONE', #16032, 0.2539999999999989488 ) ;
#22083 = DIRECTION ( 'NONE',  ( -0.8745520943968244643, 0.4849315768086544520, -4.268512490100399076E-16 ) ) ;
#22084 = FACE_OUTER_BOUND ( 'NONE', #37144, .T. ) ;
#22085 = CARTESIAN_POINT ( 'NONE',  ( -6.993440844384329225, 121.9489362634231924, -0.08176518772864471707 ) ) ;
#22086 = FACE_OUTER_BOUND ( 'NONE', #34225, .T. ) ;
#22087 = CARTESIAN_POINT ( 'NONE',  ( 16.15135472115366611, 155.1612327564137388, 1.525667687477715306 ) ) ;
#22088 = CARTESIAN_POINT ( 'NONE',  ( -4.760791928307794407, 104.6144662015457385, -0.8517687557738815585 ) ) ;
#22090 = CARTESIAN_POINT ( 'NONE',  ( 15.16136233027289393, 154.7927800759015042, -1.480671785937533347 ) ) ;
#22089 = CARTESIAN_POINT ( 'NONE',  ( 4.703170801235237342, 114.7515816609199533, 1.852262375087519120 ) ) ;
#22091 = CARTESIAN_POINT ( 'NONE',  ( -10.44084688387123627, 122.0805278159965610, 1.176281030686837425 ) ) ;
#22092 = CARTESIAN_POINT ( 'NONE',  ( 3.308978306493741250, 24.09187545982852541, -3.235542752117448018 ) ) ;
#22093 = CARTESIAN_POINT ( 'NONE',  ( -15.50015290592197381, 121.4967652112180048, -1.085784428920436362 ) ) ;
#22094 = ORIENTED_EDGE ( 'NONE', *, *, #26696, .F. ) ;
#22095 = CARTESIAN_POINT ( 'NONE',  ( -56.89469692534096623, 2.545995565645275960, 0.6470027801917009880 ) ) ;
#22096 = CARTESIAN_POINT ( 'NONE',  ( -15.99817776903328692, 146.0164801329953548, 0.4101439804456899485 ) ) ;
#22097 = CARTESIAN_POINT ( 'NONE',  ( 4.834931622272050866, -13.60668467239417545, 3.655623996717635382 ) ) ;
#22098 = CARTESIAN_POINT ( 'NONE',  ( 17.03734119261599744, 146.7604995623492243, -1.248076303867124093 ) ) ;
#22099 = CARTESIAN_POINT ( 'NONE',  ( -4.845000436079312855, 117.7309513030204613, -0.9913659128643448337 ) ) ;
#22100 = CARTESIAN_POINT ( 'NONE',  ( 10.18105065676961729, 125.9743313966586129, 0.2034416216762105212 ) ) ;
#22102 = EDGE_LOOP ( 'NONE', ( #6773, #12135, #31287, #23840 ) ) ;
#22101 = MECHANICAL_DESIGN_GEOMETRIC_PRESENTATION_REPRESENTATION (  '', ( #41885 ), #31649 ) ;
#22103 = CARTESIAN_POINT ( 'NONE',  ( 18.46656456646925548, 135.7714211226372640, 2.417028963773544259 ) ) ;
#22104 = CARTESIAN_POINT ( 'NONE',  ( 14.67500508080551924, 148.8517222229471315, 0.2932415260855780748 ) ) ;
#22105 = LINE ( 'NONE', #12542, #5521 ) ;
#22106 = CARTESIAN_POINT ( 'NONE',  ( 4.921840205057578466, 117.4109437077822946, -0.9481957113721782848 ) ) ;
#22107 = CARTESIAN_POINT ( 'NONE',  ( 15.11282490002045087, 156.1437908837410191, -0.09152821140687288082 ) ) ;
#22108 = DIRECTION ( 'NONE',  ( -5.188838149069471174E-16, 1.699382548006136313E-16, 1.000000000000000000 ) ) ;
#22109 = CARTESIAN_POINT ( 'NONE',  ( -6.422645615570758970, 77.88548590848095898, 1.270000000000003570 ) ) ;
#22110 = CARTESIAN_POINT ( 'NONE',  ( -46.60530155212501313, 26.17382724835480445, 0.08466666666665845220 ) ) ;
#22111 = CARTESIAN_POINT ( 'NONE',  ( 1.762577841197611406, -15.17375865732635631, 5.852863657745463577 ) ) ;
#22112 = CARTESIAN_POINT ( 'NONE',  ( -48.08949201794742834, 19.91830422262442468, 5.194343260851632671 ) ) ;
#22113 = DIRECTION ( 'NONE',  ( 0.6294287539884059202, 0.7770581983690814099, 1.945484789722797322E-16 ) ) ;
#22114 = CARTESIAN_POINT ( 'NONE',  ( -4.580516980462806309, 118.0858134742356782, 0.5548273466755001548 ) ) ;
#22115 = B_SPLINE_SURFACE_WITH_KNOTS ( 'NONE', 3, 3, ( 
 ( #37090, #10247, #30473, #1317, #39658, #30263, #7280, #20036, #13660, #1104, #14071, #27075 ),
 ( #1941, #40910, #24919, #11501, #34316, #8531, #37492, #5556, #8316, #21491, #12140, #34106 ),
 ( #40504, #14900, #21081, #27697, #24702, #28111, #21916, #14692, #25132, #31519, #34726, #4933 ),
 ( #27903, #18513, #2363, #15322, #17891, #5145, #11715, #30894, #38135, #18099, #34523, #5349 ),
 ( #40705, #37916, #1528, #11299, #37708, #11927, #37288, #8949, #24283, #18303, #8107, #1734 ),
 ( #15108, #24487, #21287, #8740, #4727, #17679, #31305, #30680, #14484, #27497, #2149, #31102 ),
 ( #41121, #21701, #28329, #41337, #26173, #28745, #22121, #2577, #15538, #32361, #3401, #39178 ),
 ( #12968, #31734, #25961, #15949, #22540, #19355, #9570, #18938, #35567, #35150, #32568, #28946 ),
 ( #38551, #9985, #5975, #3189, #2, #2987, #19149, #16151, #38968, #9778, #41963, #32154 ),
 ( #41548, #6181, #41758, #6385, #16369, #35352, #22745, #18724, #25343, #35776, #12559, #31946 ),
 ( #29155, #12762, #19559, #25751, #6591, #29374, #9364, #38346, #213, #28540, #34946, #13188 ),
 ( #5770, #12355, #2784, #9164, #15740, #38759, #25548, #22327, #846, #4257, #40248, #33008 ),
 ( #7234, #17424, #39394, #20609, #428, #6801, #26602, #35986, #32790, #16800, #33429, #22958 ),
 ( #13819, #23383, #20400, #17220, #39825, #1269, #13611, #3836, #23167, #36201, #26817, #29802 ),
 ( #30216, #23811, #36416, #7022, #10619, #27027, #642, #19990, #39608, #3620, #20194, #1056 ),
 ( #30422, #33219, #4047, #10412, #23601, #16585, #17007, #29594, #36622, #33640, #14226, #30007 ),
 ( #19770, #7442, #14020, #7652, #40035, #27233, #10830, #36833, #4467, #13399, #26387, #10196 ),
 ( #4674, #21034, #24231, #1687, #18249, #28060, #24438, #41071, #7859, #40655, #34266, #37659 ),
 ( #33846, #40861, #27441, #14432, #20820, #11448, #31255, #11880, #2096, #8483, #21439, #37241 ),
 ( #8059, #15061, #1476, #17840, #5094, #40456, #18047, #27642, #37441, #24649, #34056, #30839 ),
 ( #4886, #34468, #14641, #31048, #24869, #11246, #5301, #17632, #8265, #21236, #1887, #14849 ),
 ( #11041, #27854, #11663, #24025, #37041, #30632, #4608, #26538, #32941, #10556, #19924, #16729 ),
 ( #17362, #24162, #14360, #39970, #7372, #4405, #1199, #23741, #27373, #39761, #29940, #7170 ),
 ( #26955, #13755, #3982, #30349, #7794, #20331, #20128, #10760, #10969, #26751, #33154, #779 ) ),
 .UNSPECIFIED., .F., .F., .F.,
 ( 4, 2, 2, 2, 2, 2, 2, 2, 2, 2, 2, 4 ),
 ( 4, 2, 1, 2, 1, 2, 4 ),
 ( 0.000000000000000000, 0.1320084156805522713, 0.1980126235208284069, 0.2640168313611045425, 0.3918685259135502030, 0.4557943731897730055, 0.5197202204659958635, 0.5807706587133798504, 0.6418210969607638372, 0.7639219734555318109, 0.8819609867277659054, 1.000000000000000000 ),
 ( 0.000000000000000000, 0.1250000000000000000, 0.2500000000000000000, 0.5000000000000000000, 0.7500000000000000000, 0.8750000000000000000, 1.000000000000000000 ),
 .UNSPECIFIED. ) ;
#22116 = ORIENTED_EDGE ( 'NONE', *, *, #18922, .T. ) ;
#22117 = ORIENTED_EDGE ( 'NONE', *, *, #29282, .T. ) ;
#22118 = CARTESIAN_POINT ( 'NONE',  ( -2.791966037470495987, 115.6909491485424581, -1.685616604675346908 ) ) ;
#22119 = CARTESIAN_POINT ( 'NONE',  ( 8.388245728505863141, 119.8075375339928854, -1.104450739913065638 ) ) ;
#22120 = CARTESIAN_POINT ( 'NONE',  ( -7.618479139564732883, 124.9344662015457317, -0.1522353441811853947 ) ) ;
#22121 = CARTESIAN_POINT ( 'NONE',  ( 4.783303902122270301, 117.7666275948723893, 1.035273760934583898 ) ) ;
#22122 = CARTESIAN_POINT ( 'NONE',  ( -0.1698098321967818070, 106.7790779034713324, 4.970076682467829521 ) ) ;
#22123 = CARTESIAN_POINT ( 'NONE',  ( 4.560362914109654220, -11.68884639558073069, 0.6953251057713033534 ) ) ;
#22124 = CARTESIAN_POINT ( 'NONE',  ( 5.266289895157169814E-14, 83.56599999999998829, 1.904999999999999805 ) ) ;
#22125 = DIRECTION ( 'NONE',  ( -5.188838149069472160E-16, 1.699382548006136559E-16, 1.000000000000000000 ) ) ;
#22126 = CARTESIAN_POINT ( 'NONE',  ( 5.582679110870555128, 119.7830797108918688, -0.2735363082852447780 ) ) ;
#22127 = CARTESIAN_POINT ( 'NONE',  ( -10.85577430263316145, 123.7747955097422476, -1.451053175688577168 ) ) ;
#22128 = CARTESIAN_POINT ( 'NONE',  ( 0.7910183541139823582, 37.90597915310805632, -1.254447098105976321 ) ) ;
#22129 = CARTESIAN_POINT ( 'NONE',  ( -6.158966240078259879, 30.49883854570459718, 2.286114001711006871 ) ) ;
#22130 = CIRCLE ( 'NONE', #40538, 0.3810000000000000053 ) ;
#22131 = CARTESIAN_POINT ( 'NONE',  ( 3.121479725567877228, 16.06095178295013071, 3.416230322513892137 ) ) ;
#22133 = EDGE_LOOP ( 'NONE', ( #38843, #12509, #18467, #34287 ) ) ;
#22132 = CARTESIAN_POINT ( 'NONE',  ( 18.29650779608093458, 125.1624627582897915, 0.9465853942869046911 ) ) ;
#22134 = CARTESIAN_POINT ( 'NONE',  ( 1.603816410906297341, 104.6144662015457811, -4.552900351846083105 ) ) ;
#22135 = CARTESIAN_POINT ( 'NONE',  ( 3.614876661864775187, -15.45153451277975165, 3.150551394879585132 ) ) ;
#22136 = CARTESIAN_POINT ( 'NONE',  ( -17.50667431346024117, 135.4862447717955547, 1.719380121689204399 ) ) ;
#22137 = CARTESIAN_POINT ( 'NONE',  ( -0.4694259674403166716, 18.92165170904731397, 0.8533247626313392731 ) ) ;
#22138 = CARTESIAN_POINT ( 'NONE',  ( -0.1494942157332288524, 1.595350521021342782, -0.9636992805340545143 ) ) ;
#22139 = ORIENTED_EDGE ( 'NONE', *, *, #15991, .T. ) ;
#22140 = ORIENTED_EDGE ( 'NONE', *, *, #32940, .T. ) ;
#22141 = CARTESIAN_POINT ( 'NONE',  ( -47.85244527695891037, 19.39403540832952544, -5.219971639306605127 ) ) ;
#22142 = CARTESIAN_POINT ( 'NONE',  ( 3.137457178757887988, 117.8122656274855871, 0.9631651297103498433 ) ) ;
#22143 = CARTESIAN_POINT ( 'NONE',  ( -15.86865214134244795, 143.7482200480382346, 0.8098737496861397878 ) ) ;
#22144 = CARTESIAN_POINT ( 'NONE',  ( -11.03183784343237583, 128.0124916018596650, -0.2204423744267034746 ) ) ;
#22145 = CARTESIAN_POINT ( 'NONE',  ( 1.990724735134854262, -15.09768785095407040, 5.370787383207776600 ) ) ;
#22146 = CARTESIAN_POINT ( 'NONE',  ( 10.63443090528964241, 122.8495954190337898, -1.101905667251144250 ) ) ;
#22147 = CARTESIAN_POINT ( 'NONE',  ( -15.45413117217014332, 153.1703808545849483, -2.356132421238607222 ) ) ;
#22148 = CARTESIAN_POINT ( 'NONE',  ( -17.14500000000466784, 71.11999999999886768, 1.269999999999998241 ) ) ;
#22149 = EDGE_CURVE ( 'NONE', #27091, #9260, #29164, .T. ) ;
#22150 = CARTESIAN_POINT ( 'NONE',  ( 8.762167414255284115, 117.8147271796869973, 0.5760304689628181762 ) ) ;
#22151 = CARTESIAN_POINT ( 'NONE',  ( -0.3512404605478313679, 38.00633005727588198, 1.239100654724479167 ) ) ;
#22152 = CARTESIAN_POINT ( 'NONE',  ( 15.85578974452665335, 145.9541952667573810, -0.1379097727432555265 ) ) ;
#22153 = VERTEX_POINT ( 'NONE', #7241 ) ;
#22154 = CARTESIAN_POINT ( 'NONE',  ( -2.546031358067248451, 107.1167599116761124, -4.680030732370826563 ) ) ;
#22155 = DIRECTION ( 'NONE',  ( -0.7548010569845247097, -0.6559537821943284275, -7.865859715776929025E-15 ) ) ;
#22156 = DIRECTION ( 'NONE',  ( -0.1565721916418019999, -0.9876665170007956629, 8.659954811667593930E-17 ) ) ;
#22157 = CARTESIAN_POINT ( 'NONE',  ( -58.62613161866106282, -0.2841797903858078733, 0.3870556671707012786 ) ) ;
#22158 = EDGE_CURVE ( 'NONE', #38242, #22885, #33987, .T. ) ;
#22159 = VECTOR ( 'NONE', #28210, 1000.000000000000114 ) ;
#22160 = CARTESIAN_POINT ( 'NONE',  ( -8.001679540263406665, 18.69059125004590172, 2.668541714186715819 ) ) ;
#22161 = CARTESIAN_POINT ( 'NONE',  ( 12.60153737394475648, 128.4643691153342218, 1.495224527512394985 ) ) ;
#22162 = DIRECTION ( 'NONE',  ( -5.188838149069472160E-16, 1.699382548006136559E-16, 1.000000000000000000 ) ) ;
#22163 = CARTESIAN_POINT ( 'NONE',  ( 0.0007535234281856949918, 116.4338605912342786, -0.03770939363766601798 ) ) ;
#22164 = CARTESIAN_POINT ( 'NONE',  ( -6.897523911742089453, 121.8252198949890186, 0.01845719934638757193 ) ) ;
#22165 = FACE_OUTER_BOUND ( 'NONE', #8815, .T. ) ;
#22166 = CARTESIAN_POINT ( 'NONE',  ( -16.02764313970815735, 80.34763903973272647, -1.524000000000002020 ) ) ;
#22167 = CARTESIAN_POINT ( 'NONE',  ( 13.57054970571769914, 121.9345505566020194, 1.704910367088877221 ) ) ;
#22168 = EDGE_CURVE ( 'NONE', #40141, #38260, #6158, .T. ) ;
#22169 = CARTESIAN_POINT ( 'NONE',  ( 7.658903097349539557, 3.149683656735901671, 3.518291596705641400 ) ) ;
#22170 = CARTESIAN_POINT ( 'NONE',  ( 2.173545817240357003, 116.6950714377704372, -0.3876481791814581634 ) ) ;
#22171 = CARTESIAN_POINT ( 'NONE',  ( -0.3562073053189366845, 119.8383472832136931, -0.7014361403029916175 ) ) ;
#22172 = LINE ( 'NONE', #19823, #10780 ) ;
#22173 = DIRECTION ( 'NONE',  ( 1.000000000000000000, 5.463695987328526437E-16, -6.146657985744592735E-16 ) ) ;
#22174 = CARTESIAN_POINT ( 'NONE',  ( 8.369638709285570854, -11.69152869469262157, 0.7709884470677680346 ) ) ;
#22175 = CARTESIAN_POINT ( 'NONE',  ( 2.723865133717724873, 118.1588879269519197, 0.8291662895598204130 ) ) ;
#22176 = DIRECTION ( 'NONE',  ( -0.8745520943968235761, 0.4849315768086558398, -4.268512490100410909E-16 ) ) ;
#22177 = CARTESIAN_POINT ( 'NONE',  ( 3.187143392547471255, -14.52651900126690876, 3.212499789951002604 ) ) ;
#22178 = EDGE_CURVE ( 'NONE', #41065, #36274, #9499, .T. ) ;
#22179 = CARTESIAN_POINT ( 'NONE',  ( 1.058122102717250934, 124.9344662015457459, 0.02114379780294225672 ) ) ;
#22180 = CARTESIAN_POINT ( 'NONE',  ( -23.00823290520148845, 149.2143936249396461, 0.3942700086401352277 ) ) ;
#22181 = ORIENTED_EDGE ( 'NONE', *, *, #18043, .T. ) ;
#22182 = DIRECTION ( 'NONE',  ( 0.01731298258488817021, -0.9998501190848633202, -2.778415991487942562E-15 ) ) ;
#22183 = EDGE_CURVE ( 'NONE', #11064, #8452, #19997, .T. ) ;
#22184 = ORIENTED_EDGE ( 'NONE', *, *, #31090, .T. ) ;
#22185 = LINE ( 'NONE', #21554, #21957 ) ;
#22186 = CARTESIAN_POINT ( 'NONE',  ( 3.601051898931722395, -15.74651769575186044, 4.782909482641136911 ) ) ;
#22187 = CARTESIAN_POINT ( 'NONE',  ( -9.025716902756052207, 119.5326672034033777, 1.052790416315139144 ) ) ;
#22188 = CARTESIAN_POINT ( 'NONE',  ( 21.68724320794224525, 149.9601031839316079, -1.147785971009648076 ) ) ;
#22189 = CARTESIAN_POINT ( 'NONE',  ( -4.478778176974228309, 3.316883148187759645, 1.141857468124592101 ) ) ;
#22190 = CIRCLE ( 'NONE', #34443, 3.111499999999999932 ) ;
#22191 = CARTESIAN_POINT ( 'NONE',  ( -56.36817218596900148, 4.518355621917047316, -2.583766698011176199 ) ) ;
#22192 = ORIENTED_EDGE ( 'NONE', *, *, #33225, .T. ) ;
#22193 = CARTESIAN_POINT ( 'NONE',  ( -58.44182880578510009, -0.4131463110827765517, -0.3217794782792326447 ) ) ;
#22194 = CIRCLE ( 'NONE', #30393, 12.69999999999999751 ) ;
#22195 = CARTESIAN_POINT ( 'NONE',  ( -0.01386859376762973779, 119.8383472832138779, 0.6940411431075129700 ) ) ;
#22196 = CARTESIAN_POINT ( 'NONE',  ( -19.05000000000000426, 71.11999999999999034, -5.714999999999998082 ) ) ;
#22197 = CARTESIAN_POINT ( 'NONE',  ( -5.207149668175701684, 156.3268443366877989, 1.412139582428342255 ) ) ;
#22198 = DIRECTION ( 'NONE',  ( -5.188838149069472160E-16, 1.699382548006136559E-16, 1.000000000000000000 ) ) ;
#22199 = CARTESIAN_POINT ( 'NONE',  ( 5.055620027408425088, 119.3892302351119810, -0.8859254200104712540 ) ) ;
#22200 = CARTESIAN_POINT ( 'NONE',  ( -21.01875934457266837, 148.7375953542188256, -2.355668865594946926 ) ) ;
#22201 = CARTESIAN_POINT ( 'NONE',  ( -52.06546789126484498, 13.38259882428268632, -4.575081192416392106 ) ) ;
#22202 = CARTESIAN_POINT ( 'NONE',  ( 16.18586682243763875, 146.0959698922748942, -0.6488728679227168117 ) ) ;
#22203 = ORIENTED_EDGE ( 'NONE', *, *, #23185, .T. ) ;
#22204 = CARTESIAN_POINT ( 'NONE',  ( -7.368974454111360650, 120.7277362223577768, -1.240556355415273648 ) ) ;
#22205 = CARTESIAN_POINT ( 'NONE',  ( 2.947576629936649706, -15.31278845794613375, 4.223034005107467515 ) ) ;
#22206 = CARTESIAN_POINT ( 'NONE',  ( -4.237174196529505110, 118.2251025442845673, -0.4770184348334939872 ) ) ;
#22207 = AXIS2_PLACEMENT_3D ( 'NONE', #40732, #18126, #41151 ) ;
#22208 = FACE_OUTER_BOUND ( 'NONE', #20892, .T. ) ;
#22209 = CARTESIAN_POINT ( 'NONE',  ( -4.907998571170089086, 117.7148545784633882, 0.7335003228574443757 ) ) ;
#22210 = CARTESIAN_POINT ( 'NONE',  ( 9.109784082438006081, 121.7740273863187923, 1.385347505406782309 ) ) ;
#22211 = LINE ( 'NONE', #19449, #30763 ) ;
#22212 = COLOUR_RGB ( '', 0.66274510, 0.83137255, 0.94901961) ;
#22213 = CARTESIAN_POINT ( 'NONE',  ( -4.050807963365556930, 30.95410787014092335, -2.229501126309402448 ) ) ;
#22214 = CARTESIAN_POINT ( 'NONE',  ( 5.276193270648691147, 121.3253820001177417, 0.2225082926070589828 ) ) ;
#22215 = CARTESIAN_POINT ( 'NONE',  ( -25.70569512491730180, 74.05161654054386133, 1.269999999999993356 ) ) ;
#22216 = TOROIDAL_SURFACE ( 'NONE', #34509, 5.080000000000005400, 0.5080000000000000071 ) ;
#22219 = EDGE_CURVE ( 'NONE', #25673, #1100, #1436, .T. ) ;
#22218 = ORIENTED_EDGE ( 'NONE', *, *, #26331, .T. ) ;
#22217 = CARTESIAN_POINT ( 'NONE',  ( -47.34044527953909665, 17.31523404052589399, -1.593293138114936891 ) ) ;
#22220 = CARTESIAN_POINT ( 'NONE',  ( -0.2349146782472707473, 117.9394520961335360, 1.402130674019514966 ) ) ;
#22221 = PLANE ( 'NONE',  #33610 ) ;
#22222 = CARTESIAN_POINT ( 'NONE',  ( -53.41021539168369969, 10.36760520877136038, 3.951087388861569405 ) ) ;
#22223 = CARTESIAN_POINT ( 'NONE',  ( -29.88458269572754133, 69.13647124298606172, -1.523999999995101273 ) ) ;
#22224 = CARTESIAN_POINT ( 'NONE',  ( -5.305748947172281405, 53.58606249999999704, -5.247078976224250013 ) ) ;
#22225 = CARTESIAN_POINT ( 'NONE',  ( -57.43227285409300009, 3.226759729073131133, 2.064049688025078488 ) ) ;
#22226 = CARTESIAN_POINT ( 'NONE',  ( -9.784355093145462590, 118.0142902678875885, 0.004515160920743777929 ) ) ;
#22227 = VERTEX_POINT ( 'NONE', #14234 ) ;
#22228 = CARTESIAN_POINT ( 'NONE',  ( -53.04800011033383811, 17.61732480341419915, -0.3294858417196845357 ) ) ;
#22229 = CARTESIAN_POINT ( 'NONE',  ( -6.925176729217432658, 121.9065058997480122, -0.3750947163342890356 ) ) ;
#22230 = ADVANCED_FACE ( 'NONE', ( #21244 ), #4474, .T. ) ;
#22231 = CARTESIAN_POINT ( 'NONE',  ( 4.901772867295396630, 117.4071509163661204, -0.9681717027652592122 ) ) ;
#22232 = VERTEX_POINT ( 'NONE', #8274 ) ;
#22233 = CARTESIAN_POINT ( 'NONE',  ( 2.051901541566586218, 115.7029480913673751, -1.635851152962789934 ) ) ;
#22234 = CARTESIAN_POINT ( 'NONE',  ( -12.91493749300788885, 133.8340822528099636, -0.3749514369420003934 ) ) ;
#22235 = CARTESIAN_POINT ( 'NONE',  ( 2.103176148521523459, -15.33886314497087611, 5.964097425510020756 ) ) ;
#22236 = CARTESIAN_POINT ( 'NONE',  ( -19.06828360855658744, 152.1029585079319020, 1.398049597035978087 ) ) ;
#22237 = DIRECTION ( 'NONE',  ( -0.9336303900108801068, -0.3582377630124047307, 1.771430154111087713E-15 ) ) ;
#22238 = CARTESIAN_POINT ( 'NONE',  ( 20.65160272637281480, 152.5811724025633112, 0.7328296130731980496 ) ) ;
#22239 = AXIS2_PLACEMENT_3D ( 'NONE', #28451, #29073, #16283 ) ;
#22240 = ADVANCED_FACE ( 'NONE', ( #30223 ), #7165, .T. ) ;
#22241 = CARTESIAN_POINT ( 'NONE',  ( 7.992875830012473592, 122.8474187487093872, 0.2833331899898612893 ) ) ;
#22242 = CARTESIAN_POINT ( 'NONE',  ( 17.14499999999999957, 71.11999999999999034, 5.016499999999999737 ) ) ;
#22243 = CARTESIAN_POINT ( 'NONE',  ( -0.9731698936423014423, 13.46246454747003618, 0.06867709314994872860 ) ) ;
#22244 = CARTESIAN_POINT ( 'NONE',  ( 0.001319893060087149817, 116.4580521601689185, -0.06605284600166357045 ) ) ;
#22245 = CARTESIAN_POINT ( 'NONE',  ( -5.586884702347497900, 123.6644662015457214, -0.1116392523995361624 ) ) ;
#22246 = CARTESIAN_POINT ( 'NONE',  ( -3.630816577625875226E-14, 57.14999999999999147, 0.000000000000000000 ) ) ;
#22247 = ORIENTED_EDGE ( 'NONE', *, *, #11287, .F. ) ;
#22248 = CARTESIAN_POINT ( 'NONE',  ( -2.788466383568154239, 117.1109391571273619, 0.5482988353915653201 ) ) ;
#22249 = ORIENTED_EDGE ( 'NONE', *, *, #3477, .F. ) ;
#22250 = CARTESIAN_POINT ( 'NONE',  ( -58.36579948110144045, -0.2832072201896413954, -0.07825354645670587472 ) ) ;
#22251 = CARTESIAN_POINT ( 'NONE',  ( 21.43631064271305320, 148.9071063441643048, 2.241374363660425750 ) ) ;
#22252 = CARTESIAN_POINT ( 'NONE',  ( 20.17069300908746854, 147.5185649274072830, -1.704009200980389771 ) ) ;
#22253 = CARTESIAN_POINT ( 'NONE',  ( 7.425401986171529245, 12.64277321918224040, 4.020893088955488359 ) ) ;
#22254 = EDGE_CURVE ( 'NONE', #19060, #26787, #2534, .T. ) ;
#22255 = CARTESIAN_POINT ( 'NONE',  ( -14.80859988127097715, 121.7713424311148032, -1.438396347550856991 ) ) ;
#22256 = CARTESIAN_POINT ( 'NONE',  ( 4.817834478233289808, 117.8426053691435840, -0.7486223446464784770 ) ) ;
#22257 = CARTESIAN_POINT ( 'NONE',  ( 7.136594729663718439, 122.4194348751405101, 0.2521576392032937597 ) ) ;
#22258 = CIRCLE ( 'NONE', #31022, 2.540000000000000480 ) ;
#22259 = CARTESIAN_POINT ( 'NONE',  ( -14.20283082469480007, 138.9094276006951247, -0.1579304324436907880 ) ) ;
#22260 = CARTESIAN_POINT ( 'NONE',  ( -13.34589015847600102, 154.0568829568526041, -2.281985820853443592 ) ) ;
#22261 = CARTESIAN_POINT ( 'NONE',  ( 3.172349117095228710, -15.63690262102951323, 5.390679387232247599 ) ) ;
#22262 = DIRECTION ( 'NONE',  ( -5.188838149069472160E-16, 1.699382548006136559E-16, 1.000000000000000000 ) ) ;
#22263 = CARTESIAN_POINT ( 'NONE',  ( -45.14658554404967106, 22.88857079803865346, -2.562886992506571371 ) ) ;
#22264 = B_SPLINE_CURVE_WITH_KNOTS ( 'NONE', 3,
 ( #23467, #36494, #7313, #16883, #32450, #35659, #16669, #33302, #29884, #3282, #23256, #20273, #26477, #35869, #17090, #22623, #39059, #16243, #30092, #10286, #12851, #6894, #25837, #91, #517, #722, #32663, #9862, #304, #13056, #19862, #22833, #32878, #36290 ),
 .UNSPECIFIED., .F., .F.,
 ( 4, 2, 2, 2, 2, 2, 2, 2, 2, 2, 2, 2, 2, 2, 2, 2, 4 ),
 ( 0.01745000530654042953, 0.01846956716767890472, 0.01948912902881738338, 0.02050869088995585857, 0.02152825275109433376, 0.02356737647337128760, 0.02458693833450976279, 0.02560650019564823798, 0.02662606205678671317, 0.02764562391792518836, 0.02866518577906366355, 0.02917496670963290462, 0.02968474764020214221, 0.03070430950134062087, 0.03172387136247909606, 0.03274343322361757125, 0.03376299508475605338 ),
 .UNSPECIFIED. ) ;
#22265 = ORIENTED_EDGE ( 'NONE', *, *, #1230, .F. ) ;
#22266 = CARTESIAN_POINT ( 'NONE',  ( 16.04699077284479003, 131.4332636412663931, 2.269269673164717283 ) ) ;
#22267 = CARTESIAN_POINT ( 'NONE',  ( 2.666490510518176649, -13.49855353256042712, 0.05227394649444803282 ) ) ;
#22268 = DIRECTION ( 'NONE',  ( -0.8745520943968243532, 0.4849315768086547296, -6.829619984160642269E-16 ) ) ;
#22269 = AXIS2_PLACEMENT_3D ( 'NONE', #16551, #17184, #30183 ) ;
#22270 = CARTESIAN_POINT ( 'NONE',  ( -1.209846520933468339, 108.5039085404744981, 4.223631676023018144 ) ) ;
#22271 = CARTESIAN_POINT ( 'NONE',  ( -4.342437030201590886, 23.60747082334219371, 7.218840658967335067 ) ) ;
#22272 = CARTESIAN_POINT ( 'NONE',  ( 15.99655225346408649, 147.0154580547469152, 1.170958206671064206 ) ) ;
#22273 = CARTESIAN_POINT ( 'NONE',  ( 14.76838793310957421, 156.1040168620350244, -0.6600470674582793462 ) ) ;
#22274 = LINE ( 'NONE', #42121, #9069 ) ;
#22275 = CARTESIAN_POINT ( 'NONE',  ( -58.36935479428260010, -0.2906258791830944599, 0.02610806206428318774 ) ) ;
#22276 = CARTESIAN_POINT ( 'NONE',  ( -0.8838529761741459323, 116.4325158421065680, -0.01766148591713742610 ) ) ;
#22277 = ORIENTED_EDGE ( 'NONE', *, *, #8685, .F. ) ;
#22278 = CARTESIAN_POINT ( 'NONE',  ( 6.353751754745901259, 119.9757864133673735, -0.9602761413627547427 ) ) ;
#22279 = CARTESIAN_POINT ( 'NONE',  ( -23.94760723868026631, 77.08694321397520355, -1.524000000000005350 ) ) ;
#22280 = CARTESIAN_POINT ( 'NONE',  ( -4.372087114477377412, 155.8497297829079571, -0.6179351164228050752 ) ) ;
#22281 = CARTESIAN_POINT ( 'NONE',  ( 6.059261036833978764, 78.87450423423040036, 5.016499999999999737 ) ) ;
#22282 = CARTESIAN_POINT ( 'NONE',  ( 21.67415503129002019, 132.7302833492884417, 0.4548691923922799640 ) ) ;
#22283 = ADVANCED_FACE ( 'NONE', ( #38509 ), #41712, .T. ) ;
#22284 = EDGE_LOOP ( 'NONE', ( #31498, #13691, #13583, #10784 ) ) ;
#22285 = CARTESIAN_POINT ( 'NONE',  ( -0.5093740622119584671, 14.76157059199007016, 4.595130897425484306 ) ) ;
#22286 = CARTESIAN_POINT ( 'NONE',  ( -29.20122892428398487, 63.96733531828105157, 1.523999999999130495 ) ) ;
#22287 = CARTESIAN_POINT ( 'NONE',  ( -4.854959790655453133, 117.4058051295649534, 0.9982048359480585331 ) ) ;
#22288 = CARTESIAN_POINT ( 'NONE',  ( -43.16005656664477641, 21.89413631511959579, 2.197846903551415654 ) ) ;
#22289 = CARTESIAN_POINT ( 'NONE',  ( -3.174366308152011928, 76.29346620154572634, -0.06343139340882730792 ) ) ;
#22290 = CARTESIAN_POINT ( 'NONE',  ( -7.988165842219651758, 121.7257876813687858, 0.7681561951654892750 ) ) ;
#22291 =( BOUNDED_CURVE ( )  B_SPLINE_CURVE ( 2, ( #18814, #31823, #27575 ),
 .UNSPECIFIED., .F., .T. ) 
 B_SPLINE_CURVE_WITH_KNOTS ( ( 3, 3 ),
 ( 0.000000000000000000, 1.000000000000000000 ),
 .UNSPECIFIED. ) 
 CURVE ( )  GEOMETRIC_REPRESENTATION_ITEM ( )  RATIONAL_B_SPLINE_CURVE ( ( 1.000000000000000000, 0.9987193938133603899, 1.000000000000000000 ) ) 
 REPRESENTATION_ITEM ( '' )  );
#22292 = CARTESIAN_POINT ( 'NONE',  ( 0.4327634382839667393, 5.975216699623356220, -4.620561613140377055 ) ) ;
#22293 = CARTESIAN_POINT ( 'NONE',  ( 17.90421410101168576, 154.0540368679750998, 1.594113676345344954 ) ) ;
#22294 = CARTESIAN_POINT ( 'NONE',  ( -52.02227077090995522, 12.92666902011463392, -4.429676403366612725 ) ) ;
#22296 = CARTESIAN_POINT ( 'NONE',  ( 6.947343058555276230, 158.0090104422344268, -1.506406725519187972 ) ) ;
#22295 = CARTESIAN_POINT ( 'NONE',  ( 5.177913976931197482, 56.51500000000002188, 5.372099999999984554 ) ) ;
#22297 = CARTESIAN_POINT ( 'NONE',  ( -3.394752741017290631, 119.5845705363850442, 0.6980748167159184225 ) ) ;
#22298 = CARTESIAN_POINT ( 'NONE',  ( 4.198131962423935271, 12.64715247731088787, 1.959332076845688553 ) ) ;
#22299 = CARTESIAN_POINT ( 'NONE',  ( -16.47501798513129145, 155.2380866766625047, -1.211716152346587361 ) ) ;
#22300 = MECHANICAL_DESIGN_GEOMETRIC_PRESENTATION_REPRESENTATION (  '', ( #28430 ), #19562 ) ;
#22301 = ORIENTED_EDGE ( 'NONE', *, *, #19123, .F. ) ;
#22302 = CARTESIAN_POINT ( 'NONE',  ( -0.003756957834544885893, 120.7746249494737896, 0.1880135328902414193 ) ) ;
#22303 = CARTESIAN_POINT ( 'NONE',  ( 4.135482704272881449, -14.73569165307708673, 5.015242562682193039 ) ) ;
#22304 = DIRECTION ( 'NONE',  ( -0.9998004120163609398, 0.000000000000000000, -0.01997839162482749689 ) ) ;
#22305 = CARTESIAN_POINT ( 'NONE',  ( -4.661795382597888171, 117.9824458133873861, -0.8615256122207085587 ) ) ;
#22306 = CARTESIAN_POINT ( 'NONE',  ( 14.16569067496505774, 138.8670163227233161, 0.2830642121559648339 ) ) ;
#22307 = ORIENTED_EDGE ( 'NONE', *, *, #34392, .F. ) ;
#22308 = CARTESIAN_POINT ( 'NONE',  ( 18.80649797369231280, 150.3568762430427910, 2.459390564378663768 ) ) ;
#22309 = CYLINDRICAL_SURFACE ( 'NONE', #9971, 0.6349999999999966782 ) ;
#22310 = CARTESIAN_POINT ( 'NONE',  ( 7.784012320830338005, 122.6313477005580665, 0.1555430910899518460 ) ) ;
#22311 = CARTESIAN_POINT ( 'NONE',  ( -0.01289612358334801118, 159.5048567107479585, 0.6453747585945883714 ) ) ;
#22312 = CARTESIAN_POINT ( 'NONE',  ( 4.812211268859890367, 117.4735958283970234, -1.001561189053170153 ) ) ;
#22313 = CARTESIAN_POINT ( 'NONE',  ( 4.773421586889285528, 116.8420656028321218, -0.1264526730306985980 ) ) ;
#22314 = CARTESIAN_POINT ( 'NONE',  ( -12.21488373878702127, 55.49440886859295574, 5.016499999999999737 ) ) ;
#22315 = CARTESIAN_POINT ( 'NONE',  ( -42.72397600927682504, 22.83316142988638831, 1.683267422954620063 ) ) ;
#22316 = CARTESIAN_POINT ( 'NONE',  ( -46.81005371095113077, 25.73327194510126859, 1.583310528698469222 ) ) ;
#22317 = CARTESIAN_POINT ( 'NONE',  ( 1.961397211334666046, -15.23659401288117365, 5.381129598871191355 ) ) ;
#22318 = CARTESIAN_POINT ( 'NONE',  ( -48.53848336910535011, 19.22582880449973075, 5.323527254358031868 ) ) ;
#22319 = CARTESIAN_POINT ( 'NONE',  ( -58.67289155984229865, -0.3138610667730852843, 0.3158150924223985800 ) ) ;
#22320 = CARTESIAN_POINT ( 'NONE',  ( -4.567146515290242625, 118.0741377463749160, 0.6112040792829432911 ) ) ;
#22321 = ORIENTED_EDGE ( 'NONE', *, *, #15211, .T. ) ;
#22322 = VERTEX_POINT ( 'NONE', #12518 ) ;
#22323 = CARTESIAN_POINT ( 'NONE',  ( -5.177913976931285411, 57.14999999999998437, 5.372100000000002318 ) ) ;
#22324 = AXIS2_PLACEMENT_3D ( 'NONE', #38017, #28426, #28847 ) ;
#22325 = CARTESIAN_POINT ( 'NONE',  ( 5.944196296451716321, 119.0874165451813695, -1.025244264899787483 ) ) ;
#22326 = CARTESIAN_POINT ( 'NONE',  ( -4.757567707637590182, 116.6039038697339549, -1.126183464948452562 ) ) ;
#22327 = CARTESIAN_POINT ( 'NONE',  ( 4.589873572828570225, 118.0230325535246010, 0.8585248486873602314 ) ) ;
#22328 = AXIS2_PLACEMENT_3D ( 'NONE', #22242, #25872, #35905 ) ;
#22329 = CARTESIAN_POINT ( 'NONE',  ( 2.350639260211558668, -15.10312717587823705, 4.966175652281853203 ) ) ;
#22330 = CARTESIAN_POINT ( 'NONE',  ( -3.199116795994628948, 156.2293907256693331, -0.9954876105832137778 ) ) ;
#22331 = CARTESIAN_POINT ( 'NONE',  ( -2.393320966970525987, 115.7029491485454002, -1.700712295284147579 ) ) ;
#22332 = CARTESIAN_POINT ( 'NONE',  ( -0.3678760602612873298, 105.9882361710916427, 5.283425915285953067 ) ) ;
#22333 = FACE_OUTER_BOUND ( 'NONE', #4906, .T. ) ;
#22334 = CARTESIAN_POINT ( 'NONE',  ( 2.668012146925189398, 107.2306503360107541, -4.624472725681509466 ) ) ;
#22335 = CARTESIAN_POINT ( 'NONE',  ( -13.40752216115205542, 152.3772590505219569, -2.011877943007317704 ) ) ;
#22336 = DIRECTION ( 'NONE',  ( 0.3582377630123966261, -0.9336303900108832154, 0.000000000000000000 ) ) ;
#22337 = CARTESIAN_POINT ( 'NONE',  ( -4.259326390738950252, 31.70363750509472212, 4.262602491460973475 ) ) ;
#22338 = CARTESIAN_POINT ( 'NONE',  ( -3.636814527154180521, 115.7029495058465045, 1.480691701714403452 ) ) ;
#22339 = CARTESIAN_POINT ( 'NONE',  ( 3.700881553190929374, 8.714383148187751615, -2.768892949411812854 ) ) ;
#22341 = ORIENTED_EDGE ( 'NONE', *, *, #30040, .F. ) ;
#22340 = CARTESIAN_POINT ( 'NONE',  ( 5.580240031299299908, 159.0849926622337023, 0.6989143883095926268 ) ) ;
#22342 = CARTESIAN_POINT ( 'NONE',  ( 4.210806622510559372, 104.6144662015456817, -2.365042981711354297 ) ) ;
#22343 = CARTESIAN_POINT ( 'NONE',  ( 3.487342509456591522, -15.13654059619573644, 2.575171134517089566 ) ) ;
#22344 = CARTESIAN_POINT ( 'NONE',  ( -19.58589350844871291, 147.2819018089465715, 1.740056086200069796 ) ) ;
#22345 = CARTESIAN_POINT ( 'NONE',  ( 0.7587898337924254832, 1.856531735440085207, 0.6142162870750064174 ) ) ;
#22346 = CARTESIAN_POINT ( 'NONE',  ( 0.5069063945870452281, 6.992850521020996801, 0.8331330811856124674 ) ) ;
#22347 = ORIENTED_EDGE ( 'NONE', *, *, #20088, .T. ) ;
#22348 = ORIENTED_EDGE ( 'NONE', *, *, #26444, .F. ) ;
#22349 = FACE_OUTER_BOUND ( 'NONE', #15492, .T. ) ;
#22350 = CARTESIAN_POINT ( 'NONE',  ( 1.726955742647716674, 108.8931014686503289, 4.100893600158903141 ) ) ;
#22351 = CARTESIAN_POINT ( 'NONE',  ( -3.602148172789818581, 120.6468399921648711, 0.3585086490597838016 ) ) ;
#22352 = CARTESIAN_POINT ( 'NONE',  ( -10.18105065676974519, 125.9743313966586129, -0.2034416216762104657 ) ) ;
#22353 = CARTESIAN_POINT ( 'NONE',  ( 2.851896361732738860, -14.59419570037479019, 4.638016276237491020 ) ) ;
#22354 = CARTESIAN_POINT ( 'NONE',  ( 3.432158483474355037, 119.7942873563901713, -0.6544105580379840914 ) ) ;
#22355 = CARTESIAN_POINT ( 'NONE',  ( -19.66043293732255748, 148.5147687316951135, -2.511426770373370587 ) ) ;
#22356 = CARTESIAN_POINT ( 'NONE',  ( -48.27157819694446061, 19.62644098948943494, -5.255994444853051561 ) ) ;
#22357 = CARTESIAN_POINT ( 'NONE',  ( -2.948382749353948729, 50.63946620154572997, -1.837270642369388307 ) ) ;
#22358 = CARTESIAN_POINT ( 'NONE',  ( -4.834131565410835663, 32.86531471714831554, 2.080611622871570088 ) ) ;
#22359 = CARTESIAN_POINT ( 'NONE',  ( 13.12764272666522558, 133.9996589410087324, -0.1750096343312397829 ) ) ;
#22360 = ORIENTED_EDGE ( 'NONE', *, *, #41501, .T. ) ;
#22361 = DIRECTION ( 'NONE',  ( -0.000000000000000000, -0.000000000000000000, -1.000000000000000000 ) ) ;
#22362 = AXIS2_PLACEMENT_3D ( 'NONE', #33587, #39558, #794 ) ;
#22363 = DIRECTION ( 'NONE',  ( -0.2883665106726556182, -0.9575201071113218498, -1.655452583021194521E-15 ) ) ;
#22364 = CARTESIAN_POINT ( 'NONE',  ( 4.889213426004227259, 117.7581299865985471, -0.6851927402696675884 ) ) ;
#22365 = CARTESIAN_POINT ( 'NONE',  ( 0.7350785369229140276, 15.66647056970591301, -8.407117359194836936 ) ) ;
#22366 = CARTESIAN_POINT ( 'NONE',  ( 7.769844292199929114, 122.1031240515655298, 0.8163738826679364236 ) ) ;
#22367 = DIRECTION ( 'NONE',  ( 4.017660918040594346E-17, -1.000000000000000000, -2.376309959284834438E-19 ) ) ;
#22368 = CARTESIAN_POINT ( 'NONE',  ( 20.50175740331280139, 129.0975500345852822, 0.3894088793431775830 ) ) ;
#22369 = EDGE_CURVE ( 'NONE', #21980, #35923, #38745, .T. ) ;
#22370 = CARTESIAN_POINT ( 'NONE',  ( -5.267339127473358751, 116.4790307410953289, 0.8814195561379957189 ) ) ;
#22371 = CARTESIAN_POINT ( 'NONE',  ( -15.27962295839633811, 80.49293118800726177, 1.269999999999997797 ) ) ;
#22372 = CARTESIAN_POINT ( 'NONE',  ( -3.178183004559932190, -7.902942162671289239, -3.366045245292264010 ) ) ;
#22373 = CARTESIAN_POINT ( 'NONE',  ( -0.09153888643297225514, 38.16702564188061331, -1.140315812098650960 ) ) ;
#22374 = CARTESIAN_POINT ( 'NONE',  ( 20.51891680819867503, 149.8464234248869786, 2.337676305755668871 ) ) ;
#22375 = CARTESIAN_POINT ( 'NONE',  ( 8.184481992144968743, -14.99546276350015717, -2.142971516962156819 ) ) ;
#22376 = CARTESIAN_POINT ( 'NONE',  ( -5.482088966821565990, 117.2431503203738714, -0.8245388645859690335 ) ) ;
#22377 = CARTESIAN_POINT ( 'NONE',  ( -0.3576380314658750836, 120.7331730230137623, -0.5311352847986057224 ) ) ;
#22378 = DIRECTION ( 'NONE',  ( 5.188838149069472160E-16, -1.699382548006136559E-16, -1.000000000000000000 ) ) ;
#22379 = CARTESIAN_POINT ( 'NONE',  ( -10.92199999999999704, 55.24499999999999034, 0.000000000000000000 ) ) ;
#22380 = CARTESIAN_POINT ( 'NONE',  ( -3.947475993436067920, 104.6144662015413616, 3.604255196807834682 ) ) ;
#22381 = ADVANCED_BREP_SHAPE_REPRESENTATION ( '', ( #38535, #3275 ), #21588 ) ;
#22382 = CARTESIAN_POINT ( 'NONE',  ( -2.201963191602333225, 30.07953629247752758, -4.075912811544394998 ) ) ;
#22383 = CARTESIAN_POINT ( 'NONE',  ( -11.58677707360137532, 55.98894877578615592, -4.474811398758257397 ) ) ;
#22384 = CARTESIAN_POINT ( 'NONE',  ( 2.958531772299236362, 39.20946620154573736, 1.329372033065076453 ) ) ;
#22385 = CARTESIAN_POINT ( 'NONE',  ( 1.854781166956293248, -15.20994639552496253, 5.427130820981656001 ) ) ;
#22386 = EDGE_CURVE ( 'NONE', #29922, #39604, #5644, .T. ) ;
#22387 = CARTESIAN_POINT ( 'NONE',  ( 1.590100404673003398, 118.0223913815010377, -0.9765506547304492191 ) ) ;
#22388 = CARTESIAN_POINT ( 'NONE',  ( -5.848384816632850480, 117.2350771734024164, 0.3616545339607749043 ) ) ;
#22389 = CIRCLE ( 'NONE', #23096, 0.5080000000000000071 ) ;
#22390 = ORIENTED_EDGE ( 'NONE', *, *, #27142, .T. ) ;
#22391 = DIRECTION ( 'NONE',  ( -5.188838149069472160E-16, 1.699382548006136559E-16, 1.000000000000000000 ) ) ;
#22392 = VECTOR ( 'NONE', #2944, 1000.000000000000000 ) ;
#22393 = ORIENTED_EDGE ( 'NONE', *, *, #13864, .T. ) ;
#22394 = PLANE ( 'NONE',  #26722 ) ;
#22395 = CARTESIAN_POINT ( 'NONE',  ( 2.745816630209086728, -15.73397280162352985, 5.435574744647863277 ) ) ;
#22396 = CARTESIAN_POINT ( 'NONE',  ( -11.63724909022846177, 121.0393782313542346, 1.189926691809807036 ) ) ;
#22397 = CARTESIAN_POINT ( 'NONE',  ( 22.03832501185533488, 149.1257232373000647, -1.146528549967842148 ) ) ;
#22398 = CARTESIAN_POINT ( 'NONE',  ( 1.719524320724281852, 5.915668354077112667, 4.300554535892874064 ) ) ;
#22399 = CARTESIAN_POINT ( 'NONE',  ( -57.60174957807323892, 1.918618717652168737, -1.731152311951061229 ) ) ;
#22400 = ORIENTED_EDGE ( 'NONE', *, *, #24581, .F. ) ;
#22401 = CARTESIAN_POINT ( 'NONE',  ( -58.34279097978634354, -0.2008976519087390666, -0.5874393231861719800 ) ) ;
#22402 = CARTESIAN_POINT ( 'NONE',  ( -0.1041500444723911512, 106.1822392402443143, 5.212094112990278028 ) ) ;
#22403 = CARTESIAN_POINT ( 'NONE',  ( 8.689997779576109740E-16, 9.026346327358515609, 0.000000000000000000 ) ) ;
#22404 = CARTESIAN_POINT ( 'NONE',  ( -14.44833386134795283, 131.1674235819977241, 1.369607862251506658 ) ) ;
#22405 = DIRECTION ( 'NONE',  ( -0.8745520943968240202, 0.4849315768086553402, -5.361993529360572958E-16 ) ) ;
#22406 = CARTESIAN_POINT ( 'NONE',  ( 0.5101717508067669105, 119.1670848682014281, -0.5756831679880033414 ) ) ;
#22407 = CARTESIAN_POINT ( 'NONE',  ( -9.341440546823601920, 157.3305555497073271, -1.901068499721874971 ) ) ;
#22408 = CARTESIAN_POINT ( 'NONE',  ( -5.177913976931298734, 78.94499979771843812, 5.372100000000002318 ) ) ;
#22409 = ORIENTED_EDGE ( 'NONE', *, *, #17977, .T. ) ;
#22410 = CARTESIAN_POINT ( 'NONE',  ( 16.19917940306794790, 146.4165046419237228, -0.6472847106673340623 ) ) ;
#22411 = ORIENTED_EDGE ( 'NONE', *, *, #21198, .F. ) ;
#22412 = CARTESIAN_POINT ( 'NONE',  ( -0.5205939700077546473, 119.6443647996702566, -0.5336935438815135768 ) ) ;
#22413 = CARTESIAN_POINT ( 'NONE',  ( 2.733372102295486439, -15.34075898222114809, 4.536119796583970576 ) ) ;
#22414 = CARTESIAN_POINT ( 'NONE',  ( -4.242447431898493271, 118.2250608216800032, -0.4715757167317731202 ) ) ;
#22415 = ADVANCED_FACE ( 'NONE', ( #5729 ), #18259, .T. ) ;
#22416 = DIRECTION ( 'NONE',  ( 0.9998004120163608288, 0.000000000000000000, 0.01997839162482749342 ) ) ;
#22417 = VECTOR ( 'NONE', #18553, 1000.000000000000114 ) ;
#22418 = CARTESIAN_POINT ( 'NONE',  ( -4.815137252779631893, 117.6728645535923903, 0.9184442549704321390 ) ) ;
#22419 = CARTESIAN_POINT ( 'NONE',  ( 5.840731033150115437, 120.5744318282211651, 0.9509518217554208119 ) ) ;
#22420 = CARTESIAN_POINT ( 'NONE',  ( -46.72577905453591285, 25.95655153957432049, 1.270000040520065099 ) ) ;
#22421 = CARTESIAN_POINT ( 'NONE',  ( -4.420329592304260480, 21.65838872207745425, -1.398650104627336743 ) ) ;
#22422 = CARTESIAN_POINT ( 'NONE',  ( 2.787004648571185683, 120.9517662584847102, 0.1965090384792946565 ) ) ;
#22423 = DIRECTION ( 'NONE',  ( -0.9336303900108815501, -0.3582377630124009560, -4.235673982319039874E-16 ) ) ;
#22425 = ORIENTED_EDGE ( 'NONE', *, *, #31016, .T. ) ;
#22424 = CARTESIAN_POINT ( 'NONE',  ( -49.96466797210978683, 13.31430344189337589, -0.7651684107025076287 ) ) ;
#22426 = CARTESIAN_POINT ( 'NONE',  ( -11.66725022231030984, 16.50999999999999801, -5.016499999999999737 ) ) ;
#22427 = DIRECTION ( 'NONE',  ( -0.000000000000000000, -0.000000000000000000, -1.000000000000000000 ) ) ;
#22428 = CARTESIAN_POINT ( 'NONE',  ( -55.32540223338650520, 6.651447249606684764, 3.145907943678666996 ) ) ;
#22429 = CARTESIAN_POINT ( 'NONE',  ( -8.255892650435239233, 120.2042668886316505, -1.447829519518265551 ) ) ;
#22430 = CARTESIAN_POINT ( 'NONE',  ( -26.07365872405947727, 72.73903180058835005, 1.269999999999993356 ) ) ;
#22431 = CARTESIAN_POINT ( 'NONE',  ( -54.68491514712287227, 9.937145987696780480, 2.757516356780029820 ) ) ;
#22432 = CARTESIAN_POINT ( 'NONE',  ( -23.31467963135047583, 142.7201128741078833, -0.1336249016415856083 ) ) ;
#22433 = VERTEX_POINT ( 'NONE', #28069 ) ;
#22434 = CARTESIAN_POINT ( 'NONE',  ( -51.68405183839315242, 20.46365084185837446, -0.3671080129529064595 ) ) ;
#22435 = CARTESIAN_POINT ( 'NONE',  ( -5.947743514043456692, 121.4056990298405339, -0.2736948476934324970 ) ) ;
#22436 = VERTEX_POINT ( 'NONE', #2320 ) ;
#22437 = CARTESIAN_POINT ( 'NONE',  ( 0.7498611054318164992, 115.7030496223163567, -1.729246923944893322 ) ) ;
#22439 = CARTESIAN_POINT ( 'NONE',  ( -7.814053207648073318, 154.6216606121152495, -0.3474563751001364942 ) ) ;
#22438 = VECTOR ( 'NONE', #30244, 1000.000000000000000 ) ;
#22440 = CARTESIAN_POINT ( 'NONE',  ( 4.669346286639404653, -14.72966438191931893, 4.552848284282712044 ) ) ;
#22441 = CARTESIAN_POINT ( 'NONE',  ( -13.91986491619295663, 121.5005676099359846, 1.010465608187345321 ) ) ;
#22442 = CARTESIAN_POINT ( 'NONE',  ( 5.714078020757473730, 78.90256189635211115, -5.042866571093843397 ) ) ;
#22443 = CARTESIAN_POINT ( 'NONE',  ( 23.40831777029523053, 146.8136392739129974, 0.6999192077533369361 ) ) ;
#22444 = CARTESIAN_POINT ( 'NONE',  ( 2.854181719429574215, 121.0288205536620580, 0.1255016766574598708 ) ) ;
#22445 = CARTESIAN_POINT ( 'NONE',  ( 4.765727645999143114, 118.5266822147775940, -0.8411891241973677991 ) ) ;
#22446 = CARTESIAN_POINT ( 'NONE',  ( -0.8857237343455648393, 3.096269703755229141, -0.4102451188256627801 ) ) ;
#22447 = CARTESIAN_POINT ( 'NONE',  ( -21.89464077100150163, 151.4392833230981239, -0.5893027811483438905 ) ) ;
#22448 = DIRECTION ( 'NONE',  ( 0.000000000000000000, 0.000000000000000000, 1.000000000000000000 ) ) ;
#22449 = EDGE_CURVE ( 'NONE', #10681, #9538, #5935, .T. ) ;
#22450 = CYLINDRICAL_SURFACE ( 'NONE', #1675, 0.6350000000000001199 ) ;
#22451 = VERTEX_POINT ( 'NONE', #9121 ) ;
#22452 = CARTESIAN_POINT ( 'NONE',  ( -2.376166872315972345, 116.5345204588131480, 0.3007191275596990954 ) ) ;
#22453 = ORIENTED_EDGE ( 'NONE', *, *, #6035, .F. ) ;
#22454 = CARTESIAN_POINT ( 'NONE',  ( -58.33566222542154378, -0.2199106620376253540, -0.2319731289860410273 ) ) ;
#22455 = CARTESIAN_POINT ( 'NONE',  ( 12.23848595143944351, 156.6574886424908470, 1.779988832801368659 ) ) ;
#22456 = CARTESIAN_POINT ( 'NONE',  ( 12.70950188986275187, 122.0451665396574725, -1.271450951352564251 ) ) ;
#22457 = CARTESIAN_POINT ( 'NONE',  ( 5.111951166545567027, 11.99449087320206431, 6.736519543253151276 ) ) ;
#22458 = CARTESIAN_POINT ( 'NONE',  ( -15.75167367066978485, 155.0373533369262589, -1.797107981590890358 ) ) ;
#22459 = CARTESIAN_POINT ( 'NONE',  ( 4.887170171423926845, 117.7483457736543500, -0.7389058998312844073 ) ) ;
#22460 = DIRECTION ( 'NONE',  ( -5.188838149069472160E-16, 1.699382548006136559E-16, 1.000000000000000000 ) ) ;
#22461 = CARTESIAN_POINT ( 'NONE',  ( -7.558302675500311985, 122.4263405438208991, -0.1204446389788524086 ) ) ;
#22462 = EDGE_CURVE ( 'NONE', #25690, #33817, #5437, .T. ) ;
#22463 = ADVANCED_FACE ( 'NONE', ( #35110 ), #34898, .T. ) ;
#22464 = CARTESIAN_POINT ( 'NONE',  ( -1.279006062070071170, 119.0230276286704054, -0.6822954352362460284 ) ) ;
#22465 = CARTESIAN_POINT ( 'NONE',  ( 3.361984464572039144, -15.63109852379819564, 5.271848418269179604 ) ) ;
#22466 = CARTESIAN_POINT ( 'NONE',  ( -4.476425760464393555, 71.61790547347303004, 1.524000000000005128 ) ) ;
#22467 = CIRCLE ( 'NONE', #27270, 3.683000000000001162 ) ;
#22468 = CARTESIAN_POINT ( 'NONE',  ( -46.89970385779243855, 22.02655025333852379, -4.237790764466935478 ) ) ;
#22469 = VERTEX_POINT ( 'NONE', #28908 ) ;
#22470 = B_SPLINE_SURFACE_WITH_KNOTS ( 'NONE', 3, 3, ( 
 ( #24516, #8346, #15356, #15568, #2185, #24736, #11959, #38381, #18549, #37739, #34759, #34980, #15143, #41581, #8562, #25169, #21315 ),
 ( #5802, #5380, #8982, #22151, #21949, #34344, #35182, #18757, #12389, #37952, #31977, #24951, #8776, #5174, #14933, #21736, #31553 ),
 ( #2397, #25782, #19388, #9601, #13000, #39422, #39211, #26207, #13224, #29406, #3023, #10019, #23197, #3865, #13433, #25579, #36231 ),
 ( #25993, #19803, #9394, #26419, #39002, #3224, #6213, #9813, #20019, #22358, #6625, #38585, #460, #19184, #246, #35600, #35383 ),
 ( #10227, #15979, #32603, #22779, #6417, #32392, #35, #28976, #32189, #16185, #41996, #35810, #12793, #19592, #38790, #7052, #29624 ),
 ( #16830, #29189, #3436, #16401, #22991, #33037, #22570, #36017, #6832, #32821, #3650, #41792, #16617, #12590, #17660, #27475, #11278 ) ),
 .UNSPECIFIED., .F., .F., .F.,
 ( 4, 2, 4 ),
 ( 4, 1, 1, 1, 1, 1, 1, 1, 1, 1, 1, 1, 1, 1, 4 ),
 ( 0.000000000000000000, 0.5000000000000000000, 1.000000000000000000 ),
 ( 0.000000000000000000, 0.08300113939718137268, 0.1732806554784933895, 0.2717672377176819087, 0.3752096606209606167, 0.4787223716043260135, 0.5772295444745598747, 0.6668133826162351285, 0.7470991451079272982, 0.7815930070524458317, 0.8169452614683294644, 0.8547689062991584708, 0.8968063284581728745, 0.9447228702782888288, 1.000000000000000000 ),
 .UNSPECIFIED. ) ;
#22471 = CARTESIAN_POINT ( 'NONE',  ( 5.832110448082596044, 156.9788419092994047, 1.931507550941140794 ) ) ;
#22472 = CARTESIAN_POINT ( 'NONE',  ( -15.19943428492320869, 148.1072807477730748, -0.3037208696559880461 ) ) ;
#22473 = EDGE_CURVE ( 'NONE', #41900, #39553, #22918, .T. ) ;
#22474 = AXIS2_PLACEMENT_3D ( 'NONE', #26852, #14676, #39859 ) ;
#22475 = CARTESIAN_POINT ( 'NONE',  ( 13.85159022459153988, 12.96416000000000146, -5.016499999999999737 ) ) ;
#22476 = CARTESIAN_POINT ( 'NONE',  ( -3.375001179497743031, 119.3320731715853782, 0.4843141097021078090 ) ) ;
#22477 = EDGE_CURVE ( 'NONE', #23676, #24684, #16303, .T. ) ;
#22478 = CARTESIAN_POINT ( 'NONE',  ( -2.299398447937291756, 29.65396322172144039, -8.101725167555347440 ) ) ;
#22479 = CARTESIAN_POINT ( 'NONE',  ( 4.418888662852166860, 155.8637389808261275, 0.7167756870077641729 ) ) ;
#22480 = CARTESIAN_POINT ( 'NONE',  ( 8.141728797601116341, 117.8329967196738153, -0.4384511054415164422 ) ) ;
#22481 = CARTESIAN_POINT ( 'NONE',  ( 4.822993300437530273, 117.8022149080996570, 0.9221314676250721432 ) ) ;
#22482 = DIRECTION ( 'NONE',  ( -4.017660918040594346E-17, 1.000000000000000000, 2.376309959284834438E-19 ) ) ;
#22483 = CARTESIAN_POINT ( 'NONE',  ( -0.2937963077019585811, 116.4254261620736344, 0.006796306282692864999 ) ) ;
#22484 = ADVANCED_FACE ( 'NONE', ( #29336 ), #2029, .T. ) ;
#22485 = ORIENTED_EDGE ( 'NONE', *, *, #38388, .T. ) ;
#22486 = CARTESIAN_POINT ( 'NONE',  ( -8.178145033566243782, 120.5865709611434369, -1.415302197751513225 ) ) ;
#22487 = CARTESIAN_POINT ( 'NONE',  ( 5.819807902803178834, -14.34990091593344808, 2.641378012185163104 ) ) ;
#22488 = CARTESIAN_POINT ( 'NONE',  ( -10.60367000503898538, 126.1357510980948575, -0.6849044484263042687 ) ) ;
#22489 = CARTESIAN_POINT ( 'NONE',  ( 4.222548444470398010, -13.63200092856201096, 3.862739453107805421 ) ) ;
#22490 = FACE_OUTER_BOUND ( 'NONE', #21111, .T. ) ;
#22491 = VECTOR ( 'NONE', #24224, 1000.000000000000114 ) ;
#22492 = CARTESIAN_POINT ( 'NONE',  ( 20.69909148798420517, 152.5508394022679113, 0.4136171090298729758 ) ) ;
#22493 = ORIENTED_EDGE ( 'NONE', *, *, #34761, .F. ) ;
#22494 = CARTESIAN_POINT ( 'NONE',  ( 4.513502956352341222, 8.064680226961385756, -0.9949261897555528034 ) ) ;
#22495 = CARTESIAN_POINT ( 'NONE',  ( -11.74288454345109756, 118.7273140689154616, -0.2346507796901759757 ) ) ;
#22496 = CARTESIAN_POINT ( 'NONE',  ( -21.90559427349733213, 151.4293160993572940, -0.4377259060014722092 ) ) ;
#22497 = CARTESIAN_POINT ( 'NONE',  ( -0.1064799869812408512, 105.7853621660184444, 5.332934571178566507 ) ) ;
#22498 = CARTESIAN_POINT ( 'NONE',  ( -6.350000000000055600, 85.80437499999999318, 8.456951552361941263E-16 ) ) ;
#22499 = CARTESIAN_POINT ( 'NONE',  ( -6.115548012816138801, 121.1758403914483466, 0.4341407379041746784 ) ) ;
#22500 = CARTESIAN_POINT ( 'NONE',  ( -4.168830513765062307, 9.198770455692846681, 1.997586429550192166 ) ) ;
#22501 = CARTESIAN_POINT ( 'NONE',  ( 22.05995121575384843, 150.4421090420883900, 1.612468304426259325 ) ) ;
#22502 = CARTESIAN_POINT ( 'NONE',  ( -0.07831152689652476351, 109.4728569552520838, 3.919029035233729363 ) ) ;
#22504 = CARTESIAN_POINT ( 'NONE',  ( 4.041216738202956016, 118.0179939250997023, -0.7376333572805301442 ) ) ;
#22503 = CARTESIAN_POINT ( 'NONE',  ( 2.906309357581933650, -13.72804873580029472, 0.7610837935892840189 ) ) ;
#22505 = VECTOR ( 'NONE', #15985, 1000.000000000000227 ) ;
#22506 = CARTESIAN_POINT ( 'NONE',  ( -4.168830513765062307, 9.198770455692846681, 1.997586429550192166 ) ) ;
#22507 = CARTESIAN_POINT ( 'NONE',  ( -1.940752395788367446, 116.9162416783649689, -0.4172132017389482694 ) ) ;
#22508 = ORIENTED_EDGE ( 'NONE', *, *, #1230, .T. ) ;
#22509 = EDGE_CURVE ( 'NONE', #19469, #296, #31252, .T. ) ;
#22510 = CARTESIAN_POINT ( 'NONE',  ( -14.89139266796671635, 148.8756053271976327, 0.4181552259878851818 ) ) ;
#22511 = CARTESIAN_POINT ( 'NONE',  ( 6.095337826619875443, -12.40160515274643593, 0.5428006832284221206 ) ) ;
#22512 = CARTESIAN_POINT ( 'NONE',  ( -6.615214180512292604E-14, 94.32746620154571815, -2.829521569843129660E-18 ) ) ;
#22513 = CARTESIAN_POINT ( 'NONE',  ( -4.535049786513674519, 118.0744006754055562, -0.7972472874695084588 ) ) ;
#22514 = CARTESIAN_POINT ( 'NONE',  ( 7.044606587285096033, 122.0729346620515088, 0.1407680048458705979 ) ) ;
#22515 = VERTEX_POINT ( 'NONE', #19316 ) ;
#22516 = CARTESIAN_POINT ( 'NONE',  ( 14.77311812546545156, 125.6006210965460781, 2.040279103193882282 ) ) ;
#22517 = DIRECTION ( 'NONE',  ( -0.9998004120163609398, -5.205824365704083189E-17, -0.01997839162482749689 ) ) ;
#22518 = DIRECTION ( 'NONE',  ( -4.017660918040594346E-17, 1.000000000000000000, 2.376309959284834438E-19 ) ) ;
#22519 = CIRCLE ( 'NONE', #35489, 0.2539999999999942859 ) ;
#22520 = CARTESIAN_POINT ( 'NONE',  ( -14.14567801931327118, 120.5239346615589540, 0.5295366371686062168 ) ) ;
#22521 = EDGE_CURVE ( 'NONE', #41900, #10652, #42157, .T. ) ;
#22522 = CARTESIAN_POINT ( 'NONE',  ( 0.0005468344958371703160, 156.3034662015456604, -0.02736583427618478198 ) ) ;
#22523 = CARTESIAN_POINT ( 'NONE',  ( 15.06072413439829027, 156.1474796653986630, -0.2161187639505615099 ) ) ;
#22524 = CARTESIAN_POINT ( 'NONE',  ( -5.115874721081825172, 56.51499999999997215, -4.603382018214097648 ) ) ;
#22525 = AXIS2_PLACEMENT_3D ( 'NONE', #41945, #16779, #15931 ) ;
#22526 = CARTESIAN_POINT ( 'NONE',  ( -51.80188483046436687, 13.03002009012210927, 4.294765137396908017 ) ) ;
#22527 = CARTESIAN_POINT ( 'NONE',  ( -46.98785713747574277, 25.41845405000909253, 0.7790854875835052651 ) ) ;
#22528 = CYLINDRICAL_SURFACE ( 'NONE', #14199, 15.21260244842765808 ) ;
#22529 = VERTEX_POINT ( 'NONE', #13147 ) ;
#22530 = CARTESIAN_POINT ( 'NONE',  ( -48.59875010875282442, 18.41211343146811785, 5.165832069028382101 ) ) ;
#22531 = CARTESIAN_POINT ( 'NONE',  ( -10.84307050033138431, 78.30450799593342026, -1.523999999999998911 ) ) ;
#22532 = CARTESIAN_POINT ( 'NONE',  ( -4.605735037197680626, 118.0200015956283863, 0.6870595234115985939 ) ) ;
#22533 = CARTESIAN_POINT ( 'NONE',  ( -58.20750686534850615, 0.04498437427168100466, -0.4973296020553497065 ) ) ;
#22534 = ORIENTED_EDGE ( 'NONE', *, *, #830, .T. ) ;
#22535 = ORIENTED_EDGE ( 'NONE', *, *, #35079, .F. ) ;
#22536 = CARTESIAN_POINT ( 'NONE',  ( -41.23752580366542020, 23.26788267949596190, -1.524000000000005128 ) ) ;
#22537 =( BOUNDED_SURFACE ( )  B_SPLINE_SURFACE ( 3, 2, ( 
 ( #26604, #13614, #33011 ),
 ( #37044, #33849, #7862 ),
 ( #27237, #36419, #7445 ),
 ( #40251, #1272, #29806 ),
 ( #39611, #10833, #23604 ),
 ( #4470, #33223, #13823 ),
 ( #20403, #14023, #23387 ),
 ( #4677, #7237, #30426 ),
 ( #36625, #20197, #4050 ),
 ( #7656, #26392, #17011 ),
 ( #11044, #24029, #30010 ),
 ( #16803, #10199, #849 ),
 ( #39828, #10622, #27030 ),
 ( #17634, #30636, #36836 ),
 ( #33433, #17427, #4260 ),
 ( #17223, #33643, #39397 ),
 ( #8061, #11666, #21036 ),
 ( #5508, #24872, #34060 ),
 ( #18466, #31686, #40658 ),
 ( #4888, #21653, #21867 ) ),
 .UNSPECIFIED., .F., .F., .T. ) 
 B_SPLINE_SURFACE_WITH_KNOTS ( ( 4, 2, 2, 2, 2, 2, 2, 2, 2, 4 ),
 ( 3, 3 ),
 ( -2.835263634875403419E-05, 0.001133586441676013700, 0.001714555980688397662, 0.002295525519700781624, 0.003457464597725549114, 0.003747949367231741095, 0.004038434136737933076, 0.004183676521491029067, 0.004328918906244125057, 0.004619403675750317038 ),
 ( 0.000000000000000000, 0.7115407172542784764 ),
 .UNSPECIFIED. ) 
 GEOMETRIC_REPRESENTATION_ITEM ( )  RATIONAL_B_SPLINE_SURFACE ( (
 ( 1.000000000000000000, 0.8295190889138120971, 0.9016463973324821968),
 ( 1.000000000000000000, 0.8295190889138120971, 0.9016463973324821968),
 ( 1.000000000000000000, 0.8295191357741429350, 0.9016464243670769818),
 ( 1.000000000000000000, 0.8295190646856472894, 0.9016463833548040707),
 ( 1.000000000000000000, 0.8295185271377292224, 0.9016460732334303785),
 ( 1.000000000000000000, 0.8295186176601453409, 0.9016461254574927864),
 ( 1.000000000000000000, 0.8295190559657723561, 0.9016463783241464025),
 ( 1.000000000000000000, 0.8295191606352591007, 0.9016464387099165645),
 ( 1.000000000000000000, 0.8295190986999689819, 0.9016464029782977896),
 ( 1.000000000000000000, 0.8295190867078258146, 0.9016463960598077865),
 ( 1.000000000000000000, 0.8295190998541304150, 0.9016464036441549368),
 ( 1.000000000000000000, 0.8295190811289877564, 0.9016463928412725704),
 ( 1.000000000000000000, 0.8295192486502576124, 0.9016464894874032243),
 ( 1.000000000000000000, 0.8295190462722409341, 0.9016463727317682864),
 ( 1.000000000000000000, 0.8295188582200193617, 0.9016462642409502903),
 ( 1.000000000000000000, 0.8295187249109206018, 0.9016461873324561616),
 ( 1.000000000000000000, 0.8295190035458798183, 0.9016463480821370613),
 ( 1.000000000000000000, 0.8295192259831494219, 0.9016464764103275797),
 ( 1.000000000000000000, 0.8295190889132049161, 0.9016463973321320324),
 ( 1.000000000000000000, 0.8295190889132049161, 0.9016463973321320324) ) ) 
 REPRESENTATION_ITEM ( '' )  SURFACE ( )  );
#22538 = CARTESIAN_POINT ( 'NONE',  ( 8.447822738470250670, 119.5131637967545259, -1.065025361500244072 ) ) ;
#22539 = CARTESIAN_POINT ( 'NONE',  ( -5.888892352462247182, 118.9932487913337411, -0.5850130909721117378 ) ) ;
#22540 = CARTESIAN_POINT ( 'NONE',  ( 4.784214230320843697, 117.8428681949036729, 0.9402043361855015879 ) ) ;
#22541 = CARTESIAN_POINT ( 'NONE',  ( 2.906309357581933650, -13.72804873580029472, 0.7610837935892840189 ) ) ;
#22542 = CARTESIAN_POINT ( 'NONE',  ( -3.584950684498069418, 120.6468399921648711, -0.5021239885730617303 ) ) ;
#22543 = DIRECTION ( 'NONE',  ( -0.1469470846586743984, -9.335746474409589170E-17, 0.9891443546370349837 ) ) ;
#22544 = CARTESIAN_POINT ( 'NONE',  ( -0.6265688110002558542, 106.0241047940699559, 5.258438125228670046 ) ) ;
#22545 = CARTESIAN_POINT ( 'NONE',  ( 5.755298473670368509, 118.4539739381501988, -0.4326931426192709429 ) ) ;
#22546 = CARTESIAN_POINT ( 'NONE',  ( -6.534901955149031494, 120.8223817900871495, -1.022280983926979303 ) ) ;
#22547 = DIRECTION ( 'NONE',  ( -0.7071067811865486830, -0.7071067811865464625, 8.659560562354946417E-17 ) ) ;
#22548 = CARTESIAN_POINT ( 'NONE',  ( -0.01887972822151516225, 159.3676309965788960, 0.9448188026860502298 ) ) ;
#22549 = DIRECTION ( 'NONE',  ( 0.8745520943968236871, -0.4849315768086559508, 6.829619984160659032E-16 ) ) ;
#22550 = CARTESIAN_POINT ( 'NONE',  ( 4.440276399826426967, -1.430929408009915083, -1.287880193523989636 ) ) ;
#22552 = ORIENTED_EDGE ( 'NONE', *, *, #25321, .T. ) ;
#22551 = CARTESIAN_POINT ( 'NONE',  ( 5.825324126169723726, 117.1711376449269721, 0.5405197603966794828 ) ) ;
#22553 = LINE ( 'NONE', #35583, #12457 ) ;
#22554 = CARTESIAN_POINT ( 'NONE',  ( 3.555255404795384599, -15.46298345743583802, 3.323699395844104565 ) ) ;
#22555 = CARTESIAN_POINT ( 'NONE',  ( -19.37548274631734557, 145.1342744731992127, 1.755133555010167656 ) ) ;
#22556 = CARTESIAN_POINT ( 'NONE',  ( 0.6214172073067296687, 11.15065110656550118, 0.7500636867869169278 ) ) ;
#22557 = CIRCLE ( 'NONE', #8968, 0.2539999999999966729 ) ;
#22558 = CARTESIAN_POINT ( 'NONE',  ( -0.9676832378731173856, 3.540085264489355676, -0.1409938603398425416 ) ) ;
#22559 = ORIENTED_EDGE ( 'NONE', *, *, #19654, .T. ) ;
#22560 = ORIENTED_EDGE ( 'NONE', *, *, #7974, .F. ) ;
#22561 = CARTESIAN_POINT ( 'NONE',  ( -47.40532530373579334, 16.48158934372809270, 0.7854836779715855810 ) ) ;
#22562 = CARTESIAN_POINT ( 'NONE',  ( 3.138057391968664067, 117.6701293611589278, 1.012097185230346419 ) ) ;
#22563 = APPLICATION_PROTOCOL_DEFINITION ( 'draft international standard', 'automotive_design', 1998, #42030 ) ;
#22564 = CARTESIAN_POINT ( 'NONE',  ( -10.66674206690823468, 124.7671305375842934, 0.7411263988551110016 ) ) ;
#22565 = CARTESIAN_POINT ( 'NONE',  ( 3.901187470525758094, -13.68826627043556776, 3.907672046116945186 ) ) ;
#22566 = CARTESIAN_POINT ( 'NONE',  ( 1.391675519083714674, 119.6596719632383383, -0.5469696729655012524 ) ) ;
#22567 = CARTESIAN_POINT ( 'NONE',  ( 0.01152893261308097703, 118.7114655739656257, -0.5769549317675698452 ) ) ;
#22568 = DIRECTION ( 'NONE',  ( 4.017660918040594346E-17, -1.000000000000000000, -2.376309959284834438E-19 ) ) ;
#22569 = CARTESIAN_POINT ( 'NONE',  ( 8.232931626680233705, 120.3169219327360508, 1.441413524645123623 ) ) ;
#22570 = CARTESIAN_POINT ( 'NONE',  ( -2.579283729523311752, 34.63205429821886838, 0.7922911722492691489 ) ) ;
#22571 = CARTESIAN_POINT ( 'NONE',  ( 14.35733687469664410, 139.0340687859245463, -0.1707862337897577132 ) ) ;
#22572 = VERTEX_POINT ( 'NONE', #36382 ) ;
#22573 = CARTESIAN_POINT ( 'NONE',  ( 17.14499999999999957, 71.11999999999999034, -5.016499999999999737 ) ) ;
#22574 = LINE ( 'NONE', #29195, #15706 ) ;
#22575 = CARTESIAN_POINT ( 'NONE',  ( -58.50248613193047476, -0.02569321026645032813, 0.6864972099047519372 ) ) ;
#22576 = CARTESIAN_POINT ( 'NONE',  ( 3.584950684497941076, 120.6468399921648711, 0.5021239885730618413 ) ) ;
#22577 = CARTESIAN_POINT ( 'NONE',  ( 10.92199999999999704, 12.96416000000000146, 0.000000000000000000 ) ) ;
#22578 = CARTESIAN_POINT ( 'NONE',  ( 0.3004615168031275485, 116.4565202671238069, -0.06108086412306412694 ) ) ;
#22579 = CARTESIAN_POINT ( 'NONE',  ( -0.8832484628483068256, 105.9424719104300436, 5.282093952356136768 ) ) ;
#22580 = VECTOR ( 'NONE', #21707, 1000.000000000000000 ) ;
#22581 = DIRECTION ( 'NONE',  ( 0.01997839162482749689, 1.040247600000945640E-18, -0.9998004120163610509 ) ) ;
#22582 = CARTESIAN_POINT ( 'NONE',  ( -3.594857975007920814, -7.703025367003809798, -2.923569511714296798 ) ) ;
#22583 = CARTESIAN_POINT ( 'NONE',  ( -4.530671860764704739, 32.23439806600806889, 0.8345080972855752899 ) ) ;
#22584 = CARTESIAN_POINT ( 'NONE',  ( -0.02874440110946640745, 158.8294072187990196, 1.438487372358303373 ) ) ;
#22585 = CARTESIAN_POINT ( 'NONE',  ( 2.264360804680111805, 21.29314879275315064, 4.027482774281332389 ) ) ;
#22586 = CARTESIAN_POINT ( 'NONE',  ( -7.958381229837070414, -11.09356959825496247, -2.748999415197344476 ) ) ;
#22587 = CARTESIAN_POINT ( 'NONE',  ( -5.485516209714965008, 117.1863486007777766, -0.7935004768815202558 ) ) ;
#22588 = CARTESIAN_POINT ( 'NONE',  ( -2.988627099741104853, 122.7580772961051707, -0.2146329844597061054 ) ) ;
#22589 = CARTESIAN_POINT ( 'NONE',  ( 0.01793833495430298061, 118.1627382089642566, -0.8977079103094813828 ) ) ;
#22590 = CARTESIAN_POINT ( 'NONE',  ( 1.769773243241540950, 106.5493969454534522, -4.971304634441370496 ) ) ;
#22591 = CARTESIAN_POINT ( 'NONE',  ( -0.2386208842475691927, 105.1223928365816391, 5.340289220565798800 ) ) ;
#22592 = CARTESIAN_POINT ( 'NONE',  ( -4.563195415240126174, 21.88328375387019165, -0.7336086519975816289 ) ) ;
#22593 = FACE_OUTER_BOUND ( 'NONE', #30468, .T. ) ;
#22594 = DIRECTION ( 'NONE',  ( 0.7071067811865475727, -0.7071067811865474617, 0.000000000000000000 ) ) ;
#22595 = CARTESIAN_POINT ( 'NONE',  ( 3.116451998213339625, -14.00698646007624149, 1.619014592372306716 ) ) ;
#22596 = CARTESIAN_POINT ( 'NONE',  ( 1.626581124784194143, 119.3928400758114918, -0.6183738137425958126 ) ) ;
#22597 = CARTESIAN_POINT ( 'NONE',  ( -4.817281438370394575, 117.0090399748681875, 0.3002870190743006651 ) ) ;
#22598 = AXIS2_PLACEMENT_3D ( 'NONE', #15783, #28791, #41803 ) ;
#22599 = VERTEX_POINT ( 'NONE', #32970 ) ;
#22600 = CARTESIAN_POINT ( 'NONE',  ( 5.305748947172191698, 77.01756249999996840, 5.247078976224250013 ) ) ;
#22601 = ORIENTED_EDGE ( 'NONE', *, *, #14115, .F. ) ;
#22602 = CARTESIAN_POINT ( 'NONE',  ( -3.113414239748029111, 30.98679946927233431, 0.04088859964249514506 ) ) ;
#22603 = CARTESIAN_POINT ( 'NONE',  ( 3.743762692837560468, -15.60843739440008449, 4.988928788737716502 ) ) ;
#22604 = CARTESIAN_POINT ( 'NONE',  ( -11.48785675552158381, 156.2473422840488979, 1.634126210350451691 ) ) ;
#22605 = CARTESIAN_POINT ( 'NONE',  ( 9.403995501905139776, 118.7255599110314961, -0.7521618898589477187 ) ) ;
#22606 = CARTESIAN_POINT ( 'NONE',  ( 3.064284189169764971, -3.155149710853871525, 3.465721614369133174 ) ) ;
#22607 = CARTESIAN_POINT ( 'NONE',  ( -53.82649921536103221, 9.579626810350022836, -3.792271429080182887 ) ) ;
#22608 = EDGE_LOOP ( 'NONE', ( #35370, #35414, #16012, #11014 ) ) ;
#22609 = CARTESIAN_POINT ( 'NONE',  ( -58.45963793110830409, -0.4469582673305985687, -0.3141006534898306835 ) ) ;
#22610 = CARTESIAN_POINT ( 'NONE',  ( -0.001862839608873425017, 124.0591982226671490, 0.09322411149286721765 ) ) ;
#22611 = CARTESIAN_POINT ( 'NONE',  ( -11.67916898317110785, 124.4569610989641859, 1.132436424213030035 ) ) ;
#22612 = DIRECTION ( 'NONE',  ( 0.6294287539884133587, 0.7770581983690755257, 0.000000000000000000 ) ) ;
#22613 = CARTESIAN_POINT ( 'NONE',  ( 12.69690185265270266, 124.0847267554996591, -1.337322108705696566 ) ) ;
#22614 = CARTESIAN_POINT ( 'NONE',  ( -18.59893286765449005, 151.9584835496716266, -2.273025404440324859 ) ) ;
#22615 = CARTESIAN_POINT ( 'NONE',  ( -58.70413935429054675, 0.2332485698458008905, -0.6626129746612972049 ) ) ;
#22616 = CIRCLE ( 'NONE', #28080, 0.2540000000000000036 ) ;
#22617 = ORIENTED_EDGE ( 'NONE', *, *, #10234, .F. ) ;
#22618 = CARTESIAN_POINT ( 'NONE',  ( 4.591905152882217678, 118.0813191133225217, -0.5393609360573334843 ) ) ;
#22619 = CARTESIAN_POINT ( 'NONE',  ( 16.15477348297510574, 145.8839827664328368, -0.6502963436359732174 ) ) ;
#22620 = ORIENTED_EDGE ( 'NONE', *, *, #36960, .F. ) ;
#22621 = CARTESIAN_POINT ( 'NONE',  ( -10.58192191572921637, 122.8495954190337898, -1.525858888728604645 ) ) ;
#22622 = CARTESIAN_POINT ( 'NONE',  ( 1.983586949722073500, -15.35435952563934947, 5.265070481109153988 ) ) ;
#22623 = CARTESIAN_POINT ( 'NONE',  ( -0.5136306012015983136, 105.1226572023712009, -5.319725606971133836 ) ) ;
#22624 = AXIS2_PLACEMENT_3D ( 'NONE', #9724, #41910, #25699 ) ;
#22625 = CARTESIAN_POINT ( 'NONE',  ( -55.83515739322318439, 4.224161455597882586, -1.000857388952954637E-14 ) ) ;
#22626 = CARTESIAN_POINT ( 'NONE',  ( -4.862062482173646671, 117.7349268748283322, 0.8245466556072992281 ) ) ;
#22627 = CARTESIAN_POINT ( 'NONE',  ( 3.575075884023247053, 156.6183338678525558, 1.521800568792661235 ) ) ;
#22628 = CARTESIAN_POINT ( 'NONE',  ( -46.60530155212504155, 26.17382724835478314, 1.523999999999996913 ) ) ;
#22629 = CARTESIAN_POINT ( 'NONE',  ( 8.369515367582838650, -11.69187915512254783, 0.7729349465547848963 ) ) ;
#22630 = CARTESIAN_POINT ( 'NONE',  ( 9.242391706085484770, 124.1957968681474824, 0.3461533994140004178 ) ) ;
#22631 = CARTESIAN_POINT ( 'NONE',  ( -50.15972161391664486, 17.13814111569220699, -4.955022299345085202 ) ) ;
#22632 = CARTESIAN_POINT ( 'NONE',  ( -48.16508968810063607, 19.01313136326714925, -5.219744232931994965 ) ) ;
#22633 = LINE ( 'NONE', #35670, #2650 ) ;
#22634 = VECTOR ( 'NONE', #31050, 1000.000000000000227 ) ;
#22635 = CARTESIAN_POINT ( 'NONE',  ( -46.65118376738641359, 26.08833806145381473, -1.300560147374372866 ) ) ;
#22636 = CARTESIAN_POINT ( 'NONE',  ( -48.78337893976456030, 18.15300145085139860, 5.151671844828033642 ) ) ;
#22637 = CARTESIAN_POINT ( 'NONE',  ( -8.537794462167497045, 118.8508514274944332, -1.228900455792910407 ) ) ;
#22638 = CARTESIAN_POINT ( 'NONE',  ( -18.35410564743290962, 77.35382415001784295, -1.904999999999999583 ) ) ;
#22639 = LINE ( 'NONE', #35675, #5577 ) ;
#22640 = CARTESIAN_POINT ( 'NONE',  ( -55.45615287082594591, 8.171946630687445534, 2.478682617993481774 ) ) ;
#22641 = CARTESIAN_POINT ( 'NONE',  ( -57.81953393267934160, 1.609514594907199392, 1.636666387507130782 ) ) ;
#22642 = CARTESIAN_POINT ( 'NONE',  ( -11.62351318166555458, 118.7506923092098674, 0.05658863777226878777 ) ) ;
#22643 = AXIS2_PLACEMENT_3D ( 'NONE', #25892, #31662, #38273 ) ;
#22644 = VERTEX_POINT ( 'NONE', #15908 ) ;
#22645 = ORIENTED_EDGE ( 'NONE', *, *, #40941, .F. ) ;
#22646 = CARTESIAN_POINT ( 'NONE',  ( -55.24575511360421842, 11.19612964283526324, -0.2458718103055786974 ) ) ;
#22647 = CARTESIAN_POINT ( 'NONE',  ( 6.037966007429210968, 121.4449702037965295, 0.07866225072108197491 ) ) ;
#22648 = VERTEX_POINT ( 'NONE', #35524 ) ;
#22649 = CARTESIAN_POINT ( 'NONE',  ( 3.151445404061590683, 115.7029491485452866, -1.538701385061280069 ) ) ;
#22650 = CARTESIAN_POINT ( 'NONE',  ( -9.132214679254637701, 153.9061766533773152, -0.3822102345680641888 ) ) ;
#22651 = CARTESIAN_POINT ( 'NONE',  ( 6.072898904334845582, -12.55662260458653634, 0.7994981368886315831 ) ) ;
#22652 = CARTESIAN_POINT ( 'NONE',  ( -6.847865590701599281, 118.2876074772933492, 0.8134140678991771400 ) ) ;
#22653 = CARTESIAN_POINT ( 'NONE',  ( 4.968812502025208744, 56.51947257897050036, -4.801689445572365322 ) ) ;
#22654 = AXIS2_PLACEMENT_3D ( 'NONE', #16794, #23160, #19348 ) ;
#22655 = CARTESIAN_POINT ( 'NONE',  ( 13.56676737375326347, 119.6371495169912436, 0.4909217195147886348 ) ) ;
#22656 = CARTESIAN_POINT ( 'NONE',  ( 2.871147452325312432, 156.1036873960511286, 0.1443595091093279881 ) ) ;
#22657 = DIRECTION ( 'NONE',  ( 0.000000000000000000, -1.000000000000000000, -0.000000000000000000 ) ) ;
#22658 = CARTESIAN_POINT ( 'NONE',  ( 0.1941685572964340079, 16.06069190514159928, 0.9568941237268799860 ) ) ;
#22659 = CARTESIAN_POINT ( 'NONE',  ( -23.34655412193315982, 148.8653451956335516, -0.6207958181910344653 ) ) ;
#22660 = DIRECTION ( 'NONE',  ( -6.353134868986659519E-16, 1.000000000000000000, 0.000000000000000000 ) ) ;
#22661 = CARTESIAN_POINT ( 'NONE',  ( -5.237832120027546168, 115.7029491485453718, -1.023639123012231034 ) ) ;
#22662 = ORIENTED_EDGE ( 'NONE', *, *, #4319, .T. ) ;
#22663 = CARTESIAN_POINT ( 'NONE',  ( 2.467838008569906982, 116.7125891676179492, 0.4911571291703088482 ) ) ;
#22664 = ORIENTED_EDGE ( 'NONE', *, *, #10739, .T. ) ;
#22665 = CARTESIAN_POINT ( 'NONE',  ( -58.31002553906358798, -0.1654322197361378644, -0.3101674830710153818 ) ) ;
#22666 = CARTESIAN_POINT ( 'NONE',  ( 4.913347341789697786, 118.0342071775839941, 0.9606804153092149967 ) ) ;
#22667 = CARTESIAN_POINT ( 'NONE',  ( 8.792330854012570640, 120.0394951565550343, -1.134075770671235217 ) ) ;
#22668 = CARTESIAN_POINT ( 'NONE',  ( -0.4837089014371968032, -0.2951250844416551944, 0.8451309203121293301 ) ) ;
#22669 = CARTESIAN_POINT ( 'NONE',  ( -4.414756536061148928, 7.050034479431100287, -7.184669936685727620 ) ) ;
#22670 = CARTESIAN_POINT ( 'NONE',  ( -9.289280848106855615, 118.8811571165754941, -1.201727579052786377 ) ) ;
#22671 = CARTESIAN_POINT ( 'NONE',  ( 4.663464417680016183, 117.9609724899354859, -0.7408843369873798768 ) ) ;
#22672 = CARTESIAN_POINT ( 'NONE',  ( 4.792324638247207780, 56.51998046905276141, 4.972049999977001811 ) ) ;
#22673 = CARTESIAN_POINT ( 'NONE',  ( -4.224755116450005232, 155.8535809751167562, -0.04780361979672655831 ) ) ;
#22674 = ORIENTED_EDGE ( 'NONE', *, *, #36852, .T. ) ;
#22675 = CARTESIAN_POINT ( 'NONE',  ( -6.619107555072970328, 119.9895581359321994, -1.245414878088068056 ) ) ;
#22676 = CARTESIAN_POINT ( 'NONE',  ( 4.276943344491330734, -15.69687736684960377, 3.951204673509490117 ) ) ;
#22677 = CIRCLE ( 'NONE', #21312, 0.2540000000000051106 ) ;
#22678 = CARTESIAN_POINT ( 'NONE',  ( 4.787409750893364624, 118.5931160184169073, 0.9399879859136054394 ) ) ;
#22679 = EDGE_CURVE ( 'NONE', #25879, #27003, #6346, .T. ) ;
#22680 = CARTESIAN_POINT ( 'NONE',  ( -44.55074271434504851, 21.27721161058206789, -3.389857510897070547 ) ) ;
#22681 = ORIENTED_EDGE ( 'NONE', *, *, #7621, .T. ) ;
#22682 = CARTESIAN_POINT ( 'NONE',  ( 2.442377090744232149, 119.5064228623769225, 0.7372000016323178029 ) ) ;
#22683 = DIRECTION ( 'NONE',  ( -6.146657985744592735E-16, 3.905054717696928257E-31, 1.000000000000000000 ) ) ;
#22684 = AXIS2_PLACEMENT_3D ( 'NONE', #21903, #25330, #41111 ) ;
#22685 = CARTESIAN_POINT ( 'NONE',  ( -4.548929788228186943, 119.7344140837147819, 0.3435137807816315836 ) ) ;
#22686 = CARTESIAN_POINT ( 'NONE',  ( 8.431793794909870243, 26.85621209503467455, -0.1224882448600171925 ) ) ;
#22687 = CARTESIAN_POINT ( 'NONE',  ( 5.232823448427218693, 121.2166884500396833, 0.3893023073710020210 ) ) ;
#22688 = EDGE_CURVE ( 'NONE', #20108, #16766, #29892, .T. ) ;
#22689 = CARTESIAN_POINT ( 'NONE',  ( 7.773589648320840872, 158.6130819278358501, -0.6584978287542903042 ) ) ;
#22690 = DIRECTION ( 'NONE',  ( 5.188838149069472160E-16, -1.699382548006136559E-16, -1.000000000000000000 ) ) ;
#22691 = AXIS2_PLACEMENT_3D ( 'NONE', #33923, #1555, #4754 ) ;
#22692 = AXIS2_PLACEMENT_3D ( 'NONE', #19122, #9340, #28718 ) ;
#22693 = CARTESIAN_POINT ( 'NONE',  ( -6.555005513994535572E-14, 79.34146620154574236, -6.390659674827382268E-18 ) ) ;
#22694 = PRODUCT_DEFINITION_CONTEXT ( 'detailed design', #22944, 'design' ) ;
#22695 = CARTESIAN_POINT ( 'NONE',  ( -1.798461198689529583, 116.4670535197835051, -0.02282230188723645067 ) ) ;
#22696 = VERTEX_POINT ( 'NONE', #12723 ) ;
#22697 = CARTESIAN_POINT ( 'NONE',  ( 6.372047788406695723, 120.0155008613895262, -0.9547430740777989033 ) ) ;
#22698 = CARTESIAN_POINT ( 'NONE',  ( 22.46755768833288158, 150.8526571111528654, 0.4489552724284878171 ) ) ;
#22699 = VECTOR ( 'NONE', #15105, 1000.000000000000000 ) ;
#22700 = CARTESIAN_POINT ( 'NONE',  ( -8.208845571667785279, 122.7966848691156514, -0.5426025200548864058 ) ) ;
#22701 = CARTESIAN_POINT ( 'NONE',  ( 2.073997095138572000, -14.95492255878227894, 5.604884748988061105 ) ) ;
#22702 = CARTESIAN_POINT ( 'NONE',  ( -5.125197423627203541, 116.9874462378649156, 0.2390140417207006485 ) ) ;
#22703 = CARTESIAN_POINT ( 'NONE',  ( 6.896076486346172096, 117.1676486657671177, 0.1523180551073342603 ) ) ;
#22704 = ORIENTED_EDGE ( 'NONE', *, *, #20655, .T. ) ;
#22705 = CARTESIAN_POINT ( 'NONE',  ( -4.603678009535974169, 12.38766144714272066, -0.4343361176327051321 ) ) ;
#22706 = EDGE_CURVE ( 'NONE', #16646, #27187, #3363, .T. ) ;
#22707 = CARTESIAN_POINT ( 'NONE',  ( 0.8498849898440922201, 105.1231291862523562, 5.276109398275504958 ) ) ;
#22708 = CARTESIAN_POINT ( 'NONE',  ( -4.801770124674531459, 117.3993836138989479, 1.016061141329191786 ) ) ;
#22709 = CARTESIAN_POINT ( 'NONE',  ( 3.686126148285236770, 108.9297438659294670, 3.861031192209934737 ) ) ;
#22710 = CARTESIAN_POINT ( 'NONE',  ( 7.821621632655430645, 122.4026362592563260, 0.6204867030296015162 ) ) ;
#22711 = EDGE_CURVE ( 'NONE', #40327, #35273, #39428, .T. ) ;
#22712 = CARTESIAN_POINT ( 'NONE',  ( 3.547999066118234346, 14.38381850277834317, -2.990331240093012433 ) ) ;
#22713 = CARTESIAN_POINT ( 'NONE',  ( 22.54106487284166960, 146.4122051224262577, 1.767531409769413475 ) ) ;
#22714 = CARTESIAN_POINT ( 'NONE',  ( -50.04979780823605751, 16.23027998585079601, -4.918765685689631795 ) ) ;
#22716 = CARTESIAN_POINT ( 'NONE',  ( 21.01144550848343684, 149.0309112320384486, -1.514039682450821322 ) ) ;
#22715 = CARTESIAN_POINT ( 'NONE',  ( 5.354045385511907007, 57.14999999999996305, 5.213862164334982729 ) ) ;
#22717 = CARTESIAN_POINT ( 'NONE',  ( 1.100877510726109954, 5.750359496286542971, -4.487862572965156005 ) ) ;
#22718 = CARTESIAN_POINT ( 'NONE',  ( -16.38310316169965830, 155.2191194103077407, -1.312707330359597302 ) ) ;
#22719 = EDGE_CURVE ( 'NONE', #10933, #22232, #12266, .T. ) ;
#22720 = VERTEX_POINT ( 'NONE', #42135 ) ;
#22721 = CARTESIAN_POINT ( 'NONE',  ( -1.588992450109173449, 120.9073379818811134, 0.1002710119552034512 ) ) ;
#22722 = CARTESIAN_POINT ( 'NONE',  ( 5.314795342858649185, -13.92002763284938638, 3.476347616104731753 ) ) ;
#22723 = CARTESIAN_POINT ( 'NONE',  ( 0.1695430583838596905, 115.7029491485453718, 1.764635982249148638 ) ) ;
#22724 = ORIENTED_EDGE ( 'NONE', *, *, #35707, .T. ) ;
#22725 = CARTESIAN_POINT ( 'NONE',  ( -0.03256023585726924852, 157.9544661776888290, 1.629447346748784664 ) ) ;
#22726 = CARTESIAN_POINT ( 'NONE',  ( 14.50851225146812595, 78.09971119798316863, 5.392902600000138769 ) ) ;
#22727 = CYLINDRICAL_SURFACE ( 'NONE', #15037, 5.588000000000006295 ) ;
#22728 = CARTESIAN_POINT ( 'NONE',  ( -0.3541790919672200832, 116.9919054422455531, 0.3273860145854424752 ) ) ;
#22729 = CARTESIAN_POINT ( 'NONE',  ( 8.185302851676453884, 117.6493956690293317, -0.2478838862282036759 ) ) ;
#22730 = CARTESIAN_POINT ( 'NONE',  ( -4.966122758792669067, 56.51499999999997215, -4.710630977848821566 ) ) ;
#22731 = CARTESIAN_POINT ( 'NONE',  ( -6.437058721807690810E-14, 62.83146620154573014, 4.519164521849267879E-29 ) ) ;
#22732 = CARTESIAN_POINT ( 'NONE',  ( -47.01067208220106863, 24.90190543975541360, 1.870441909736396902 ) ) ;
#22733 = CARTESIAN_POINT ( 'NONE',  ( 1.850362377257448232, -15.22409370683930341, 5.412180775546769240 ) ) ;
#22734 = CARTESIAN_POINT ( 'NONE',  ( -47.43570116002442205, 20.37060963802031566, 5.342502768866032703 ) ) ;
#22735 = DIRECTION ( 'NONE',  ( -0.8745520943968250194, 0.4849315768086535083, -5.424246918827963022E-16 ) ) ;
#22736 = CARTESIAN_POINT ( 'NONE',  ( -4.610742620264918656, 118.0210047857977003, 0.6828504890990388931 ) ) ;
#22737 = CARTESIAN_POINT ( 'NONE',  ( -5.901202670473868928, 78.88741954747034413, -5.016800487701043920 ) ) ;
#22738 = EDGE_CURVE ( 'NONE', #6546, #39412, #23773, .T. ) ;
#22739 = VERTEX_POINT ( 'NONE', #19524 ) ;
#22740 = ORIENTED_EDGE ( 'NONE', *, *, #24798, .F. ) ;
#22741 = FACE_OUTER_BOUND ( 'NONE', #19621, .T. ) ;
#22743 = ADVANCED_FACE ( 'NONE', ( #6981, #26562 ), #32532, .T. ) ;
#22742 = CARTESIAN_POINT ( 'NONE',  ( -3.570975303727345285, 118.7434192143189620, -0.9358452737509639352 ) ) ;
#22744 = CARTESIAN_POINT ( 'NONE',  ( -5.011858831344667031, 114.3657942991566472, -1.958205155698268696 ) ) ;
#22745 = CARTESIAN_POINT ( 'NONE',  ( 4.659120009405922858, 117.9637684512630500, 0.9018216066107574980 ) ) ;
#22746 = CARTESIAN_POINT ( 'NONE',  ( 2.769760999665409340, -14.92388480464812872, 4.423285184949336646 ) ) ;
#22747 = CARTESIAN_POINT ( 'NONE',  ( -1.501069045181644634, 120.4980338609919386, -0.3776272143368911149 ) ) ;
#22748 = CARTESIAN_POINT ( 'NONE',  ( -17.14499999999999957, 71.11999999999999034, 5.714999999999998082 ) ) ;
#22749 = DIRECTION ( 'NONE',  ( 0.6559537821943243197, -0.7548010569845282625, 8.537024980200743918E-16 ) ) ;
#22750 = LINE ( 'NONE', #2994, #10388 ) ;
#22751 = CARTESIAN_POINT ( 'NONE',  ( 5.300219172352869990, 116.7134249176580028, -0.8085863681920514301 ) ) ;
#22752 = CARTESIAN_POINT ( 'NONE',  ( -16.85437733762588763, 144.1809451582817587, -2.058110026898293921 ) ) ;
#22753 = CARTESIAN_POINT ( 'NONE',  ( -13.85159022459153988, 16.50999999999999801, -5.016499999999999737 ) ) ;
#22754 = CARTESIAN_POINT ( 'NONE',  ( -0.02768730785358111679, 158.9256195073445213, 1.385586103196075891 ) ) ;
#22755 = CARTESIAN_POINT ( 'NONE',  ( -6.733080298864849599E-14, 123.6644662015457214, 4.141858957710797243E-18 ) ) ;
#22756 = CARTESIAN_POINT ( 'NONE',  ( -15.52860580939315227, 147.5347899789022392, -0.2435143895907615208 ) ) ;
#22757 = CARTESIAN_POINT ( 'NONE',  ( -4.550674770548566173, 2.667180226961371137, -0.8080508602523946982 ) ) ;
#22759 = VERTEX_POINT ( 'NONE', #37002 ) ;
#22758 = CARTESIAN_POINT ( 'NONE',  ( 16.67457936879062785, 122.7093839631038463, 0.9722687365115705305 ) ) ;
#22760 = CARTESIAN_POINT ( 'NONE',  ( 5.024208363535699107, 104.6144662015413900, -1.824882619888055002 ) ) ;
#22761 = CARTESIAN_POINT ( 'NONE',  ( 3.351832917607362461, -15.21525542808549503, 3.277475278119628133 ) ) ;
#22762 = CARTESIAN_POINT ( 'NONE',  ( -12.30591244053544564, 123.0735437985678971, 1.316165607245708635 ) ) ;
#22763 = CARTESIAN_POINT ( 'NONE',  ( 0.2555639604167124768, 10.49987491555810593, 0.9396316490698124468 ) ) ;
#22764 = CARTESIAN_POINT ( 'NONE',  ( -2.832181158176262592, 116.7549172960530939, -0.3515502119895594912 ) ) ;
#22765 = ADVANCED_FACE ( 'NONE', ( #40615 ), #16965, .T. ) ;
#22766 = CARTESIAN_POINT ( 'NONE',  ( -0.9658880162092680077, 3.969362202269336226, 0.1338930134723784471 ) ) ;
#22767 = ORIENTED_EDGE ( 'NONE', *, *, #2212, .T. ) ;
#22768 = VERTEX_POINT ( 'NONE', #20572 ) ;
#22769 = CARTESIAN_POINT ( 'NONE',  ( -42.01646181069634878, 22.10209156318453694, 0.7046475714187654393 ) ) ;
#22770 = CARTESIAN_POINT ( 'NONE',  ( -0.1065646865916383690, 105.8844662015456919, 5.332932678536313809 ) ) ;
#22771 = DIRECTION ( 'NONE',  ( -1.145073529767529528E-18, -3.363395138353311800E-16, -0.9999999999999998890 ) ) ;
#22772 = AXIS2_PLACEMENT_3D ( 'NONE', #26824, #23819, #19996 ) ;
#22773 = CARTESIAN_POINT ( 'NONE',  ( -9.814938192569949038, 124.1138826855306831, 0.4990610963926597754 ) ) ;
#22774 = CARTESIAN_POINT ( 'NONE',  ( 2.474817137005230983, -14.89163965485640340, 5.628581999208025266 ) ) ;
#22775 = CARTESIAN_POINT ( 'NONE',  ( 15.29320056080882040, 150.6904849259475441, -1.473493523582195097 ) ) ;
#22776 = CARTESIAN_POINT ( 'NONE',  ( -1.027076152783870544, 158.1148137021529578, -1.645667644272182484 ) ) ;
#22777 = CARTESIAN_POINT ( 'NONE',  ( -48.16862273754407653, 19.56935307722002193, -5.361094314902742575 ) ) ;
#22778 = CARTESIAN_POINT ( 'NONE',  ( 8.267145744840583177, 120.1492222882854009, 1.449473100370770817 ) ) ;
#22779 = CARTESIAN_POINT ( 'NONE',  ( -0.5377276166119240308, 37.39316116396758360, -0.3507468784153330299 ) ) ;
#22780 = CARTESIAN_POINT ( 'NONE',  ( 15.80820582674403951, 146.9282941555416073, -0.1367419433413213647 ) ) ;
#22781 = VERTEX_POINT ( 'NONE', #4008 ) ;
#22782 = CYLINDRICAL_SURFACE ( 'NONE', #3425, 0.6350000000000014522 ) ;
#22783 = CARTESIAN_POINT ( 'NONE',  ( -26.07955644221209113, 72.55303096390359485, 1.269999999999993356 ) ) ;
#22784 = CARTESIAN_POINT ( 'NONE',  ( -58.82993853617183788, -0.2576789964694181645, 0.02280678270975886393 ) ) ;
#22785 = DIRECTION ( 'NONE',  ( 9.627370216492862708E-17, 1.000000000000000000, -0.000000000000000000 ) ) ;
#22786 = CARTESIAN_POINT ( 'NONE',  ( 22.53108783561238226, 150.7873321363286152, 0.2974592429706746644 ) ) ;
#22787 = CARTESIAN_POINT ( 'NONE',  ( -0.3646759018191795265, 105.8822825325953261, 5.328619312200441271 ) ) ;
#22788 = DIRECTION ( 'NONE',  ( 0.9998004120163608288, 0.000000000000000000, 0.01997839162482749342 ) ) ;
#22789 = DIRECTION ( 'NONE',  ( -4.017660918040594346E-17, 1.000000000000000000, 2.376309959284834438E-19 ) ) ;
#22790 = CARTESIAN_POINT ( 'NONE',  ( -0.7874499056167989508, 36.06947511884756352, -0.2613531129797825869 ) ) ;
#22791 = CARTESIAN_POINT ( 'NONE',  ( 2.740693480742271149, 158.6924860557018064, 1.553331106148862606 ) ) ;
#22792 = CIRCLE ( 'NONE', #20767, 1.396999999999998909 ) ;
#22793 = CARTESIAN_POINT ( 'NONE',  ( 1.027636191897724816, 24.96647085856908532, -4.506105791511280323 ) ) ;
#22794 = CARTESIAN_POINT ( 'NONE',  ( -6.736519641741455899, -9.595509028896938020, 5.111951147309959254 ) ) ;
#22795 = CARTESIAN_POINT ( 'NONE',  ( -8.717398971979335442, 118.0183826319925373, -0.7839213143053921362 ) ) ;
#22796 = CARTESIAN_POINT ( 'NONE',  ( -3.315449255180983545, 124.9344662015457743, -0.06625056644921928362 ) ) ;
#22797 = CARTESIAN_POINT ( 'NONE',  ( 5.511035053980530840, -11.68933965407963704, 0.7135650660036900739 ) ) ;
#22798 = CARTESIAN_POINT ( 'NONE',  ( -10.92199999999999527, 55.98894877578615592, 6.098637220230963427E-16 ) ) ;
#22799 = CARTESIAN_POINT ( 'NONE',  ( -0.9366858060089110483, 104.6144662015478701, 5.262845480310400781 ) ) ;
#22800 = CARTESIAN_POINT ( 'NONE',  ( 3.400481176189167343, 25.78150505744974552, 3.158589348000393482 ) ) ;
#22801 = CARTESIAN_POINT ( 'NONE',  ( -6.059261036834082681, 78.87450423423038615, -5.016499999999999737 ) ) ;
#22802 = CARTESIAN_POINT ( 'NONE',  ( 2.857130780617909149, -14.87311083204414786, 4.269097905712053276 ) ) ;
#22803 = CARTESIAN_POINT ( 'NONE',  ( 2.387353046264464762, 119.4803856251332945, -0.5366433100809052670 ) ) ;
#22804 = CARTESIAN_POINT ( 'NONE',  ( -22.26937170471362748, 150.7043692363948537, 0.4001190995498107861 ) ) ;
#22805 = EDGE_LOOP ( 'NONE', ( #14798, #20190, #39365, #6719, #20816, #32395, #10537, #33448, #15005, #11826 ) ) ;
#22806 = CARTESIAN_POINT ( 'NONE',  ( 5.177913976931196594, 77.01756249999996840, 5.372100000000004094 ) ) ;
#22807 = EDGE_CURVE ( 'NONE', #450, #38156, #11528, .T. ) ;
#22808 = ORIENTED_EDGE ( 'NONE', *, *, #6349, .F. ) ;
#22809 = FACE_OUTER_BOUND ( 'NONE', #25581, .T. ) ;
#22810 = CARTESIAN_POINT ( 'NONE',  ( 2.631220017305710090, -15.63525587843500553, 5.668892982663133573 ) ) ;
#22811 = CARTESIAN_POINT ( 'NONE',  ( -20.44439181834797381, 148.1475078817917961, 1.665223645801947816 ) ) ;
#22812 = CARTESIAN_POINT ( 'NONE',  ( 6.847865590701471383, 118.2876074772933492, -0.8134140678991769180 ) ) ;
#22813 = ADVANCED_FACE ( 'NONE', ( #4844 ), #1229, .F. ) ;
#22814 = CARTESIAN_POINT ( 'NONE',  ( -4.609222696788063622, 3.091975128091568159, 0.4746723485708761459 ) ) ;
#22815 = CARTESIAN_POINT ( 'NONE',  ( 6.059261036833978764, 78.87450423423040036, 5.016499999999999737 ) ) ;
#22816 = VERTEX_POINT ( 'NONE', #37202 ) ;
#22817 = CARTESIAN_POINT ( 'NONE',  ( 2.407412430484044816E-32, 1.626303258728256651E-15, 0.000000000000000000 ) ) ;
#22818 = CARTESIAN_POINT ( 'NONE',  ( -0.007670926890914411475, 121.5961256765098284, 0.3838845493044711343 ) ) ;
#22819 =( NAMED_UNIT ( * ) SI_UNIT ( $, .STERADIAN. ) SOLID_ANGLE_UNIT ( ) );
#22820 = B_SPLINE_SURFACE_WITH_KNOTS ( 'NONE', 3, 1, ( 
 ( #6471, #19446 ),
 ( #2869, #3284 ),
 ( #15830, #29248 ),
 ( #92, #22834 ) ),
 .UNSPECIFIED., .F., .F., .F.,
 ( 4, 4 ),
 ( 2, 2 ),
 ( 0.000000000000000000, 0.6118630412642168670 ),
 ( 0.000000000000000000, 1.000000000000000000 ),
 .UNSPECIFIED. ) ;
#22821 = CARTESIAN_POINT ( 'NONE',  ( -0.8674473734594028151, 156.8926940187749324, 1.309446568524254673 ) ) ;
#22822 = CARTESIAN_POINT ( 'NONE',  ( 5.071597197228429721, 117.1436960276084278, 0.6009254234287543239 ) ) ;
#22823 = CARTESIAN_POINT ( 'NONE',  ( 18.88959041316438459, 148.1672603684278329, -1.723054188180887403 ) ) ;
#22824 = CARTESIAN_POINT ( 'NONE',  ( -18.34395142906178222, 131.7683309214445728, -2.187682908440787610 ) ) ;
#22825 = CARTESIAN_POINT ( 'NONE',  ( -58.60752282809816904, -0.1920500713008393978, -0.6598870774482961110 ) ) ;
#22826 = EDGE_LOOP ( 'NONE', ( #36938, #11108, #13298, #11728, #2425, #15040, #5272 ) ) ;
#22827 = CARTESIAN_POINT ( 'NONE',  ( 4.462286611852313456, 118.1590011982771244, -0.4284256476081526599 ) ) ;
#22828 = CARTESIAN_POINT ( 'NONE',  ( 13.64865021167016046, 134.2686865373913463, -0.6688813089635637921 ) ) ;
#22829 = VECTOR ( 'NONE', #2599, 1000.000000000000227 ) ;
#22830 = VERTEX_POINT ( 'NONE', #33179 ) ;
#22831 = CARTESIAN_POINT ( 'NONE',  ( -17.71853448156636901, 146.5573550606970628, -2.243325415855147664 ) ) ;
#22832 = CARTESIAN_POINT ( 'NONE',  ( 2.429471885602138670, -15.51652123318236676, 4.968198114871331228 ) ) ;
#22833 = CARTESIAN_POINT ( 'NONE',  ( -5.287127330377648704, 105.1224767669196183, -0.7827282581152339436 ) ) ;
#22834 = CARTESIAN_POINT ( 'NONE',  ( 5.106395947886037234, 78.95054594174946772, -5.392902600000141433 ) ) ;
#22835 = CARTESIAN_POINT ( 'NONE',  ( -4.852690634155996108, 117.6441829300342334, 0.9099436388107151608 ) ) ;
#22836 = CARTESIAN_POINT ( 'NONE',  ( 2.508893989683063541, 119.8406177399916714, 0.6723988897110715346 ) ) ;
#22837 = CARTESIAN_POINT ( 'NONE',  ( -46.70722035912341141, 25.99002130462735849, 1.524000028476692359 ) ) ;
#22838 = CARTESIAN_POINT ( 'NONE',  ( -4.559029627765868398, 31.49133049583988253, -0.6947656260628575220 ) ) ;
#22839 = CARTESIAN_POINT ( 'NONE',  ( 9.051149985088882133, 123.9289873439938674, 0.3396360471471667752 ) ) ;
#22840 = DIRECTION ( 'NONE',  ( -5.188838149069471174E-16, 1.699382548006136313E-16, 1.000000000000000000 ) ) ;
#22841 = CARTESIAN_POINT ( 'NONE',  ( -48.19617591663109124, 18.61566378669634503, -4.750300018642161781 ) ) ;
#22842 = CARTESIAN_POINT ( 'NONE',  ( -5.562698904337072925, 116.6986079444752846, -0.1401370167873323136 ) ) ;
#22843 = CARTESIAN_POINT ( 'NONE',  ( 4.799643950526473191, 115.7029491485453292, 1.472414092453835588 ) ) ;
#22844 = CARTESIAN_POINT ( 'NONE',  ( -46.61813330717926362, 26.15088526608503372, -1.277411791215423031 ) ) ;
#22845 = DIRECTION ( 'NONE',  ( -0.4849315768086535083, -0.8745520943968250194, -1.030032898892974695E-16 ) ) ;
#22846 = DIRECTION ( 'NONE',  ( -0.9998004120163609398, -4.016384292689130894E-17, -0.01997839162482749689 ) ) ;
#22847 = CARTESIAN_POINT ( 'NONE',  ( -5.871452009091383317, 65.30181249999996851, 5.016499999999999737 ) ) ;
#22848 = CARTESIAN_POINT ( 'NONE',  ( -4.074955089416341991, 118.2429491485453354, 0.1454234154749719787 ) ) ;
#22849 = CARTESIAN_POINT ( 'NONE',  ( -6.484670282503085616E-14, 71.97546620154574271, 3.533028205012241021E-29 ) ) ;
#22850 = CARTESIAN_POINT ( 'NONE',  ( -57.35225397299146977, 4.112755766825001658, 0.3099640861128158398 ) ) ;
#22851 = CIRCLE ( 'NONE', #26278, 0.2540000000000029456 ) ;
#22852 = CARTESIAN_POINT ( 'NONE',  ( -57.43854689232674815, 1.757847328446624058, 1.624773336220232789 ) ) ;
#22853 = CARTESIAN_POINT ( 'NONE',  ( -15.79392588796415353, 121.0087326939336378, -0.08323308591264573508 ) ) ;
#22854 = AXIS2_PLACEMENT_3D ( 'NONE', #39489, #36299, #17517 ) ;
#22855 = ORIENTED_EDGE ( 'NONE', *, *, #28953, .T. ) ;
#22856 = CARTESIAN_POINT ( 'NONE',  ( -53.65397596840620764, 15.31786685697163897, -0.6615342354324158514 ) ) ;
#22857 = AXIS2_PLACEMENT_3D ( 'NONE', #14064, #30052, #889 ) ;
#22858 = CARTESIAN_POINT ( 'NONE',  ( 6.071239300402657690, 121.4397587287365639, 0.1177787590444958898 ) ) ;
#22859 = ORIENTED_EDGE ( 'NONE', *, *, #38592, .T. ) ;
#22860 = DIRECTION ( 'NONE',  ( -5.188838149069472160E-16, 1.699382548006136559E-16, 1.000000000000000000 ) ) ;
#22861 = CARTESIAN_POINT ( 'NONE',  ( -8.071037755103120048, 122.8559727437779827, -0.2401247476687868587 ) ) ;
#22862 = CARTESIAN_POINT ( 'NONE',  ( 5.767107246999573889, -13.94705323133380048, 2.761945726399152701 ) ) ;
#22863 = CARTESIAN_POINT ( 'NONE',  ( -18.85936551755652246, 131.8417273817641444, 1.350502370828212673 ) ) ;
#22864 = CARTESIAN_POINT ( 'NONE',  ( 1.172031118611134874E-15, 12.17394877578616885, 0.000000000000000000 ) ) ;
#22865 = CARTESIAN_POINT ( 'NONE',  ( 23.25077945365668342, 149.0206351951634076, 0.9193108337986204415 ) ) ;
#22866 = CARTESIAN_POINT ( 'NONE',  ( 8.436454488239842675, 123.3184168920685551, 0.2537209124029990437 ) ) ;
#22867 = CARTESIAN_POINT ( 'NONE',  ( 5.065658811076494850, 115.6909491485453145, -1.197684230374509218 ) ) ;
#22868 = CARTESIAN_POINT ( 'NONE',  ( 0.8726510978149698561, 7.843753604616166442, 0.4398688123008435147 ) ) ;
#22869 = CARTESIAN_POINT ( 'NONE',  ( -23.08789804466238849, 149.8924475812327159, -0.6911741358207282859 ) ) ;
#22870 = CARTESIAN_POINT ( 'NONE',  ( -11.58677707360137532, 55.24499999999999034, 4.474811398758258285 ) ) ;
#22871 = EDGE_CURVE ( 'NONE', #9633, #12494, #20994, .T. ) ;
#22872 = CARTESIAN_POINT ( 'NONE',  ( 8.515285667870288113E-16, 8.844871939465425825, 0.000000000000000000 ) ) ;
#22873 = CARTESIAN_POINT ( 'NONE',  ( 2.765491355666962914, 117.1119770199604631, 0.6595734277189526651 ) ) ;
#22874 = ORIENTED_EDGE ( 'NONE', *, *, #38086, .T. ) ;
#22875 = CARTESIAN_POINT ( 'NONE',  ( -58.36964224452065508, -0.2912198378497423135, -0.01722170194331728438 ) ) ;
#22876 = CARTESIAN_POINT ( 'NONE',  ( 9.605778978211040098, 157.4977751962898083, 1.777432263976032711 ) ) ;
#22877 = CARTESIAN_POINT ( 'NONE',  ( 19.99643065938083453, 145.3736917597469471, -1.717600817134501634 ) ) ;
#22878 = CARTESIAN_POINT ( 'NONE',  ( 0.9680108232324700079, 2.729151709021603978, 0.1071397942825247085 ) ) ;
#22879 = CARTESIAN_POINT ( 'NONE',  ( -3.310625167495538257, 6.824969433126684137, -7.744297517547710896 ) ) ;
#22880 = CARTESIAN_POINT ( 'NONE',  ( -2.895878334088895834, 159.0164033662945258, -1.329837440140976046 ) ) ;
#22881 = CARTESIAN_POINT ( 'NONE',  ( 4.894174812879662717, 117.7423131706384112, -0.7196635720700498284 ) ) ;
#22882 = CARTESIAN_POINT ( 'NONE',  ( 13.70496720263909829, 119.6480011847203002, 0.2738578607179662505 ) ) ;
#22883 = CARTESIAN_POINT ( 'NONE',  ( 15.87656987697858746, 149.2064892436030163, -1.252469198948042539 ) ) ;
#22884 = CARTESIAN_POINT ( 'NONE',  ( -8.961118498053046721, 123.9105667600146177, -0.1452814789513759974 ) ) ;
#22885 = VERTEX_POINT ( 'NONE', #27606 ) ;
#22886 = CARTESIAN_POINT ( 'NONE',  ( -5.693059210196507181, 156.8407539676644546, -1.898889529600695569 ) ) ;
#22887 = CARTESIAN_POINT ( 'NONE',  ( 3.555926573287145231, -15.62149673449747489, 5.135790484437000814 ) ) ;
#22888 = TOROIDAL_SURFACE ( 'NONE', #17462, 3.111499999999999488, 0.2540000000000000036 ) ;
#22889 = CARTESIAN_POINT ( 'NONE',  ( -37.66124916107632714, 74.02712188174415076, 1.523999999999987587 ) ) ;
#22890 = CARTESIAN_POINT ( 'NONE',  ( -48.38589991294941939, 19.15920805527091630, -5.452675306770326635 ) ) ;
#22892 = ORIENTED_EDGE ( 'NONE', *, *, #12395, .F. ) ;
#22891 = AXIS2_PLACEMENT_3D ( 'NONE', #39659, #32841, #13872 ) ;
#22893 = CARTESIAN_POINT ( 'NONE',  ( -0.01081828683971087710, 119.3136608367422866, 0.5413913113077197803 ) ) ;
#22894 = DIRECTION ( 'NONE',  ( -4.017660918040594346E-17, 1.000000000000000000, 2.376309959284834438E-19 ) ) ;
#22895 = CARTESIAN_POINT ( 'NONE',  ( -3.467804978690799622, 119.7720183225874138, 0.4097519885510785276 ) ) ;
#22896 = CARTESIAN_POINT ( 'NONE',  ( -7.980626778564171353, 22.53057930515566554, 2.691543149341120156 ) ) ;
#22897 = CARTESIAN_POINT ( 'NONE',  ( 7.664053125822814394, 122.2986020547093915, 0.5896768268545022895 ) ) ;
#22898 = CARTESIAN_POINT ( 'NONE',  ( 8.125192968412290995, 117.9016134627522945, -0.4934282302770852113 ) ) ;
#22899 = EDGE_CURVE ( 'NONE', #11900, #20726, #13781, .T. ) ;
#22900 = CARTESIAN_POINT ( 'NONE',  ( -15.21260244842765630, 17.14499999999999957, 0.000000000000000000 ) ) ;
#22901 = CARTESIAN_POINT ( 'NONE',  ( -30.75918919842648336, 69.77432548395512413, -1.524000000000007793 ) ) ;
#22902 = CIRCLE ( 'NONE', #33828, 9.048749999999998295 ) ;
#22903 = EDGE_CURVE ( 'NONE', #38897, #6194, #14259, .T. ) ;
#22904 = CARTESIAN_POINT ( 'NONE',  ( -0.8920107295036362460, 116.4394364983335493, 0.02072182073814212572 ) ) ;
#22905 = ORIENTED_EDGE ( 'NONE', *, *, #38951, .F. ) ;
#22906 = CARTESIAN_POINT ( 'NONE',  ( -6.706889091645539480, 120.9727344454672107, -1.004351640261528900 ) ) ;
#22907 = CARTESIAN_POINT ( 'NONE',  ( 3.232439242213211994, -15.36757322000031145, 5.574794819488745112 ) ) ;
#22908 = AXIS2_PLACEMENT_3D ( 'NONE', #39763, #39972, #36764 ) ;
#22909 = CARTESIAN_POINT ( 'NONE',  ( -9.364230102553138479, 123.8909350679826815, -0.6996930829695081622 ) ) ;
#22910 = CARTESIAN_POINT ( 'NONE',  ( 3.231995002093183800, -14.34039573884512997, 4.866605245980782257 ) ) ;
#22911 = DIRECTION ( 'NONE',  ( -0.3256999990547897461, -0.9454731675810318370, 0.000000000000000000 ) ) ;
#22912 = CARTESIAN_POINT ( 'NONE',  ( 0.8860745468265911473, 116.4323782974132513, 0.03055428320029210734 ) ) ;
#22913 = ADVANCED_FACE ( 'NONE', ( #26987 ), #33598, .T. ) ;
#22914 = EDGE_LOOP ( 'NONE', ( #12946, #38564, #10568, #38128 ) ) ;
#22915 = CARTESIAN_POINT ( 'NONE',  ( -4.399545650080316506, 2.442302885307133131, -1.471791394725967095 ) ) ;
#22916 = CARTESIAN_POINT ( 'NONE',  ( -1.491112615444313949, 105.1235505628452387, 5.131223246399314597 ) ) ;
#22917 = DIRECTION ( 'NONE',  ( 0.3582377630123916856, -0.9336303900108853249, 3.445432962228668055E-16 ) ) ;
#22918 = LINE ( 'NONE', #9740, #22392 ) ;
#22919 = CIRCLE ( 'NONE', #39969, 0.2539999999999975056 ) ;
#22920 = CARTESIAN_POINT ( 'NONE',  ( -6.978456853209969779, 121.0120372305622567, 0.7589161456756378099 ) ) ;
#22921 = CARTESIAN_POINT ( 'NONE',  ( -3.586339569854333220, 7.474549112184489807, -2.913498476264247294 ) ) ;
#22922 = CARTESIAN_POINT ( 'NONE',  ( 17.57666534335605490, 125.1652531886817172, 1.391946913312248180 ) ) ;
#22923 = CARTESIAN_POINT ( 'NONE',  ( -48.16232371146166003, 19.02200717996782586, -5.227009030934667955 ) ) ;
#22925 = CARTESIAN_POINT ( 'NONE',  ( 11.94841889513447697, 120.7721054874162974, -1.107169436317064770 ) ) ;
#22924 = DIRECTION ( 'NONE',  ( -5.188838149069472160E-16, 1.699382548006136559E-16, 1.000000000000000000 ) ) ;
#22926 = CARTESIAN_POINT ( 'NONE',  ( -3.128764270554720728, 7.249652477310866594, -3.416742352092642321 ) ) ;
#22927 = CARTESIAN_POINT ( 'NONE',  ( -22.50793294095888797, 142.2972183020237367, -1.640122747091713906 ) ) ;
#22928 = ORIENTED_EDGE ( 'NONE', *, *, #16805, .F. ) ;
#22929 = EDGE_CURVE ( 'NONE', #26282, #40423, #19704, .T. ) ;
#22930 = CARTESIAN_POINT ( 'NONE',  ( -13.67682410656413516, 150.2105054413494543, 0.1652630162413761539 ) ) ;
#22931 = CARTESIAN_POINT ( 'NONE',  ( 6.168037961413951997, -13.40247527924742776, 1.492370457280242091 ) ) ;
#22932 = LINE ( 'NONE', #3597, #24078 ) ;
#22933 = CIRCLE ( 'NONE', #16841, 3.175000000000001155 ) ;
#22934 = CARTESIAN_POINT ( 'NONE',  ( -2.753942980615568192, 107.6238140763581441, -4.560544256597707680 ) ) ;
#22935 = ORIENTED_EDGE ( 'NONE', *, *, #17010, .T. ) ;
#22936 = EDGE_CURVE ( 'NONE', #296, #31875, #30379, .T. ) ;
#22937 = CARTESIAN_POINT ( 'NONE',  ( 8.537619249161298995, 156.7723266660784986, 2.072230564756332161 ) ) ;
#22938 = CARTESIAN_POINT ( 'NONE',  ( 12.69999999999999929, 17.14499999999999957, 1.555301434917138235E-15 ) ) ;
#22939 = CARTESIAN_POINT ( 'NONE',  ( -6.503981220335420706E-14, 66.64146620154573952, -9.408573323119121831E-18 ) ) ;
#22940 = CARTESIAN_POINT ( 'NONE',  ( -12.94589274040331439, 156.9034992427187376, 0.7570359663163894748 ) ) ;
#22941 = EDGE_CURVE ( 'NONE', #21011, #29590, #7821, .T. ) ;
#22942 = CARTESIAN_POINT ( 'NONE',  ( 11.57591774076040103, 118.7825156662901378, -0.1473217720007391485 ) ) ;
#22943 = PLANE ( 'NONE',  #34920 ) ;
#22944 = APPLICATION_CONTEXT ( 'automotive_design' ) ;
#22945 = CARTESIAN_POINT ( 'NONE',  ( -46.74369117050184741, 25.88875364612797725, 1.392958786023526185 ) ) ;
#22946 = CARTESIAN_POINT ( 'NONE',  ( -49.37240900658670739, 23.24656341648388036, 0.6295958749597029280 ) ) ;
#22947 = CARTESIAN_POINT ( 'NONE',  ( -4.973570852245686957, 117.3993868453976575, -0.9750598967993134858 ) ) ;
#22948 = EDGE_CURVE ( 'NONE', #17342, #41432, #24400, .T. ) ;
#22949 = CARTESIAN_POINT ( 'NONE',  ( -56.21344593158320180, 5.939860726778031896, 2.828251681716853927 ) ) ;
#22950 = CARTESIAN_POINT ( 'NONE',  ( -58.81783741892115103, -0.2724193165228563362, 0.09424156098961072869 ) ) ;
#22951 = CARTESIAN_POINT ( 'NONE',  ( -4.547585464732198268, 118.0892030396713039, 0.5918700655309280245 ) ) ;
#22952 = CARTESIAN_POINT ( 'NONE',  ( -58.37241122568488549, -0.2962816677227891882, -1.026553828834651941E-14 ) ) ;
#22953 = VERTEX_POINT ( 'NONE', #13982 ) ;
#22954 = EDGE_LOOP ( 'NONE', ( #5622, #35866, #7879, #1166 ) ) ;
#22955 = CARTESIAN_POINT ( 'NONE',  ( -2.168366069047774403, 118.7629491485468236, -1.225207463359169857 ) ) ;
#22956 = CARTESIAN_POINT ( 'NONE',  ( -8.375474303938146292, 119.6239881352457388, -1.418291987643603091 ) ) ;
#22957 = CARTESIAN_POINT ( 'NONE',  ( -6.891280466594768228, 121.8252198949890186, -0.2939903263561802760 ) ) ;
#22958 = CARTESIAN_POINT ( 'NONE',  ( 4.536752517374653237, 118.0323550597005209, 0.8638088581934265653 ) ) ;
#22959 = CARTESIAN_POINT ( 'NONE',  ( -46.95726096424718321, 25.94444535518948669, -0.08936005021616608146 ) ) ;
#22960 = CARTESIAN_POINT ( 'NONE',  ( -7.153290765950069741, 121.6016026263613838, -0.8513816870021353456 ) ) ;
#22961 = CARTESIAN_POINT ( 'NONE',  ( -4.299427874650186610, 115.7036758056284356, -1.546095265231658855 ) ) ;
#22962 = CARTESIAN_POINT ( 'NONE',  ( -14.53564353655538000, 79.78436006922240153, -1.524000000000001132 ) ) ;
#22963 = CARTESIAN_POINT ( 'NONE',  ( 5.267339127473229965, 116.4790307410953289, -0.8814195561379954968 ) ) ;
#22964 = CARTESIAN_POINT ( 'NONE',  ( -16.67506696845916991, 147.9788754379930822, -1.914365833524547256 ) ) ;
#22965 = CARTESIAN_POINT ( 'NONE',  ( 1.925929944387235853E-31, 3.469446951953614189E-15, 0.000000000000000000 ) ) ;
#22966 = CARTESIAN_POINT ( 'NONE',  ( -0.03245814172817860360, 158.1186941186938952, 1.624338139048501661 ) ) ;
#22967 = CARTESIAN_POINT ( 'NONE',  ( 7.819596425025786779, 122.5025573198914230, -0.1851469994925282470 ) ) ;
#22968 = CARTESIAN_POINT ( 'NONE',  ( -15.77235285888377270, 146.5682724429268262, -0.2480670253506113976 ) ) ;
#22969 = CARTESIAN_POINT ( 'NONE',  ( 4.574821423538755205, -2.080616851812391310, 0.6590154617212384824 ) ) ;
#22971 = ORIENTED_EDGE ( 'NONE', *, *, #8699, .F. ) ;
#22970 = CARTESIAN_POINT ( 'NONE',  ( 22.23561040172127434, 150.7043692363948537, 1.289434558007280129 ) ) ;
#22972 = CARTESIAN_POINT ( 'NONE',  ( -17.14500000000466784, 71.11999999999886768, -1.270000000000000684 ) ) ;
#22973 = CARTESIAN_POINT ( 'NONE',  ( 3.116032494879745762, -15.28226460877120374, 3.911124699519683556 ) ) ;
#22974 = CARTESIAN_POINT ( 'NONE',  ( -11.94919878421465675, 122.6721150436042223, 1.294096368778067996 ) ) ;
#22975 = CARTESIAN_POINT ( 'NONE',  ( -0.7398639285967090196, 8.776656789086558774, 0.6336005302938405581 ) ) ;
#22976 = CARTESIAN_POINT ( 'NONE',  ( -3.233108093638920266, 159.4494809562368971, -0.4325382840285660890 ) ) ;
#22977 = AXIS2_PLACEMENT_3D ( 'NONE', #37639, #21842, #21631 ) ;
#22978 = CARTESIAN_POINT ( 'NONE',  ( -0.06867543354984582959, -8.127513596672324425, -0.9731866935420671050 ) ) ;
#22979 = ORIENTED_EDGE ( 'NONE', *, *, #27378, .T. ) ;
#22980 = ADVANCED_FACE ( 'NONE', ( #10582 ), #20783, .F. ) ;
#22981 = ORIENTED_EDGE ( 'NONE', *, *, #26007, .T. ) ;
#22982 = CARTESIAN_POINT ( 'NONE',  ( -45.23155955595164812, 20.39474799592974463, 2.956275845755106157 ) ) ;
#22983 = CARTESIAN_POINT ( 'NONE',  ( 4.850755190080882073, 117.2937442104795593, 0.9187341308512859683 ) ) ;
#22984 = DIRECTION ( 'NONE',  ( 0.000000000000000000, 0.000000000000000000, 1.000000000000000000 ) ) ;
#22985 = CARTESIAN_POINT ( 'NONE',  ( -9.599121003648976469, 153.9312916436033447, 0.7969471826422134253 ) ) ;
#22986 = CARTESIAN_POINT ( 'NONE',  ( 3.649535173467634674, -14.21384370944696407, 4.751373335446510637 ) ) ;
#22987 = CARTESIAN_POINT ( 'NONE',  ( 17.34190353359454306, 148.5513402141484391, -1.530992562556359182 ) ) ;
#22988 = CARTESIAN_POINT ( 'NONE',  ( -12.85210230480898375, 122.5866728308148055, -1.831397601346916426 ) ) ;
#22989 = DIRECTION ( 'NONE',  ( 5.188838149069472160E-16, -1.699382548006136559E-16, -1.000000000000000000 ) ) ;
#22990 = CARTESIAN_POINT ( 'NONE',  ( 3.093198985275321444, -14.55695847870221193, 3.716444964235936066 ) ) ;
#22991 = CARTESIAN_POINT ( 'NONE',  ( -1.114473875789820934, 36.31367722304656809, -0.2353634988756889146 ) ) ;
#22992 = CARTESIAN_POINT ( 'NONE',  ( 1.582738162022832018, 156.2580631240469415, -0.1078144505905371531 ) ) ;
#22993 = ORIENTED_EDGE ( 'NONE', *, *, #28269, .T. ) ;
#22994 = CARTESIAN_POINT ( 'NONE',  ( -10.00099186598785650, 77.19260062651656540, 1.270000000000000684 ) ) ;
#22995 = CARTESIAN_POINT ( 'NONE',  ( 0.9967641087948266865, 106.0888231320409716, 5.244678224992261661 ) ) ;
#22996 = CARTESIAN_POINT ( 'NONE',  ( 18.35410564743290607, 77.35382415001784295, -1.904999999999999583 ) ) ;
#22997 = CARTESIAN_POINT ( 'NONE',  ( 11.41714695485569564, 57.14999999999999858, 5.016499999999999737 ) ) ;
#22998 = CARTESIAN_POINT ( 'NONE',  ( 5.750520748247040181, 159.1178304044242964, 0.06386070104996836860 ) ) ;
#22999 = ADVANCED_FACE ( 'NONE', ( #4635 ), #10789, .F. ) ;
#23000 = VECTOR ( 'NONE', #10402, 1000.000000000000114 ) ;
#23001 = CARTESIAN_POINT ( 'NONE',  ( -3.110646482806300739, 107.8085536575111689, 4.359277737140974551 ) ) ;
#23002 = ADVANCED_FACE ( 'NONE', ( #23769 ), #36024, .T. ) ;
#23003 = CARTESIAN_POINT ( 'NONE',  ( -4.459494944917585357, 115.6909491485452719, 1.361414471398195714 ) ) ;
#23004 = DIRECTION ( 'NONE',  ( -6.353134868986659519E-16, 1.000000000000000000, 0.000000000000000000 ) ) ;
#23005 = CARTESIAN_POINT ( 'NONE',  ( -4.457266160556883960, 31.52268539727636565, -0.7032076836091958327 ) ) ;
#23006 = CARTESIAN_POINT ( 'NONE',  ( 19.77411333694939088, 150.7280352275851101, 2.313572189391364109 ) ) ;
#23007 = CARTESIAN_POINT ( 'NONE',  ( -4.137704358559117779, 17.39492794009094823, -2.099109474953318788 ) ) ;
#23008 = CARTESIAN_POINT ( 'NONE',  ( -5.217102898550305845, -11.97038331068927342, -6.647077075081065267 ) ) ;
#23009 = CARTESIAN_POINT ( 'NONE',  ( -8.722122541997446632, 117.9971651243157424, -0.7652714498589991976 ) ) ;
#23010 = CARTESIAN_POINT ( 'NONE',  ( -0.3783624953764856969, 110.0486234891351245, -3.695659563127995373 ) ) ;
#23011 = LINE ( 'NONE', #41816, #18239 ) ;
#23012 = CARTESIAN_POINT ( 'NONE',  ( -1.146254217351140303, 106.2775121091388115, -5.162372565581046402 ) ) ;
#23013 = CARTESIAN_POINT ( 'NONE',  ( 2.498149781570049299, 104.6144662015456959, 4.129972621594562909 ) ) ;
#23014 = CARTESIAN_POINT ( 'NONE',  ( 4.203610184846851894, 17.99761390031315500, -1.968029828111186319 ) ) ;
#23015 = FACE_BOUND ( 'NONE', #1866, .T. ) ;
#23016 = CARTESIAN_POINT ( 'NONE',  ( -3.967884321586665042, 117.3993838589258019, -1.334270751278506362 ) ) ;
#23017 = CARTESIAN_POINT ( 'NONE',  ( 3.093198985275321444, -14.55695847870221193, 3.716444964235936066 ) ) ;
#23018 = CARTESIAN_POINT ( 'NONE',  ( 2.352838477949680929, 119.2037781873646622, -0.5921520780602625988 ) ) ;
#23019 = CARTESIAN_POINT ( 'NONE',  ( -5.842267051812750189, 117.1711376449269721, 0.3073735213368162800 ) ) ;
#23020 = LINE ( 'NONE', #2683, #35983 ) ;
#23021 = ORIENTED_EDGE ( 'NONE', *, *, #12352, .T. ) ;
#23022 = LINE ( 'NONE', #28600, #14779 ) ;
#23023 = ORIENTED_EDGE ( 'NONE', *, *, #9514, .F. ) ;
#23024 = CARTESIAN_POINT ( 'NONE',  ( -30.20416046766209561, 71.17241488000101413, 1.523999999999992028 ) ) ;
#23025 = CARTESIAN_POINT ( 'NONE',  ( 5.309364964326869440, -15.28511724905957969, 2.738662543889408774 ) ) ;
#23026 = CARTESIAN_POINT ( 'NONE',  ( -20.10795522872020058, 148.3334041379468715, 1.700709099906817956 ) ) ;
#23027 = CARTESIAN_POINT ( 'NONE',  ( 20.59913821282560420, 136.3738900553462372, -1.239205967624167570 ) ) ;
#23028 = CARTESIAN_POINT ( 'NONE',  ( -0.1020318426323372635, 30.30579279289823802, -0.9687052925327788166 ) ) ;
#23029 = CARTESIAN_POINT ( 'NONE',  ( -58.76039124197362185, -0.3072667177839057961, -0.2129973275852694858 ) ) ;
#23030 = ORIENTED_EDGE ( 'NONE', *, *, #39363, .T. ) ;
#23031 = CARTESIAN_POINT ( 'NONE',  ( -25.77058783747419213, 72.83664265955201245, 1.523999999999993804 ) ) ;
#23032 = CARTESIAN_POINT ( 'NONE',  ( 1.051265659380868689, 124.5996987749017109, 0.05046802306060386295 ) ) ;
#23033 = FILL_AREA_STYLE ('',( #35643 ) ) ;
#23034 = CARTESIAN_POINT ( 'NONE',  ( -11.73912714424001180, 153.3684197651487580, 1.370860710263250182 ) ) ;
#23035 = CARTESIAN_POINT ( 'NONE',  ( -43.55282894732439303, 21.75186528800919916, 2.470256908105690652 ) ) ;
#23036 = CARTESIAN_POINT ( 'NONE',  ( 0.01081828683957167594, 119.3136608367422866, -0.5413913113077197803 ) ) ;
#23037 = AXIS2_PLACEMENT_3D ( 'NONE', #15787, #25796, #29419 ) ;
#23038 = CARTESIAN_POINT ( 'NONE',  ( -1.153229101629017261, 158.8088198215516229, -1.472604719115122807 ) ) ;
#23039 = CARTESIAN_POINT ( 'NONE',  ( -57.71946847630993460, 1.146847591362354368, -1.351507486235954403 ) ) ;
#23040 = VERTEX_POINT ( 'NONE', #8023 ) ;
#23041 = CARTESIAN_POINT ( 'NONE',  ( 4.603039994573143723, 118.0757665291171037, -0.5234378334457231441 ) ) ;
#23042 = CARTESIAN_POINT ( 'NONE',  ( 9.648208730819460399, 124.2480737032941533, -0.3321887029122944091 ) ) ;
#23043 = ORIENTED_EDGE ( 'NONE', *, *, #19791, .F. ) ;
#23044 = CARTESIAN_POINT ( 'NONE',  ( -17.54535662205675450, 147.9903219242534078, -2.232389162988360543 ) ) ;
#23045 = CARTESIAN_POINT ( 'NONE',  ( 3.315889604118840150, -14.76599673617913488, 0.9486971755708663023 ) ) ;
#23046 = CARTESIAN_POINT ( 'NONE',  ( -22.46755768833301303, 150.8526571111528654, -0.4489552724284875951 ) ) ;
#23047 = CARTESIAN_POINT ( 'NONE',  ( 6.349999999999945466, 86.35999999999998522, 0.000000000000000000 ) ) ;
#23048 = CARTESIAN_POINT ( 'NONE',  ( 2.776928087254650013, 2.301956178644051221, 3.707541451904531105 ) ) ;
#23049 = CARTESIAN_POINT ( 'NONE',  ( 0.8144440842625040311, 156.8926940187749324, 1.343054762528750112 ) ) ;
#23050 = CARTESIAN_POINT ( 'NONE',  ( -3.046231754824817006, 31.09810386281187533, 0.4001267285823237874 ) ) ;
#23051 = ADVANCED_FACE ( 'NONE', ( #28237 ), #40794, .T. ) ;
#23052 = CARTESIAN_POINT ( 'NONE',  ( -4.507778648822867495, 31.37953541088120346, -1.025544427737863362 ) ) ;
#23053 = CARTESIAN_POINT ( 'NONE',  ( 11.85612367793081745, 151.9842433124228762, 0.4520816642129338314 ) ) ;
#23054 = FACE_OUTER_BOUND ( 'NONE', #36740, .T. ) ;
#23055 = AXIS2_PLACEMENT_3D ( 'NONE', #1276, #4264, #23608 ) ;
#23056 = CARTESIAN_POINT ( 'NONE',  ( -48.50421218116025557, 14.67712143704001626, -8.170758227952415863E-15 ) ) ;
#23057 = AXIS2_PLACEMENT_3D ( 'NONE', #33902, #36675, #23870 ) ;
#23058 = LINE ( 'NONE', #29474, #9864 ) ;
#23059 = DIRECTION ( 'NONE',  ( 2.731847993664264244E-14, -1.365923996832132122E-14, 1.000000000000000000 ) ) ;
#23060 = DIRECTION ( 'NONE',  ( 0.9998004120163608288, 0.000000000000000000, 0.01997839162482749342 ) ) ;
#23061 = CARTESIAN_POINT ( 'NONE',  ( -30.15519950990045572, 69.97033940222175374, -1.270000000000007123 ) ) ;
#23062 = CARTESIAN_POINT ( 'NONE',  ( -8.564670675228182262, 118.7243493509376435, -1.182334654099753468 ) ) ;
#23063 = CARTESIAN_POINT ( 'NONE',  ( -6.059261036834474368, 65.30181249999996851, 5.016499999999999737 ) ) ;
#23064 = CARTESIAN_POINT ( 'NONE',  ( -6.059261036834474368, 56.51499999999997925, 4.381499999999999950 ) ) ;
#23065 = CARTESIAN_POINT ( 'NONE',  ( -8.584014518950162653, 73.13423810798757074, 1.270000000000002460 ) ) ;
#23066 = CARTESIAN_POINT ( 'NONE',  ( -56.90927647567382763, 5.206763508130138440, 0.7605795637954813060 ) ) ;
#23067 = CARTESIAN_POINT ( 'NONE',  ( -56.65231406860745977, 4.194353530936431262, 2.518504496425231221 ) ) ;
#23068 = CARTESIAN_POINT ( 'NONE',  ( -22.63314285866090003, 150.6357905964555925, -0.1239933314926728036 ) ) ;
#23069 = ORIENTED_EDGE ( 'NONE', *, *, #28031, .F. ) ;
#23070 = CARTESIAN_POINT ( 'NONE',  ( -51.08083271936510528, 17.88738476406025057, -2.973263991802298278 ) ) ;
#23071 = CARTESIAN_POINT ( 'NONE',  ( 6.984995591253446712, 121.9529933140264575, 0.08165562821682262329 ) ) ;
#23072 = ORIENTED_EDGE ( 'NONE', *, *, #14420, .T. ) ;
#23073 = FACE_BOUND ( 'NONE', #7509, .T. ) ;
#23074 = CARTESIAN_POINT ( 'NONE',  ( -9.566940353391325758, 124.8108731098830049, -0.2265937611309800925 ) ) ;
#23075 = CARTESIAN_POINT ( 'NONE',  ( 4.196136289373067818, -14.93657984310306475, 5.004071965215434403 ) ) ;
#23076 = CARTESIAN_POINT ( 'NONE',  ( -0.4229338353208662582, 117.8786474493541050, 0.5307671053780920190 ) ) ;
#23077 = DIRECTION ( 'NONE',  ( 0.9998004120163608288, 0.000000000000000000, 0.01997839162482749342 ) ) ;
#23078 = CARTESIAN_POINT ( 'NONE',  ( 0.3088162040006633968, 116.5752054743899038, 0.1648661904198057415 ) ) ;
#23079 = CARTESIAN_POINT ( 'NONE',  ( 2.031162158012311370, -15.69476345269874074, 5.605913305253631407 ) ) ;
#23080 = CARTESIAN_POINT ( 'NONE',  ( 4.765335592615821625, 118.5266822147775940, -0.8412684598427435656 ) ) ;
#23081 = CARTESIAN_POINT ( 'NONE',  ( 0.9522911014763013604, -10.27702741150894994, -0.2247348558088197723 ) ) ;
#23082 = CARTESIAN_POINT ( 'NONE',  ( -8.209937203459384492, 117.5146787832509858, -0.2970838962712566977 ) ) ;
#23083 = CARTESIAN_POINT ( 'NONE',  ( 6.059261036833978764, 78.87450423423040036, 5.016499999999999737 ) ) ;
#23084 = FACE_OUTER_BOUND ( 'NONE', #38926, .T. ) ;
#23085 = ORIENTED_EDGE ( 'NONE', *, *, #28433, .T. ) ;
#23086 = CARTESIAN_POINT ( 'NONE',  ( 5.544339057385890612, 116.8028365428300361, 0.4221121198209883962 ) ) ;
#23087 = ORIENTED_EDGE ( 'NONE', *, *, #39685, .F. ) ;
#23088 = CARTESIAN_POINT ( 'NONE',  ( -4.293775319276113223, 119.8084884740358547, 0.7325880323699283103 ) ) ;
#23089 = CARTESIAN_POINT ( 'NONE',  ( -58.36967811586515609, -0.2912949152869354075, -0.01564362208030510917 ) ) ;
#23090 = CARTESIAN_POINT ( 'NONE',  ( 10.54454712121190951, 119.9085704333771787, 1.450830856784146139 ) ) ;
#23091 = CARTESIAN_POINT ( 'NONE',  ( 8.713776656587251424, 120.2102557752085232, -1.142027078586575595 ) ) ;
#23092 = CARTESIAN_POINT ( 'NONE',  ( -0.9360807938713975318, 7.254031735439380846, -0.2770855581244007215 ) ) ;
#23093 = CARTESIAN_POINT ( 'NONE',  ( -21.88420111187377870, 149.4141677464492091, -2.022441453707984227 ) ) ;
#23094 = CARTESIAN_POINT ( 'NONE',  ( 4.591938001951629822, 118.0392868320003714, -0.6629688387655557902 ) ) ;
#23095 = CARTESIAN_POINT ( 'NONE',  ( 10.08214312826198267, 118.0934564804968971, 0.2014652138697922978 ) ) ;
#23096 = AXIS2_PLACEMENT_3D ( 'NONE', #15983, #25785, #19391 ) ;
#23097 = CARTESIAN_POINT ( 'NONE',  ( 10.43918028506318940, 123.9810924921358151, -0.8290978625009025604 ) ) ;
#23098 = CARTESIAN_POINT ( 'NONE',  ( -6.503408402854686798, 121.7799126398724354, -0.1299535771408516782 ) ) ;
#23099 = ORIENTED_EDGE ( 'NONE', *, *, #27602, .T. ) ;
#23100 = CARTESIAN_POINT ( 'NONE',  ( 0.01081828683958208255, 119.3136608367422866, -0.5413913113077195582 ) ) ;
#23102 = CARTESIAN_POINT ( 'NONE',  ( 4.081004676854354862, -15.57459693632588760, 4.681182614216856663 ) ) ;
#23101 = VECTOR ( 'NONE', #35069, 1000.000000000000227 ) ;
#23103 = CARTESIAN_POINT ( 'NONE',  ( -14.38915334913366983, 80.27078028363496287, 1.269999999999998019 ) ) ;
#23104 = CARTESIAN_POINT ( 'NONE',  ( -46.25688858429101202, 20.73875112231587892, -4.700046123029353318 ) ) ;
#23105 = CARTESIAN_POINT ( 'NONE',  ( 11.70444740893354485, 123.2143981803894093, 1.719255905491489766 ) ) ;
#23106 = CARTESIAN_POINT ( 'NONE',  ( -1.114473875789821378, 36.31367722304657519, -0.2353634988756885538 ) ) ;
#23107 = CARTESIAN_POINT ( 'NONE',  ( -16.71197878298170991, 83.87086364642222236, -1.524000000000002686 ) ) ;
#23108 = CARTESIAN_POINT ( 'NONE',  ( -4.933025141172056927, 117.5302216577071874, 0.6666291745611304664 ) ) ;
#23109 = CARTESIAN_POINT ( 'NONE',  ( 6.556273983038449771, -14.34328088419217728, -5.323198733142235461 ) ) ;
#23110 = CARTESIAN_POINT ( 'NONE',  ( 9.476112355320449154, 124.1929984354129175, 0.6154534730440990309 ) ) ;
#23111 = CARTESIAN_POINT ( 'NONE',  ( 13.06303874853649738, 119.8917521002241955, -0.5243808535303263740 ) ) ;
#23112 = DIRECTION ( 'NONE',  ( 0.8745520943968249084, -0.4849315768086533418, 5.271987356194193006E-16 ) ) ;
#23113 = FACE_OUTER_BOUND ( 'NONE', #20049, .T. ) ;
#23114 = CARTESIAN_POINT ( 'NONE',  ( -6.439805278602227377E-14, 159.6054662015457382, 1.008550168686281963E-16 ) ) ;
#23115 = EDGE_LOOP ( 'NONE', ( #5124, #41976, #32331, #23984 ) ) ;
#23116 = CARTESIAN_POINT ( 'NONE',  ( 6.621162754568407749, 120.6004594848523226, -0.8446542950495584678 ) ) ;
#23117 = CARTESIAN_POINT ( 'NONE',  ( 23.11127252101355722, 149.9001116002701224, 0.4618182267416076070 ) ) ;
#23118 = CARTESIAN_POINT ( 'NONE',  ( -13.65930421665844641, 150.2105054413494543, -0.7115039165091185946 ) ) ;
#23119 = CARTESIAN_POINT ( 'NONE',  ( 3.097180478269691672, -14.43375334869456594, 4.992610980676636778 ) ) ;
#23120 = CARTESIAN_POINT ( 'NONE',  ( -0.008308726997795933336, 117.3658353995175503, 0.4158026747930030909 ) ) ;
#23121 = CARTESIAN_POINT ( 'NONE',  ( -33.20758249455312239, 49.81222039523557044, 1.523999999999993804 ) ) ;
#23122 = CARTESIAN_POINT ( 'NONE',  ( 2.743358099589752630, 116.5337465564440578, 0.09497135926289701491 ) ) ;
#23123 = ORIENTED_EDGE ( 'NONE', *, *, #4825, .T. ) ;
#23124 = CARTESIAN_POINT ( 'NONE',  ( 1.398650104629075797, 0.06838872207683838189, -4.420329592304430122 ) ) ;
#23125 = CARTESIAN_POINT ( 'NONE',  ( -0.1569751959820993303, 105.1223796759901177, 5.342321742714839949 ) ) ;
#23126 = CARTESIAN_POINT ( 'NONE',  ( -14.24929227862422465, 61.25037559889041461, -5.016500000000000625 ) ) ;
#23127 = CARTESIAN_POINT ( 'NONE',  ( -6.135835944515187101, 77.40800365160224317, -1.269999999999996243 ) ) ;
#23128 = CARTESIAN_POINT ( 'NONE',  ( -7.815079368384979297, 122.5103633090772064, 0.1576210380653273735 ) ) ;
#23129 = CARTESIAN_POINT ( 'NONE',  ( -4.468841950160419962, 8.124252568732815760, -1.173904233648782158 ) ) ;
#23130 = CARTESIAN_POINT ( 'NONE',  ( 1.281755300609836334, 159.3505072347868747, 0.9987438389826047702 ) ) ;
#23131 = DIRECTION ( 'NONE',  ( -0.5149185422762221354, 0.8572391118119440101, -4.128606161907601007E-16 ) ) ;
#23132 = CARTESIAN_POINT ( 'NONE',  ( 21.15257933310676108, 148.4376209648218321, -1.514591261405503708 ) ) ;
#23133 = CARTESIAN_POINT ( 'NONE',  ( 3.912982837994093188, 14.17146771520798332, -2.459658384584827218 ) ) ;
#23134 = CARTESIAN_POINT ( 'NONE',  ( -11.27775095430307140, 119.0414093155750379, -0.9684783378491814698 ) ) ;
#23135 = AXIS2_PLACEMENT_3D ( 'NONE', #13890, #4117, #16654 ) ;
#23136 = ORIENTED_EDGE ( 'NONE', *, *, #31794, .T. ) ;
#23137 = CARTESIAN_POINT ( 'NONE',  ( -8.770618086121094947, 123.6813396614493712, -0.1752578222716850986 ) ) ;
#23138 = CARTESIAN_POINT ( 'NONE',  ( -15.82110658236432776, 145.7390459690742830, 0.1389873312028087615 ) ) ;
#23139 = CARTESIAN_POINT ( 'NONE',  ( 2.112423120037338453, -15.42067558999450583, 5.959086572354191702 ) ) ;
#23140 = CONICAL_SURFACE ( 'NONE', #4823, 14.73199999999999577, 0.7853981633974488341 ) ;
#23141 = CARTESIAN_POINT ( 'NONE',  ( -18.88948446928058544, 80.17638627449419175, -1.524000000000003352 ) ) ;
#23142 = CARTESIAN_POINT ( 'NONE',  ( 2.906309357581933650, -13.72804873580029472, 0.7610837935892840189 ) ) ;
#23143 = VERTEX_POINT ( 'NONE', #5891 ) ;
#23144 = CARTESIAN_POINT ( 'NONE',  ( 2.460791562519470066, 158.0185616612000956, 1.723846131599015230 ) ) ;
#23145 = DIRECTION ( 'NONE',  ( -0.9998501190848636533, -0.01731298258487451447, -5.158639060800524920E-16 ) ) ;
#23146 = CARTESIAN_POINT ( 'NONE',  ( 14.16569067496491563, 138.8670163227227476, 0.2830642121559620583 ) ) ;
#23147 = CARTESIAN_POINT ( 'NONE',  ( -22.10675755583041635, 150.4421090420883900, 0.7299123522449004753 ) ) ;
#23148 = CARTESIAN_POINT ( 'NONE',  ( -8.392384909494198908, 27.87760190725155951, 0.4359655409547527616 ) ) ;
#23149 = EDGE_CURVE ( 'NONE', #5536, #4600, #41470, .T. ) ;
#23150 = CARTESIAN_POINT ( 'NONE',  ( 22.71658102202232854, 150.3666470947781022, -0.1371106802449218731 ) ) ;
#23151 =( BOUNDED_CURVE ( )  B_SPLINE_CURVE ( 3, ( #4053, #33436, #39831, #30013 ),
 .UNSPECIFIED., .F., .T. ) 
 B_SPLINE_CURVE_WITH_KNOTS ( ( 4, 4 ),
 ( 3.750906500318047510, 4.712388980384687898 ),
 .UNSPECIFIED. ) 
 CURVE ( )  GEOMETRIC_REPRESENTATION_ITEM ( )  RATIONAL_B_SPLINE_CURVE ( ( 1.000000000000000000, 0.9244349266169029633, 0.9244349266169029633, 1.000000000000000000 ) ) 
 REPRESENTATION_ITEM ( '' )  );
#23152 = CARTESIAN_POINT ( 'NONE',  ( -5.354045385558898751, 56.51499999999976609, -5.213862164400199894 ) ) ;
#23153 = CARTESIAN_POINT ( 'NONE',  ( -50.65446802363735657, 15.06743570032490176, 4.641860962342715169 ) ) ;
#23154 = CARTESIAN_POINT ( 'NONE',  ( -50.95401362087786623, 21.69085173448186055, 0.3723302588259275736 ) ) ;
#23155 = AXIS2_PLACEMENT_3D ( 'NONE', #11625, #5894, #18855 ) ;
#23156 = CARTESIAN_POINT ( 'NONE',  ( -4.962974768447578455, 117.4026934023842585, -1.029810944977519460 ) ) ;
#23157 = CARTESIAN_POINT ( 'NONE',  ( -48.65005484009959957, 18.46594748123760965, 5.297328305960426142 ) ) ;
#23158 = CARTESIAN_POINT ( 'NONE',  ( -5.586884702347496123, 85.69146620154573668, -0.1116392523995361624 ) ) ;
#23159 = CARTESIAN_POINT ( 'NONE',  ( -4.558231547695950958, 118.1058047250539005, 0.4915253113856153377 ) ) ;
#23160 = DIRECTION ( 'NONE',  ( 0.000000000000000000, 1.000000000000000000, 0.000000000000000000 ) ) ;
#23161 = B_SPLINE_SURFACE_WITH_KNOTS ( 'NONE', 5, 3, ( 
 ( #32220, #38413, #15595, #29010 ),
 ( #42029, #12621, #39240, #3470 ),
 ( #35415, #12825, #15803, #38821 ),
 ( #6659, #29439, #28811, #9225 ),
 ( #25813, #26024, #41827, #35213 ),
 ( #25609, #22600, #29222, #35631 ),
 ( #63, #9422, #13033, #39032 ),
 ( #9840, #22806, #35844, #3897 ) ),
 .UNSPECIFIED., .F., .F., .F.,
 ( 6, 2, 6 ),
 ( 4, 4 ),
 ( 0.000000000000000000, 0.5000000000000000000, 1.000000000000000000 ),
 ( -0.002373312499999995218, 0.03277393749999999578 ),
 .UNSPECIFIED. ) ;
#23162 = ORIENTED_EDGE ( 'NONE', *, *, #3533, .T. ) ;
#23163 = CARTESIAN_POINT ( 'NONE',  ( -42.72397600927682504, 22.83316142988638831, 1.683267422954620063 ) ) ;
#23164 = CARTESIAN_POINT ( 'NONE',  ( -3.727707540449571866, 118.8936418977788634, -0.9337890276463987060 ) ) ;
#23165 = CARTESIAN_POINT ( 'NONE',  ( -5.211883163658477258, 116.1034411669277375, -1.237845179234434045 ) ) ;
#23167 = CARTESIAN_POINT ( 'NONE',  ( 4.521618879414620373, 118.0718733995298066, 0.8081141274518772732 ) ) ;
#23166 = CIRCLE ( 'NONE', #33398, 0.6350000000000001199 ) ;
#23168 = CARTESIAN_POINT ( 'NONE',  ( -5.192366003377138384, 121.0352659167314755, -0.5503205103620255612 ) ) ;
#23169 = CARTESIAN_POINT ( 'NONE',  ( -1.791851930664796644, 115.7029402959327911, -1.723146288102838986 ) ) ;
#23170 = CARTESIAN_POINT ( 'NONE',  ( -5.177913976931298734, 78.94499979771843812, -5.372100000000003206 ) ) ;
#23171 = CARTESIAN_POINT ( 'NONE',  ( 5.498174961348566647, 117.5088849381099436, -0.6086507346144034436 ) ) ;
#23172 = CARTESIAN_POINT ( 'NONE',  ( -14.96631152213295479, 150.5987129668814077, -1.974168424754894957 ) ) ;
#23173 = CARTESIAN_POINT ( 'NONE',  ( 4.304052292061569140, 104.6144662015457385, -3.992357259174772466 ) ) ;
#23174 = CARTESIAN_POINT ( 'NONE',  ( -0.03066982525788228969, 157.3074135339440147, 1.534843470138540722 ) ) ;
#23175 = DIRECTION ( 'NONE',  ( -0.6675346791887244446, 0.7445787077807199950, 3.626530295975567369E-14 ) ) ;
#23176 = CARTESIAN_POINT ( 'NONE',  ( -7.540585633152407041, 122.4256904137044302, -0.07081817902877589332 ) ) ;
#23177 = CARTESIAN_POINT ( 'NONE',  ( 4.586363120317823672, -1.655842793181455663, -0.6244342276643227718 ) ) ;
#23178 = CARTESIAN_POINT ( 'NONE',  ( 20.97948398557565497, 132.3427885975763161, 1.200284224572990777 ) ) ;
#23179 = CARTESIAN_POINT ( 'NONE',  ( -5.719305292821792008, 76.92870498041706639, -1.269999999999995799 ) ) ;
#23180 = CARTESIAN_POINT ( 'NONE',  ( 3.071204355543858178, -15.18643405355604692, 3.901769932616943493 ) ) ;
#23181 = CARTESIAN_POINT ( 'NONE',  ( -19.00012635448491594, 147.0452383304005082, 1.727400128179960026 ) ) ;
#23182 = CARTESIAN_POINT ( 'NONE',  ( -0.1482875670852983607, 5.528424516503947395, -0.9633795868741713564 ) ) ;
#23183 = CARTESIAN_POINT ( 'NONE',  ( -15.83212890848034426, 121.4040080620525117, -0.8411940925737089181 ) ) ;
#23184 = CARTESIAN_POINT ( 'NONE',  ( -0.9630862182390291792, 27.11985920190685917, 0.1463314843619143713 ) ) ;
#23185 = EDGE_CURVE ( 'NONE', #1265, #26041, #21398, .T. ) ;
#23186 = ORIENTED_EDGE ( 'NONE', *, *, #39378, .T. ) ;
#23187 = CARTESIAN_POINT ( 'NONE',  ( -45.58494389689082738, 18.10922195552005221, 0.2974575429725789255 ) ) ;
#23188 = CARTESIAN_POINT ( 'NONE',  ( 5.246142718657039516, 116.7267603939287426, 1.018146482794727747 ) ) ;
#23189 = DIRECTION ( 'NONE',  ( 0.000000000000000000, 0.000000000000000000, 1.000000000000000000 ) ) ;
#23190 = CARTESIAN_POINT ( 'NONE',  ( -15.92216882203272377, 147.6644253265642135, 0.6463398217596320050 ) ) ;
#23191 = CARTESIAN_POINT ( 'NONE',  ( 4.301541689408341362, -12.13840576482722078, 1.420409876116004222 ) ) ;
#23192 = CARTESIAN_POINT ( 'NONE',  ( 10.76607124212182498, 123.2317624570580534, -1.067040512904773752 ) ) ;
#23193 = CARTESIAN_POINT ( 'NONE',  ( -11.06681148537632353, 121.4866960210745503, -1.697623966824489461 ) ) ;
#23194 = CARTESIAN_POINT ( 'NONE',  ( -4.429613830441260447, 104.6144662015457527, 1.943785857760518043 ) ) ;
#23195 = AXIS2_PLACEMENT_3D ( 'NONE', #30701, #17913, #2177 ) ;
#23196 = CARTESIAN_POINT ( 'NONE',  ( 3.211984996733021624, -14.06435921420946755, 2.432701253525752172 ) ) ;
#23197 = CARTESIAN_POINT ( 'NONE',  ( -6.125448292536311179, 31.19746429541880772, 1.780260802209707949 ) ) ;
#23198 = CARTESIAN_POINT ( 'NONE',  ( 4.580760836099185163, 121.1907927009877000, 0.02326454623414945036 ) ) ;
#23199 = ORIENTED_EDGE ( 'NONE', *, *, #677, .F. ) ;
#23200 = CARTESIAN_POINT ( 'NONE',  ( -5.232920286240068108, 115.9100003722636956, 1.117763783589812432 ) ) ;
#23201 = CARTESIAN_POINT ( 'NONE',  ( -0.1065207248106947446, 105.8844037013955983, 5.332933549509751181 ) ) ;
#23202 = VECTOR ( 'NONE', #30820, 1000.000000000000000 ) ;
#23203 = LINE ( 'NONE', #7058, #22505 ) ;
#23204 = EDGE_CURVE ( 'NONE', #31017, #2334, #37164, .T. ) ;
#23205 = CARTESIAN_POINT ( 'NONE',  ( -29.81357423954495189, 70.62209452652477637, 1.269999999999991802 ) ) ;
#23206 = CARTESIAN_POINT ( 'NONE',  ( 0.001838942458788770306, 116.4858755864912183, -0.09202820039585830891 ) ) ;
#23207 = CARTESIAN_POINT ( 'NONE',  ( -5.103137870717271873, 114.3519703858145959, 1.758966173294684854 ) ) ;
#23208 = CIRCLE ( 'NONE', #39582, 0.2539999999999998925 ) ;
#23209 = DIRECTION ( 'NONE',  ( -5.188838149069472160E-16, 1.699382548006136559E-16, 1.000000000000000000 ) ) ;
#23210 = DIRECTION ( 'NONE',  ( -0.9998004120163609398, 0.000000000000000000, -0.01997839162482749689 ) ) ;
#23211 = CARTESIAN_POINT ( 'NONE',  ( -1.543289776211116626, 35.18841652350401006, 0.2515601095814950505 ) ) ;
#23212 = EDGE_CURVE ( 'NONE', #23250, #28134, #8152, .T. ) ;
#23213 = CARTESIAN_POINT ( 'NONE',  ( 13.54337464129331714, 122.2126086331852974, 1.756000464972328867 ) ) ;
#23214 = CARTESIAN_POINT ( 'NONE',  ( -1.512449008193210931, 25.81601926892489018, -4.382106060783010903 ) ) ;
#23215 = CARTESIAN_POINT ( 'NONE',  ( -8.302162399154521921, -10.86525386290528594, -1.555404731216454284 ) ) ;
#23216 = CARTESIAN_POINT ( 'NONE',  ( -5.532489265500688980, 117.9651905194339605, -1.089543468331991116 ) ) ;
#23217 = CARTESIAN_POINT ( 'NONE',  ( -3.074626428557295732, 123.1875568577169560, -0.1788317054798707617 ) ) ;
#23218 = CARTESIAN_POINT ( 'NONE',  ( -5.555120986090559931, 78.91530963298718859, 5.093895734005253750 ) ) ;
#23219 = AXIS2_PLACEMENT_3D ( 'NONE', #24233, #2100, #21239 ) ;
#23220 = CARTESIAN_POINT ( 'NONE',  ( 17.14499999999999957, 71.11999999999999034, -5.016499999999999737 ) ) ;
#23221 = CARTESIAN_POINT ( 'NONE',  ( -1.607155361308500563, 104.6144662015456959, 4.551785039662791021 ) ) ;
#23222 = AXIS2_PLACEMENT_3D ( 'NONE', #36310, #16900, #29902 ) ;
#23223 = CARTESIAN_POINT ( 'NONE',  ( 1.325333094648095011, 19.28447512809159292, -4.440015753949128730 ) ) ;
#23224 = CARTESIAN_POINT ( 'NONE',  ( -47.35944255389382107, 21.37623662739424191, -4.722871667523179440 ) ) ;
#23225 = DIRECTION ( 'NONE',  ( -0.1565721916418034432, -0.9876665170007953298, 8.659954811667511346E-17 ) ) ;
#23226 = CARTESIAN_POINT ( 'NONE',  ( 3.226040172055379518, -13.73821525131127608, 2.149215086980220235 ) ) ;
#23227 = CARTESIAN_POINT ( 'NONE',  ( 2.102284131448346027, 122.9394440205640961, -0.1126375150955781085 ) ) ;
#23228 = CARTESIAN_POINT ( 'NONE',  ( -14.24059674577823387, 120.4756499382577886, 0.4587616384891654575 ) ) ;
#23229 = CARTESIAN_POINT ( 'NONE',  ( 4.922801907822831780, 117.4099815471397363, -0.9489923651248427516 ) ) ;
#23230 = ORIENTED_EDGE ( 'NONE', *, *, #36703, .F. ) ;
#23231 = DIRECTION ( 'NONE',  ( -0.8745520943968243532, 0.4849315768086547296, -6.829619984160642269E-16 ) ) ;
#23232 = ORIENTED_EDGE ( 'NONE', *, *, #35246, .T. ) ;
#23233 = CARTESIAN_POINT ( 'NONE',  ( -5.204863647155245410, 115.7029491485453576, 1.024056704596592038 ) ) ;
#23234 = CARTESIAN_POINT ( 'NONE',  ( 2.719191112037562252, -15.71471113085404170, 5.040136806425350002 ) ) ;
#23235 = CARTESIAN_POINT ( 'NONE',  ( -20.39294766749442900, 148.4497675966422889, 1.664483663417329895 ) ) ;
#23236 = CARTESIAN_POINT ( 'NONE',  ( 12.48318382086454115, 120.3283006479967128, -0.8937555771000558202 ) ) ;
#23237 = CARTESIAN_POINT ( 'NONE',  ( -4.595132424582489605, -6.828429371805166959, -0.5093739664528403877 ) ) ;
#23238 = ADVANCED_FACE ( 'NONE', ( #28452 ), #2487, .F. ) ;
#23239 = CARTESIAN_POINT ( 'NONE',  ( -58.62437260890455093, -0.2808582271535189356, -0.3920676774944526488 ) ) ;
#23240 = EDGE_LOOP ( 'NONE', ( #17390, #24896, #25410, #33146 ) ) ;
#23241 = FACE_OUTER_BOUND ( 'NONE', #20482, .T. ) ;
#23242 = CARTESIAN_POINT ( 'NONE',  ( 1.058386756517223137, 124.8229041592835387, 0.03077316225166111877 ) ) ;
#23243 = CARTESIAN_POINT ( 'NONE',  ( -14.75676393591426816, 134.6798445586954927, 1.238239479614488214 ) ) ;
#23244 = CARTESIAN_POINT ( 'NONE',  ( -6.350000000000036060, 57.78499999999998948, 7.776507174585692163E-16 ) ) ;
#23245 = EDGE_CURVE ( 'NONE', #15805, #21511, #10182, .T. ) ;
#23246 = CARTESIAN_POINT ( 'NONE',  ( 18.41704236485550439, 146.8095856830544790, -1.664602135862215393 ) ) ;
#23247 = CARTESIAN_POINT ( 'NONE',  ( -20.91063213905309937, 147.8517002469272370, -2.402771019925620255 ) ) ;
#23248 = CARTESIAN_POINT ( 'NONE',  ( -58.43690671596436914, -0.4125963578781866037, -1.035377653829272970E-14 ) ) ;
#23249 = ADVANCED_FACE ( 'NONE', ( #8861 ), #31857, .T. ) ;
#23250 = VERTEX_POINT ( 'NONE', #11622 ) ;
#23251 = CARTESIAN_POINT ( 'NONE',  ( 4.407527007107042039, 118.1629860519386881, -0.4885628053013030825 ) ) ;
#23252 = CARTESIAN_POINT ( 'NONE',  ( 3.022581645176192211, 156.1079525116674631, -0.4343475099915217741 ) ) ;
#23253 = ORIENTED_EDGE ( 'NONE', *, *, #19933, .F. ) ;
#23254 = CARTESIAN_POINT ( 'NONE',  ( -8.183297913989086680, 121.2453320564195280, -1.294587653635731916 ) ) ;
#23255 = CARTESIAN_POINT ( 'NONE',  ( 1.980066450162843106, -15.31690195035381663, 5.269506609478212589 ) ) ;
#23256 = CARTESIAN_POINT ( 'NONE',  ( 2.447805105500874934, 105.1245809240877662, -4.785117320943135688 ) ) ;
#23257 = CIRCLE ( 'NONE', #14415, 2.540000000000000480 ) ;
#23258 = CARTESIAN_POINT ( 'NONE',  ( -58.33992048227231209, -0.2288887037933118318, 0.2155571079148066727 ) ) ;
#23259 = CARTESIAN_POINT ( 'NONE',  ( -2.065029617914060367, 6.824861272777455135, -4.134893973632223663 ) ) ;
#23260 = CARTESIAN_POINT ( 'NONE',  ( 3.657622835216417290, 156.7231754051992425, 1.598616135119148352 ) ) ;
#23261 = CARTESIAN_POINT ( 'NONE',  ( -0.3625295811786362621, 32.83794214056845107, 1.283952373590488305 ) ) ;
#23262 = CARTESIAN_POINT ( 'NONE',  ( -2.359559261509405204, 14.11188314818778267, 3.974389579228013503 ) ) ;
#23263 = CARTESIAN_POINT ( 'NONE',  ( 6.494557633019020670, 121.7745328324513139, 0.2023806202038008484 ) ) ;
#23264 = LINE ( 'NONE', #33734, #39219 ) ;
#23265 = AXIS2_PLACEMENT_3D ( 'NONE', #9203, #37962, #41379 ) ;
#23266 = CARTESIAN_POINT ( 'NONE',  ( -53.95448410595108157, 8.335714161839828051, -2.220323970834214844 ) ) ;
#23267 = CARTESIAN_POINT ( 'NONE',  ( 5.177913976931196594, 78.94499979771845233, 5.372100000000001430 ) ) ;
#23268 = CARTESIAN_POINT ( 'NONE',  ( -2.026290786761661522, 117.3993837374443672, 1.369916322765275529 ) ) ;
#23269 = DIRECTION ( 'NONE',  ( -0.1906721105965040186, 0.9816537812491095139, -2.657572025465703189E-16 ) ) ;
#23270 = DIRECTION ( 'NONE',  ( -0.9998004120163610509, -4.016384292689131511E-17, -0.01997839162482749689 ) ) ;
#23271 = CARTESIAN_POINT ( 'NONE',  ( -6.194847070882102180, 64.72978607931611350, -1.269999999999994023 ) ) ;
#23272 = LINE ( 'NONE', #29689, #20489 ) ;
#23273 = CARTESIAN_POINT ( 'NONE',  ( -4.074955089416341991, 118.2429491485453354, 0.1454234154749719787 ) ) ;
#23274 = CARTESIAN_POINT ( 'NONE',  ( -5.106395947886143816, 78.95054594174945350, -1.904999999999999583 ) ) ;
#23275 = CARTESIAN_POINT ( 'NONE',  ( -58.21785149106106871, 1.559091779220117546, 0.3785645914142855561 ) ) ;
#23276 = CARTESIAN_POINT ( 'NONE',  ( -57.80205714066466527, 2.371715784325115095, 1.753227392946289598 ) ) ;
#23277 = CARTESIAN_POINT ( 'NONE',  ( -21.39485547647985086, 132.5159896776619917, -0.01683271311856767219 ) ) ;
#23278 = EDGE_CURVE ( 'NONE', #29922, #35053, #18808, .T. ) ;
#23279 = ORIENTED_EDGE ( 'NONE', *, *, #13097, .T. ) ;
#23280 = CARTESIAN_POINT ( 'NONE',  ( -57.84788464146735265, 2.520999533240836143, -0.7145982302433674382 ) ) ;
#23281 = CARTESIAN_POINT ( 'NONE',  ( 7.796796354633476867, 122.5849000957118022, -0.007570717282985798234 ) ) ;
#23282 = ORIENTED_EDGE ( 'NONE', *, *, #26151, .T. ) ;
#23283 = CARTESIAN_POINT ( 'NONE',  ( 3.636484375549583259, 115.7029495056428487, -1.480734918736348105 ) ) ;
#23284 = CARTESIAN_POINT ( 'NONE',  ( -13.59043555108506851, 150.2357272821285221, -0.3212980696657036783 ) ) ;
#23285 = CARTESIAN_POINT ( 'NONE',  ( 5.669917404453804544, -14.04548127125972101, 2.990483579271598469 ) ) ;
#23286 = CARTESIAN_POINT ( 'NONE',  ( -2.840063763404333308, 158.7847427699215928, 1.391859091975727658 ) ) ;
#23287 = CARTESIAN_POINT ( 'NONE',  ( 4.203610184846851894, 17.99761390031315500, -1.968029828111186541 ) ) ;
#23288 = CIRCLE ( 'NONE', #36243, 0.2539999999999962288 ) ;
#23289 = CARTESIAN_POINT ( 'NONE',  ( 5.814470848032661898, 117.0573985505404693, 0.4185731406947919009 ) ) ;
#23290 = CARTESIAN_POINT ( 'NONE',  ( 2.303556031286093653, -15.40459834138439810, 5.802045920756290442 ) ) ;
#23291 = CARTESIAN_POINT ( 'NONE',  ( -29.26089923143846860, 65.68766220334288164, 1.269999999999992912 ) ) ;
#23292 = CARTESIAN_POINT ( 'NONE',  ( 0.9725752971277935588, -10.50039532299128808, -0.08436647605774086345 ) ) ;
#23293 = CARTESIAN_POINT ( 'NONE',  ( -5.792301705315751725, 116.9567987913546006, -0.2385690759321333065 ) ) ;
#23294 = CARTESIAN_POINT ( 'NONE',  ( -10.28897677580358305, 56.51499999999998636, 4.381500000000000838 ) ) ;
#23295 = DIRECTION ( 'NONE',  ( -0.3256999990547864710, -0.9454731675810330582, 1.399154850856895850E-16 ) ) ;
#23296 = ORIENTED_EDGE ( 'NONE', *, *, #9552, .F. ) ;
#23297 = CARTESIAN_POINT ( 'NONE',  ( 8.731230164061564381, 117.9563494393051144, 0.7283447773125311109 ) ) ;
#23298 = ORIENTED_EDGE ( 'NONE', *, *, #38816, .T. ) ;
#23299 = CARTESIAN_POINT ( 'NONE',  ( -12.33128838443264463, 153.5964916033214820, 1.587645809864455471 ) ) ;
#23300 = CARTESIAN_POINT ( 'NONE',  ( -57.58831721485822186, 1.394338577185886274, -1.315253866661476367 ) ) ;
#23301 = CARTESIAN_POINT ( 'NONE',  ( 17.69400247866221321, 128.5843929717815115, 1.987683303373968702 ) ) ;
#23302 = CARTESIAN_POINT ( 'NONE',  ( 12.91500497980660178, 122.5866728308148055, -1.316509475493082171 ) ) ;
#23303 = CARTESIAN_POINT ( 'NONE',  ( 0.9007433063219677516, 2.300345052497278608, 0.3717552062572989091 ) ) ;
#23304 = CARTESIAN_POINT ( 'NONE',  ( -21.61975215418298291, 149.3076860495818323, -2.139488579489918774 ) ) ;
#23305 = CARTESIAN_POINT ( 'NONE',  ( 4.587194918930014964, 118.0383489642607913, -0.6670231109234234790 ) ) ;
#23306 = VECTOR ( 'NONE', #32518, 1000.000000000000000 ) ;
#23307 = EDGE_CURVE ( 'NONE', #38115, #28439, #21067, .T. ) ;
#23308 = AXIS2_PLACEMENT_3D ( 'NONE', #28263, #24635, #12076 ) ;
#23309 = EDGE_CURVE ( 'NONE', #20396, #5931, #2731, .T. ) ;
#23310 = CARTESIAN_POINT ( 'NONE',  ( 4.803469898345580802, 156.0326374431741385, -1.047298710704739122 ) ) ;
#23311 = CARTESIAN_POINT ( 'NONE',  ( -2.888995153171277419, 156.0927491134738716, -0.02440385714215712737 ) ) ;
#23312 = ORIENTED_EDGE ( 'NONE', *, *, #17586, .F. ) ;
#23313 = CARTESIAN_POINT ( 'NONE',  ( -18.63996327081357052, 147.1333978507680627, -2.447832456508666432 ) ) ;
#23314 = CARTESIAN_POINT ( 'NONE',  ( 4.914263517198875775, -15.39432152949170352, 0.3857354017804055513 ) ) ;
#23315 = CARTESIAN_POINT ( 'NONE',  ( -4.556757383386185190, 31.49269130883712720, -0.6906699653381264126 ) ) ;
#23316 = CARTESIAN_POINT ( 'NONE',  ( -4.575423324728332020, 118.0775249002766003, -0.7112773029818583170 ) ) ;
#23317 = CARTESIAN_POINT ( 'NONE',  ( -52.50198181065980663, 11.96455506022023307, -4.263607785004590589 ) ) ;
#23318 = CARTESIAN_POINT ( 'NONE',  ( -30.50798996576767763, 65.61473877417354572, 1.523999999999992694 ) ) ;
#23319 = CARTESIAN_POINT ( 'NONE',  ( 11.19992112824918706, 154.5781333488962446, 2.119767339128326267 ) ) ;
#23320 = LINE ( 'NONE', #781, #16104 ) ;
#23321 = AXIS2_PLACEMENT_3D ( 'NONE', #26340, #32744, #3577 ) ;
#23322 = CARTESIAN_POINT ( 'NONE',  ( 23.11127252101355722, 149.9001116002701224, 0.4618182267416076070 ) ) ;
#23323 = CIRCLE ( 'NONE', #38313, 0.7620000000000000107 ) ;
#23324 = CARTESIAN_POINT ( 'NONE',  ( -1.660137282266059611, 14.53371390510571004, 8.268994913937449454 ) ) ;
#23325 = CARTESIAN_POINT ( 'NONE',  ( 13.34275001191896415, 134.1388935151753401, 0.9731691531512426385 ) ) ;
#23326 = CARTESIAN_POINT ( 'NONE',  ( 20.57308965805791701, 132.2049894596293313, -0.6677571715933801055 ) ) ;
#23327 = DIRECTION ( 'NONE',  ( 0.9963166110440661027, 0.000000000000000000, -0.08575086330566526749 ) ) ;
#23328 = ORIENTED_EDGE ( 'NONE', *, *, #36023, .T. ) ;
#23329 = CARTESIAN_POINT ( 'NONE',  ( 0.6575858438756917446, 118.7629491485454025, 1.273916485320598202 ) ) ;
#23330 = CIRCLE ( 'NONE', #12499, 5.588000000000006295 ) ;
#23331 = CARTESIAN_POINT ( 'NONE',  ( -5.755666581048902941, 159.1151184437813981, -0.09834937626042344894 ) ) ;
#23332 = ORIENTED_EDGE ( 'NONE', *, *, #17820, .F. ) ;
#23333 = CARTESIAN_POINT ( 'NONE',  ( 6.848188653798881198, 121.3878566068075173, -0.5633949501833540596 ) ) ;
#23334 = CARTESIAN_POINT ( 'NONE',  ( -4.518622368304341386, 75.45558079800476037, 1.524000000000004462 ) ) ;
#23335 = CARTESIAN_POINT ( 'NONE',  ( -15.79012389680301709, 146.9282941555416073, -0.7681517710631363682 ) ) ;
#23336 = CARTESIAN_POINT ( 'NONE',  ( 4.218352450475082449, -13.04292013931325478, 2.887648331721151873 ) ) ;
#23337 = CARTESIAN_POINT ( 'NONE',  ( -20.93040400792228795, 136.4823663107028722, 1.114867025985508464 ) ) ;
#23338 = DIRECTION ( 'NONE',  ( -0.9998004120163609398, 0.000000000000000000, -0.01997839162482749689 ) ) ;
#23339 = CARTESIAN_POINT ( 'NONE',  ( 1.417643301182374582, 159.6052071245950970, 0.07209812905978400799 ) ) ;
#23340 = EDGE_LOOP ( 'NONE', ( #3832, #39362, #32720, #24175 ) ) ;
#23341 = CARTESIAN_POINT ( 'NONE',  ( -1.861891798414337940, 1.167894131763866250, -4.247245584637167504 ) ) ;
#23342 = CARTESIAN_POINT ( 'NONE',  ( -23.45208337669183152, 146.8499405026647651, -0.4686284387228153991 ) ) ;
#23343 = CARTESIAN_POINT ( 'NONE',  ( -23.91048590848665611, 81.84235438443283783, -1.270000000000006235 ) ) ;
#23344 = CARTESIAN_POINT ( 'NONE',  ( -6.434551728065664555, 119.5454990110429065, 1.003392985923742931 ) ) ;
#23345 = EDGE_CURVE ( 'NONE', #31840, #38617, #20015, .T. ) ;
#23346 = CARTESIAN_POINT ( 'NONE',  ( 1.583070580811935191, 1.852152477310867074, 4.353984577079609508 ) ) ;
#23347 = CARTESIAN_POINT ( 'NONE',  ( 14.52885936862946004, 121.1548589120785095, 1.307706137645302302 ) ) ;
#23348 = CARTESIAN_POINT ( 'NONE',  ( -57.20860189791900297, 2.757428422320434613, -2.041684569451241327 ) ) ;
#23350 = CARTESIAN_POINT ( 'NONE',  ( 13.70042256495996824, 122.3361261571837986, -1.218568937077757042 ) ) ;
#23349 = DIRECTION ( 'NONE',  ( 0.9998004120163609398, 4.016384292689130894E-17, 0.01997839162482749689 ) ) ;
#23351 = AXIS2_PLACEMENT_3D ( 'NONE', #8215, #5045, #1840 ) ;
#23352 = CARTESIAN_POINT ( 'NONE',  ( -0.3558933743640902425, 1.202427940091101100, 4.626034787239965418 ) ) ;
#23353 = CARTESIAN_POINT ( 'NONE',  ( -20.20545065706726717, 152.4988772720997190, -1.451042778694937363 ) ) ;
#23354 = EDGE_CURVE ( 'NONE', #32592, #17039, #12708, .T. ) ;
#23355 = ORIENTED_EDGE ( 'NONE', *, *, #356, .F. ) ;
#23356 = VECTOR ( 'NONE', #37633, 1000.000000000000114 ) ;
#23357 = CARTESIAN_POINT ( 'NONE',  ( -15.85578974452678658, 145.9541952667573810, 0.1379097727432557485 ) ) ;
#23358 = CARTESIAN_POINT ( 'NONE',  ( 2.083301838685661878, -15.46665383083971257, 5.961979448439955753 ) ) ;
#23359 = CARTESIAN_POINT ( 'NONE',  ( -42.19606231239161787, 22.08888036620040296, 1.545000424059492339 ) ) ;
#23360 = CIRCLE ( 'NONE', #20654, 0.6350000000000014522 ) ;
#23361 = CARTESIAN_POINT ( 'NONE',  ( -1.903537964721656151, 106.6614287958324354, -4.980401174282360621 ) ) ;
#23362 = ORIENTED_EDGE ( 'NONE', *, *, #25053, .T. ) ;
#23363 = CARTESIAN_POINT ( 'NONE',  ( 13.39306239354261407, 123.7870877700634509, 1.917211633051635333 ) ) ;
#23364 = CARTESIAN_POINT ( 'NONE',  ( -17.14500000000466784, 71.11999999999886768, 1.269999999999998241 ) ) ;
#23365 = VECTOR ( 'NONE', #33718, 1000.000000000000000 ) ;
#23366 = DIRECTION ( 'NONE',  ( 0.9998004120163608288, 0.000000000000000000, 0.01997839162482760791 ) ) ;
#23367 = CARTESIAN_POINT ( 'NONE',  ( -14.96085986107159016, 121.2513550155162960, 0.6271060280491598249 ) ) ;
#23368 = CARTESIAN_POINT ( 'NONE',  ( -4.534963259934312596, 26.26729952004485824, -7.114490783490484027 ) ) ;
#23369 = CARTESIAN_POINT ( 'NONE',  ( 5.855671506236596713, 121.0368588677253143, 0.7388637662663295469 ) ) ;
#23370 = CARTESIAN_POINT ( 'NONE',  ( 4.803851041827788215, 116.9482543694763166, -0.2466672064845015777 ) ) ;
#23371 = CARTESIAN_POINT ( 'NONE',  ( -23.43300365160793319, 82.12916405548841681, 1.269999999999994023 ) ) ;
#23372 = CARTESIAN_POINT ( 'NONE',  ( -48.76205491696826044, 18.14848438229189753, 5.115617678642917276 ) ) ;
#23373 = CARTESIAN_POINT ( 'NONE',  ( -49.85168879002940656, 22.56840098298264152, 0.7122439767497134033 ) ) ;
#23374 = CARTESIAN_POINT ( 'NONE',  ( 2.104948366110713565, 106.4601199789983212, -4.917459751093059772 ) ) ;
#23375 = CARTESIAN_POINT ( 'NONE',  ( -55.11216289415786207, 6.786895728730008237, 3.177266426849158609 ) ) ;
#23376 = CARTESIAN_POINT ( 'NONE',  ( -58.24081614096904502, 0.5413803788780069404, 1.084122344208306332 ) ) ;
#23377 = CARTESIAN_POINT ( 'NONE',  ( -4.432033464645024345, 118.1653844686336186, 0.4638121791032019381 ) ) ;
#23378 = CARTESIAN_POINT ( 'NONE',  ( -17.14500000000466784, 71.11999999999886768, 1.269999999999998241 ) ) ;
#23379 = ORIENTED_EDGE ( 'NONE', *, *, #37045, .T. ) ;
#23380 = CARTESIAN_POINT ( 'NONE',  ( -4.722993557843548018, 118.7629491485454309, -0.9938571727007795564 ) ) ;
#23381 = CARTESIAN_POINT ( 'NONE',  ( 6.146672433393463031, 119.5348080636299954, -1.011818472031234206 ) ) ;
#23382 = CARTESIAN_POINT ( 'NONE',  ( -5.262805716460127847, 116.4520502601644409, -1.094458988799881682 ) ) ;
#23383 = CARTESIAN_POINT ( 'NONE',  ( 4.596454834243283827, 118.0615255785435949, 0.7279963062917687022 ) ) ;
#23384 = CARTESIAN_POINT ( 'NONE',  ( -11.86571527151352612, 128.3619849303985632, -1.073981288313974991 ) ) ;
#23385 = TOROIDAL_SURFACE ( 'NONE', #21348, 3.683000000000000718, 0.5080000000000000071 ) ;
#23386 = CARTESIAN_POINT ( 'NONE',  ( -0.9706191444543458280, 115.7029418442419484, -1.748960127381335994 ) ) ;
#23387 = CARTESIAN_POINT ( 'NONE',  ( 2.557047726870576465, 118.1651003891136185, -0.7232189756707855244 ) ) ;
#23388 = CARTESIAN_POINT ( 'NONE',  ( 4.861212978143112373, 112.7561542417671916, -2.378900599183503051 ) ) ;
#23389 = CARTESIAN_POINT ( 'NONE',  ( -7.227551859934705725, 121.2980461901665308, -1.025750885112893585 ) ) ;
#23390 = CARTESIAN_POINT ( 'NONE',  ( -5.336395407662996249, 116.0444662015457169, 0.06658830643601890142 ) ) ;
#23391 = CARTESIAN_POINT ( 'NONE',  ( -0.03153870137021549253, 158.4432089348667319, 1.578325583784928376 ) ) ;
#23392 = CARTESIAN_POINT ( 'NONE',  ( 8.207314164617031338, 120.6877426416259738, -1.076149196205714587 ) ) ;
#23393 = CARTESIAN_POINT ( 'NONE',  ( -15.77438986758538242, 146.5666090065403466, -0.1139034878652071398 ) ) ;
#23394 = CARTESIAN_POINT ( 'NONE',  ( 4.634220987317881679, -1.855718946426311078, -0.01876340930339078644 ) ) ;
#23395 = CARTESIAN_POINT ( 'NONE',  ( 5.539025187978692699, 159.0643023895801491, 0.7880117631591502247 ) ) ;
#23396 = DIRECTION ( 'NONE',  ( -5.188838149069471174E-16, 1.699382548006136313E-16, 1.000000000000000000 ) ) ;
#23397 = CARTESIAN_POINT ( 'NONE',  ( 2.352443540978347958, -15.20488079220741540, 4.935102241435597392 ) ) ;
#23398 = CIRCLE ( 'NONE', #29538, 12.69999999999999751 ) ;
#23399 = CARTESIAN_POINT ( 'NONE',  ( -3.316780243214269230, 119.1333808041459577, 0.7607270569537705196 ) ) ;
#23400 = CARTESIAN_POINT ( 'NONE',  ( 0.6087277426107279288, -8.065848283227245119, 0.7602462886992925606 ) ) ;
#23401 = CARTESIAN_POINT ( 'NONE',  ( -21.25299977426499609, 132.4531229209162575, -0.9669248719381910995 ) ) ;
#23402 = CARTESIAN_POINT ( 'NONE',  ( -0.7739057699295280868, 27.87760190725158083, 0.5882008851359883383 ) ) ;
#23403 = VERTEX_POINT ( 'NONE', #22041 ) ;
#23404 = EDGE_CURVE ( 'NONE', #24559, #13560, #25478, .T. ) ;
#23405 = CARTESIAN_POINT ( 'NONE',  ( -41.93982928939168175, 22.21638423992008882, 1.241790202385180342 ) ) ;
#23406 = CARTESIAN_POINT ( 'NONE',  ( 2.902940568641189323, 107.8364052097302306, 4.470325690468442303 ) ) ;
#23407 = CARTESIAN_POINT ( 'NONE',  ( -12.35517153206337149, 152.0262389575480881, 0.8038591168380521124 ) ) ;
#23408 = CARTESIAN_POINT ( 'NONE',  ( 4.310348487322937849, -12.41951052373176090, 1.878555342735434230 ) ) ;
#23409 = CARTESIAN_POINT ( 'NONE',  ( 12.55519531044855697, 126.0212559692275249, -1.204658208757142246 ) ) ;
#23410 = AXIS2_PLACEMENT_3D ( 'NONE', #28537, #24915, #31515 ) ;
#23411 = CARTESIAN_POINT ( 'NONE',  ( -6.111605970564546020, 157.2590385278250267, -1.959406070573513459 ) ) ;
#23412 = FACE_OUTER_BOUND ( 'NONE', #13463, .T. ) ;
#23413 = CARTESIAN_POINT ( 'NONE',  ( 2.107392885931908211, -15.11054218480166433, 5.236909061670549370 ) ) ;
#23414 = CARTESIAN_POINT ( 'NONE',  ( -4.910297347208772756, 117.4773399772923170, -1.095285516455568375 ) ) ;
#23415 = CARTESIAN_POINT ( 'NONE',  ( 15.75440288366313268, 145.7063497038720925, 0.08391657230255397670 ) ) ;
#23416 = ORIENTED_EDGE ( 'NONE', *, *, #27215, .T. ) ;
#23417 = CARTESIAN_POINT ( 'NONE',  ( 1.650612623617701257E-15, 17.14499999999999957, 0.000000000000000000 ) ) ;
#23418 = FACE_OUTER_BOUND ( 'NONE', #11149, .T. ) ;
#23419 = SHAPE_REPRESENTATION ( 'Base Ring', ( #3275 ), #9399 ) ;
#23420 = DIRECTION ( 'NONE',  ( 5.188838149069472160E-16, -1.699382548006136559E-16, -1.000000000000000000 ) ) ;
#23421 = DIRECTION ( 'NONE',  ( 1.000000000000000000, 6.353134868986659519E-16, 0.000000000000000000 ) ) ;
#23422 = CARTESIAN_POINT ( 'NONE',  ( 23.20816695139192021, 149.6253602407241488, 0.3098579641399932250 ) ) ;
#23423 = CARTESIAN_POINT ( 'NONE',  ( -5.379991719817741824, 116.9256180743815179, 0.7442756809649816452 ) ) ;
#23424 = CARTESIAN_POINT ( 'NONE',  ( 1.741439286752546556, -15.57054322800294166, 5.502057211990651453 ) ) ;
#23425 = CARTESIAN_POINT ( 'NONE',  ( 14.39766717389552042, 12.96416000000000146, -1.904999999999999583 ) ) ;
#23426 = CARTESIAN_POINT ( 'NONE',  ( -5.010339283552668554, 117.3993855393351566, -0.7509198670801209285 ) ) ;
#23427 = CARTESIAN_POINT ( 'NONE',  ( 20.74782508767430755, 148.9555414352193168, 2.393722347598511657 ) ) ;
#23428 = CARTESIAN_POINT ( 'NONE',  ( 4.610398055573782905, 23.01736123548795021, -0.3254830233858732602 ) ) ;
#23429 = CARTESIAN_POINT ( 'NONE',  ( -4.329333532990936817, 10.85900946394830413, -7.254296797256971630 ) ) ;
#23430 = CARTESIAN_POINT ( 'NONE',  ( -2.454038931915638599, 117.4443284220410533, -0.7335733216053069716 ) ) ;
#23431 = CARTESIAN_POINT ( 'NONE',  ( -0.3093948633800919779, 109.1907409294041429, -4.022046774707581207 ) ) ;
#23432 = CARTESIAN_POINT ( 'NONE',  ( -5.571852488405353299, 78.91397923090406152, 5.086862008547728742 ) ) ;
#23433 = DIRECTION ( 'NONE',  ( -0.9998004120163608288, 0.000000000000000000, -0.01997839162482747608 ) ) ;
#23434 = CARTESIAN_POINT ( 'NONE',  ( -0.006734421712100887789, 121.9236798544229003, 0.3370180007451228366 ) ) ;
#23435 = CARTESIAN_POINT ( 'NONE',  ( -1.861891798414337940, 1.167894131763866250, -4.247245584637167504 ) ) ;
#23436 = CARTESIAN_POINT ( 'NONE',  ( -28.69846420587789737, 77.20784726182124302, 1.269999999999991580 ) ) ;
#23437 = DIRECTION ( 'NONE',  ( -0.3256999990547844170, -0.9454731675810337244, -8.328397965206681691E-18 ) ) ;
#23438 = CARTESIAN_POINT ( 'NONE',  ( 2.821697343786723877, -14.64683725402170289, 4.582568527534213843 ) ) ;
#23439 = CARTESIAN_POINT ( 'NONE',  ( 4.022785008250933991, 122.0441497943765370, -0.1183375255305477575 ) ) ;
#23440 = CARTESIAN_POINT ( 'NONE',  ( -7.827178552123696065, 158.6358315003295161, 0.5664908120210209175 ) ) ;
#23441 = ADVANCED_FACE ( 'NONE', ( #5684 ), #5053, .F. ) ;
#23442 = CARTESIAN_POINT ( 'NONE',  ( 4.999258502396517478, 117.4056799841109466, -0.8307607214361057979 ) ) ;
#23443 = CARTESIAN_POINT ( 'NONE',  ( -13.79703500197643073, 79.79115557309579287, 1.523999999999998911 ) ) ;
#23444 = ORIENTED_EDGE ( 'NONE', *, *, #19844, .F. ) ;
#23445 = CARTESIAN_POINT ( 'NONE',  ( -4.855072294470597072, 115.7029491485453718, 1.279409886141102071 ) ) ;
#23446 = CARTESIAN_POINT ( 'NONE',  ( 2.005403748902764516, -15.69871118693741430, 5.609036204238825540 ) ) ;
#23447 = CARTESIAN_POINT ( 'NONE',  ( -5.005942668485581670, 118.7197616721209670, 0.8869178833313973165 ) ) ;
#23448 = CARTESIAN_POINT ( 'NONE',  ( 19.13467844095158199, 131.8899703912256314, -1.275959715510668779 ) ) ;
#23449 = CARTESIAN_POINT ( 'NONE',  ( 0.9754839647580387796, 27.70931421350951496, 0.02445524045744520980 ) ) ;
#23450 = ADVANCED_FACE ( 'NONE', ( #31213 ), #29711, .T. ) ;
#23451 = CARTESIAN_POINT ( 'NONE',  ( -58.54066364324206972, -0.1080589709450771596, -0.6031363701337029148 ) ) ;
#23452 = VERTEX_POINT ( 'NONE', #16071 ) ;
#23453 = CARTESIAN_POINT ( 'NONE',  ( -4.973569738608247803, 117.3993868453981548, -0.9750659555622913643 ) ) ;
#23454 = CARTESIAN_POINT ( 'NONE',  ( 1.733652500133013197, 120.5851793143259130, 0.4713357653683603044 ) ) ;
#23455 = FILL_AREA_STYLE_COLOUR ( '', #21626 ) ;
#23456 = CARTESIAN_POINT ( 'NONE',  ( -10.16557698404471921, 154.1059161911440469, 1.245122368702753946 ) ) ;
#23457 = CARTESIAN_POINT ( 'NONE',  ( 3.070829792790402024, 118.0750053011746985, 0.9656202980712693673 ) ) ;
#23458 = CARTESIAN_POINT ( 'NONE',  ( 14.24002733280059374, 152.6618899727951089, -1.673933364105638866 ) ) ;
#23459 = CARTESIAN_POINT ( 'NONE',  ( -13.08065502438839189, 121.7804325175133755, -1.718327614618424315 ) ) ;
#23460 = CARTESIAN_POINT ( 'NONE',  ( -27.59695233663404679, 58.25262445104075226, -1.270000000000004015 ) ) ;
#23461 = ORIENTED_EDGE ( 'NONE', *, *, #33952, .T. ) ;
#23462 = CARTESIAN_POINT ( 'NONE',  ( 4.252665683302173427, 118.2250214913236448, -0.3074501678815576566 ) ) ;
#23463 = ADVANCED_FACE ( 'NONE', ( #16284 ), #10113, .T. ) ;
#23464 = CARTESIAN_POINT ( 'NONE',  ( 3.658657848224157405, 120.8687762150871379, -0.2216941123881816522 ) ) ;
#23465 = ORIENTED_EDGE ( 'NONE', *, *, #22936, .F. ) ;
#23466 = CARTESIAN_POINT ( 'NONE',  ( 3.405374690515594605, -14.89039384781155917, 1.812165507210882209 ) ) ;
#23467 = CARTESIAN_POINT ( 'NONE',  ( 5.314256983240370324, 105.1224655745845382, -0.4585143440169748841 ) ) ;
#23468 = CARTESIAN_POINT ( 'NONE',  ( -58.35999251409275246, -0.2710268728049192166, 0.1245515173811342219 ) ) ;
#23469 = AXIS2_PLACEMENT_3D ( 'NONE', #40444, #11236, #11439 ) ;
#23470 = CARTESIAN_POINT ( 'NONE',  ( 4.309711357183296343, 3.151582320728117725, 1.677628897243969464 ) ) ;
#23472 = EDGE_CURVE ( 'NONE', #5073, #22768, #38883, .T. ) ;
#23471 = CARTESIAN_POINT ( 'NONE',  ( 10.31823449898706180, 154.1877054190025262, 1.778048316349531310 ) ) ;
#23473 = CARTESIAN_POINT ( 'NONE',  ( 0.5299325911148425883, 33.81561889908242335, 0.8798404401248783868 ) ) ;
#23474 = CARTESIAN_POINT ( 'NONE',  ( 2.488009491785908800, 18.85968022696138391, -3.895047602898422223 ) ) ;
#23475 = CARTESIAN_POINT ( 'NONE',  ( 8.071037755102992151, 122.8559727437779827, 0.2401247476687870253 ) ) ;
#23476 = CARTESIAN_POINT ( 'NONE',  ( -3.495814013870744308, 108.2588365649876607, 4.019948443012803629 ) ) ;
#23477 = EDGE_CURVE ( 'NONE', #16450, #4948, #41883, .T. ) ;
#23478 = CARTESIAN_POINT ( 'NONE',  ( -52.67395729902614221, 10.59333423579336753, -2.513629069394799576 ) ) ;
#23479 = CARTESIAN_POINT ( 'NONE',  ( 5.562754537904068819, 116.7283259021707806, -0.08022358443418030338 ) ) ;
#23480 = CARTESIAN_POINT ( 'NONE',  ( -0.03519895179131819068, 115.7029491485452866, 1.761499482103557446 ) ) ;
#23481 = DIRECTION ( 'NONE',  ( 0.9816537812491126225, 0.1906721105964872265, 8.537024980200846470E-16 ) ) ;
#23482 = DIRECTION ( 'NONE',  ( -5.188838149069472160E-16, 1.699382548006136559E-16, 1.000000000000000000 ) ) ;
#23483 = CARTESIAN_POINT ( 'NONE',  ( -29.42319995514127839, 68.34872547565998957, -1.524000000000006905 ) ) ;
#23484 = EDGE_CURVE ( 'NONE', #11121, #2591, #29505, .T. ) ;
#23485 = CARTESIAN_POINT ( 'NONE',  ( -5.353961914030953118, 56.51499999999979451, 5.213928161110560566 ) ) ;
#23486 = CARTESIAN_POINT ( 'NONE',  ( -17.14500000000466784, 71.11999999999886768, -1.270000000000000684 ) ) ;
#23487 = CARTESIAN_POINT ( 'NONE',  ( -57.84788464146735265, 2.520999533240836143, 0.7145982302433464550 ) ) ;
#23488 = CARTESIAN_POINT ( 'NONE',  ( -58.60752282809816904, -0.1920500713008393978, 0.6598870774482750168 ) ) ;
#23489 = CARTESIAN_POINT ( 'NONE',  ( -23.34493312772039175, 146.7646281656787437, -0.007662864037405678515 ) ) ;
#23490 = ORIENTED_EDGE ( 'NONE', *, *, #28512, .F. ) ;
#23491 = CARTESIAN_POINT ( 'NONE',  ( -55.74683331106318462, 9.129907917338066170, -0.4890489271862362708 ) ) ;
#23492 = CARTESIAN_POINT ( 'NONE',  ( 6.064603996746924075, 121.4401124717423528, 0.1114288923163564010 ) ) ;
#23493 = ORIENTED_EDGE ( 'NONE', *, *, #11533, .T. ) ;
#23494 = DIRECTION ( 'NONE',  ( -0.8745520943967999283, 0.4849315768086988609, -5.424246918827959078E-16 ) ) ;
#23495 = CARTESIAN_POINT ( 'NONE',  ( 0.0005023639977569234428, 120.9974662015457056, -0.02514034870427536705 ) ) ;
#23496 = CARTESIAN_POINT ( 'NONE',  ( 6.473144302699227026, -13.19137087452153168, 0.2309683151692971392 ) ) ;
#23497 = CARTESIAN_POINT ( 'NONE',  ( -20.65103440377624011, 150.0789294893613999, 1.463288793709878854 ) ) ;
#23498 = CARTESIAN_POINT ( 'NONE',  ( -0.1328416520900886078, 24.48205809745167372, 4.627450821846854190 ) ) ;
#23499 = CARTESIAN_POINT ( 'NONE',  ( 10.73501234801821802, 157.9381345072164038, 0.5669044750022473877 ) ) ;
#23500 = CARTESIAN_POINT ( 'NONE',  ( 10.38578193225963275, 153.1602398435892383, 0.3880091275358500402 ) ) ;
#23501 = CARTESIAN_POINT ( 'NONE',  ( 3.979181138743986601, 26.09377549647152961, 2.406711837290479661 ) ) ;
#23502 = CARTESIAN_POINT ( 'NONE',  ( 0.8800754956866637668, -0.3565347152210476267, -0.4212773433312864690 ) ) ;
#23503 = CARTESIAN_POINT ( 'NONE',  ( -16.82892344227272474, 155.2408147041404050, -0.5439083615366221425 ) ) ;
#23504 = DIRECTION ( 'NONE',  ( -0.8745520943968250194, 0.4849315768086532863, -5.361993529360574930E-16 ) ) ;
#23505 = CARTESIAN_POINT ( 'NONE',  ( 4.962228190351918755, 117.4046759642803863, 1.029882822851095892 ) ) ;
#23506 = AXIS2_PLACEMENT_3D ( 'NONE', #31691, #31475, #37871 ) ;
#23507 = CARTESIAN_POINT ( 'NONE',  ( -5.551989495070855263, 116.9209052717933446, 0.3361809518408999664 ) ) ;
#23508 = CARTESIAN_POINT ( 'NONE',  ( -3.413396786258182658, 119.6896249646678569, 0.6770706109030820707 ) ) ;
#23509 = CARTESIAN_POINT ( 'NONE',  ( -57.95255339509083825, 0.6073592009028576655, -0.9201367675222190678 ) ) ;
#23510 = CARTESIAN_POINT ( 'NONE',  ( 20.86684145051964734, 149.6610172957225586, 2.296701127946504606 ) ) ;
#23511 = CARTESIAN_POINT ( 'NONE',  ( 5.880668475635486558, 119.2401804501882197, -0.9647153462086464071 ) ) ;
#23512 = CARTESIAN_POINT ( 'NONE',  ( -0.4938630982110026046, -9.903502963049303887, 0.8462501600425517134 ) ) ;
#23513 = CARTESIAN_POINT ( 'NONE',  ( -12.12330053995824741, 120.5818589831333441, -1.513795679345424361 ) ) ;
#23514 = CARTESIAN_POINT ( 'NONE',  ( 4.668726057213791414, 118.0244701076749436, -0.5694989693638285999 ) ) ;
#23515 = CARTESIAN_POINT ( 'NONE',  ( -47.00787117332040310, 24.49876931072293829, -2.333946431867834015 ) ) ;
#23516 = CARTESIAN_POINT ( 'NONE',  ( 4.831188462585346954, 104.6144662015456959, 0.2218974364397717225 ) ) ;
#23517 = CARTESIAN_POINT ( 'NONE',  ( 6.522410937005443721, 121.2869106855140018, -0.5334890203407732789 ) ) ;
#23518 = DIRECTION ( 'NONE',  ( 5.463695987328526437E-16, -1.000000000000000000, -1.672774450599033775E-31 ) ) ;
#23519 = ORIENTED_EDGE ( 'NONE', *, *, #11106, .F. ) ;
#23520 = CARTESIAN_POINT ( 'NONE',  ( -5.832110448082723941, 156.9788419092994047, -1.931507550941140572 ) ) ;
#23521 = CARTESIAN_POINT ( 'NONE',  ( 2.422525963563016749, -15.70080278133445617, 5.253054914258033392 ) ) ;
#23522 = CARTESIAN_POINT ( 'NONE',  ( -10.28897677580358305, 57.14999999999998437, 5.016499999999999737 ) ) ;
#23523 = CARTESIAN_POINT ( 'NONE',  ( -4.571919090563273613, 118.0413024280605043, -0.8379947033858301531 ) ) ;
#23524 = CARTESIAN_POINT ( 'NONE',  ( -53.83456308493991571, 9.379524109395250164, -3.755176697756441140 ) ) ;
#23525 = ADVANCED_FACE ( 'NONE', ( #6097 ), #9286, .T. ) ;
#23526 = CARTESIAN_POINT ( 'NONE',  ( 13.85159022459153988, 57.78500000000000369, -5.016500000000005066 ) ) ;
#23527 = B_SPLINE_SURFACE_WITH_KNOTS ( 'NONE', 3, 3, ( 
 ( #5771, #38136, #39983, #4829, #10774, #29375, #27386, #7807, #11190 ),
 ( #36987, #214, #3621, #33585, #19771, #9986, #23968, #30780, #14376 ),
 ( #40396, #32791, #16586, #13189, #1419, #6802, #1629, #22959, #16370 ),
 ( #20769, #1214, #4621, #33793, #29595, #20555, #27177, #26174, #14584 ),
 ( #39179, #3402, #17576, #30580, #24176, #37185, #40598, #4417, #8007 ),
 ( #10986, #17375, #23755, #35988, #36777, #20978, #8208, #7593, #33999 ),
 ( #1004, #17781, #27589, #30365, #14173, #40191, #13968, #11398, #24385 ),
 ( #26972, #37390, #32570, #11822, #2681, #37598, #41228, #31841, #27798 ),
 ( #15638, #5242, #24811, #34622, #38243, #28643, #17993, #2041, #12462 ),
 ( #41654, #28005, #35054, #41014, #30991, #15433, #38024, #41442, #22025 ),
 ( #1831, #34409, #21593, #8424, #40806, #12031, #18837, #2472, #25456 ),
 ( #11607, #5449, #18409, #5874, #21383, #34208, #37806, #38453, #8631 ),
 ( #31416, #2258, #15220, #34835, #28222, #31198, #24591, #25022, #21809 ),
 ( #8845, #14795, #21180, #5669, #5036, #18626, #18197, #15006, #9060 ),
 ( #31631, #28436, #12247, #25240, #19466, #330, #39291, #22434, #32903 ),
 ( #42079, #39082, #6081, #19673, #29697, #6287, #32474, #13082, #10097 ),
 ( #6704, #2886, #3304, #23070, #6918, #36103, #35464, #16269, #38868 ),
 ( #26074, #538, #13296, #118, #19887, #15849, #19044, #22228, #9884 ),
 ( #26283, #38663, #35257, #28855, #13512, #3734, #22856, #12872, #35894 ),
 ( #29059, #19258, #3522, #29489, #26501, #25861, #32688, #16483, #9680 ),
 ( #32266, #16692, #32049, #3096, #9271, #41868, #16057, #22646, #12667 ),
 ( #25656, #29271, #9471, #35680, #6489, #7965, #23491, #30116, #10725 ),
 ( #33956, #36316, #20295, #30738, #29907, #20932, #4152, #11148, #17115 ),
 ( #33748, #14127, #17531, #40353, #1163, #7135, #10520, #39933, #26714 ),
 ( #30318, #37143, #20724, #1586, #4573, #39722, #36518, #20092, #16905 ),
 ( #4787, #33536, #10311, #23923, #17737, #24134, #13720, #14544, #36725 ),
 ( #956, #33323, #39505, #745, #23280, #36939, #7337, #13925, #3945 ),
 ( #33116, #26918, #27128, #23705, #7547, #1372, #20508, #4368, #17328 ),
 ( #40142, #10934, #7760, #30532, #14329, #27341, #15172, #24981, #37980 ),
 ( #14961, #21763, #41398, #5408, #40971, #5201, #34165, #31159, #18580 ),
 ( #1998, #31588, #5831, #40764, #5623, #21979, #24766, #27963, #8588 ),
 ( #34368, #11775, #37553, #37764, #28178, #18156, #9015, #1791, #18364 ),
 ( #4991, #31370, #38198, #11562, #21552, #34581, #2426, #35012, #24343 ),
 ( #18786, #17949, #31799, #2214, #12203, #41183, #37348, #34789, #11986 ) ),
 .UNSPECIFIED., .F., .F., .F.,
 ( 4, 1, 1, 1, 1, 1, 1, 1, 1, 1, 1, 2, 1, 1, 1, 1, 1, 1, 1, 1, 1, 1, 1, 1, 1, 1, 1, 1, 1, 1, 4 ),
 ( 4, 1, 1, 1, 1, 1, 4 ),
 ( 0.000000000000000000, 0.01653533301974152714, 0.03307066603948305428, 0.04960599905922458142, 0.06614133207896610855, 0.09921199811844916283, 0.1322826641579322171, 0.1653533301974152714, 0.1984239962368983257, 0.2314946622763813799, 0.2500000000000000000, 0.2645653283158644342, 0.3105299952961229071, 0.3335123287862520325, 0.3564946622763812689, 0.4024593292566397418, 0.4943886632171566875, 0.5863179971776735222, 0.6666666666666666297, 0.6782473311381906900, 0.7701766650987074136, 0.8161413320789658865, 0.8850883325493537068, 0.8965794992944182695, 0.9080706660394826102, 0.9195618327845473949, 0.9310529995296121797, 0.9425441662746769644, 0.9540353330197415271, 0.9770176665098706525, 1.000000000000000000 ),
 ( 0.000000000000000000, 0.2500000000000000000, 0.4444444444444445308, 0.5000000000000000000, 0.7500000000000000000, 0.8333333333333333703, 1.000000000000000000 ),
 .UNSPECIFIED. ) ;
#23528 = CARTESIAN_POINT ( 'NONE',  ( 17.85978967527192296, 148.7876888829155746, 2.377023446492704473 ) ) ;
#23529 = CARTESIAN_POINT ( 'NONE',  ( -1.820350978615107751, 35.44831059284695129, 0.3018992756893351115 ) ) ;
#23530 = ADVANCED_FACE ( 'NONE', ( #32703 ), #7117, .T. ) ;
#23531 = CARTESIAN_POINT ( 'NONE',  ( 22.83540780336915432, 150.4058779721138421, 0.4563057931615321361 ) ) ;
#23532 = AXIS2_PLACEMENT_3D ( 'NONE', #11716, #24703, #20873 ) ;
#23533 = CARTESIAN_POINT ( 'NONE',  ( 1.932697321913770416, 19.28018055242734619, -8.218723488459904303 ) ) ;
#23534 = CARTESIAN_POINT ( 'NONE',  ( 15.91553746749626796, 146.9815093338748966, 1.044385907527698665 ) ) ;
#23535 = CIRCLE ( 'NONE', #31707, 0.6350000000000014522 ) ;
#23536 = CARTESIAN_POINT ( 'NONE',  ( 17.79905452297344937, 125.1550653296939970, -0.5857557929999462898 ) ) ;
#23537 = AXIS2_PLACEMENT_3D ( 'NONE', #11084, #37908, #24071 ) ;
#23538 = ADVANCED_FACE ( 'NONE', ( #9485 ), #19273, .T. ) ;
#23539 = DIRECTION ( 'NONE',  ( -0.8745520943968241312, 0.4849315768086548406, -5.691349986800536046E-16 ) ) ;
#23540 = B_SPLINE_CURVE_WITH_KNOTS ( 'NONE', 3,
 ( #9779, #41964, #18725, #31735, #8951, #22329, #35777, #21917, #19151, #22746, #38347, #32362, #35151, #6592, #32155, #41338, #12763, #2364, #5976, #6182, #2988, #18940, #38760, #31947, #3, #34947, #28330, #15950, #28947, #9571, #22541, #35568, #41759, #3190, #16152 ),
 .UNSPECIFIED., .F., .F.,
 ( 4, 1, 1, 1, 1, 1, 1, 1, 1, 1, 1, 1, 1, 1, 1, 1, 1, 1, 1, 1, 1, 1, 1, 1, 1, 1, 1, 1, 1, 1, 1, 1, 4 ),
 ( 0.000000000000000000, 0.02711375962671787321, 0.05385523109991235263, 0.08027126036152537614, 0.1064096946071439176, 0.1323192412471900226, 0.1580495177521483718, 0.1882118685537063907, 0.2182788543618764954, 0.2483346178351386324, 0.2784631806910429774, 0.3054937156393619513, 0.3327069032348308197, 0.3601597580799023035, 0.3879077415152338837, 0.4160045136367338525, 0.4445017332217630623, 0.4734489055539064517, 0.5028932750457014711, 0.5328797594123376724, 0.5634509204570880003, 0.5946469669818265080, 0.6265057848166851739, 0.6590629893014032792, 0.6923519956652609553, 0.7264041031822485728, 0.7612485893105871426, 0.7986318966073006065, 0.8369441774603861850, 0.8762126957585177900, 0.9164627945539034481, 0.9577180065289634392, 1.000000000000000000 ),
 .UNSPECIFIED. ) ;
#23541 = ORIENTED_EDGE ( 'NONE', *, *, #16231, .F. ) ;
#23542 = DIRECTION ( 'NONE',  ( 4.017660918040594346E-17, -1.000000000000000000, -2.376309959284834438E-19 ) ) ;
#23543 = EDGE_CURVE ( 'NONE', #9633, #12494, #26130, .T. ) ;
#23544 = UNCERTAINTY_MEASURE_WITH_UNIT (LENGTH_MEASURE( 1.000000000000000082E-05 ), #41838, 'distance_accuracy_value', 'NONE');
#23545 = CARTESIAN_POINT ( 'NONE',  ( -16.10770497005625757, 121.2391669109744186, -0.2160841345999987839 ) ) ;
#23546 = ORIENTED_EDGE ( 'NONE', *, *, #10721, .T. ) ;
#23547 = CARTESIAN_POINT ( 'NONE',  ( -8.005205585284276282, 121.4511398066844521, -1.197578517849991586 ) ) ;
#23548 = CARTESIAN_POINT ( 'NONE',  ( -8.635102817406197673, 118.5712416014078059, 0.7746300195078978934 ) ) ;
#23549 = ORIENTED_EDGE ( 'NONE', *, *, #2134, .T. ) ;
#23550 = FACE_OUTER_BOUND ( 'NONE', #7207, .T. ) ;
#23551 = CARTESIAN_POINT ( 'NONE',  ( -4.529648377621004585, 121.1059516323014549, -0.2990124396216894409 ) ) ;
#23552 = CARTESIAN_POINT ( 'NONE',  ( 4.658995561375286698, -13.35466759734559083, 3.413121997863386881 ) ) ;
#23553 = CARTESIAN_POINT ( 'NONE',  ( -5.352805660278798783, 158.9031408473208273, 0.9771030980504661345 ) ) ;
#23554 = DIRECTION ( 'NONE',  ( 0.1906721105964958585, -0.9816537812491110682, -9.356030339620071016E-15 ) ) ;
#23555 = CARTESIAN_POINT ( 'NONE',  ( 3.295257134497863838, 159.4684106755469202, 0.1128235000732134147 ) ) ;
#23556 = VERTEX_POINT ( 'NONE', #3317 ) ;
#23557 = CARTESIAN_POINT ( 'NONE',  ( -0.5842699607273857954, -4.454521554441356557, 4.585487691134133570 ) ) ;
#23558 = CARTESIAN_POINT ( 'NONE',  ( -13.69515342115119694, 119.6466660129326272, -0.2899717296217780294 ) ) ;
#23559 = DIRECTION ( 'NONE',  ( -0.9336303900108928744, -0.3582377630123714241, 0.000000000000000000 ) ) ;
#23560 = DIRECTION ( 'NONE',  ( 0.5149185422762211362, -0.8572391118119444542, 0.000000000000000000 ) ) ;
#23561 = CARTESIAN_POINT ( 'NONE',  ( -6.585129507136150195, 119.8605863436230692, 0.9846512238138591666 ) ) ;
#23562 = CARTESIAN_POINT ( 'NONE',  ( -4.540528814728789442, -1.371322978654152092, -0.8806307088788817294 ) ) ;
#23563 = CARTESIAN_POINT ( 'NONE',  ( 18.89746971955487709, 128.6554162386474047, 1.621015360058189581 ) ) ;
#23564 = CARTESIAN_POINT ( 'NONE',  ( -58.82993853617958280, -0.2576789964487402607, -0.02280678271007593322 ) ) ;
#23566 = CARTESIAN_POINT ( 'NONE',  ( 7.829350110466591239, 119.0983413489662297, -1.000240898550800672 ) ) ;
#23565 = DIRECTION ( 'NONE',  ( -0.8745520943968225769, 0.4849315768086578382, -5.691349986800571545E-16 ) ) ;
#23567 = CARTESIAN_POINT ( 'NONE',  ( -3.254339884055971854, 0.1279812147911008058, 3.287934741457726684 ) ) ;
#23568 = CARTESIAN_POINT ( 'NONE',  ( -17.76144578550761111, 125.1550653296939970, -1.296339218450673014 ) ) ;
#23569 = ORIENTED_EDGE ( 'NONE', *, *, #23472, .T. ) ;
#23570 = VERTEX_POINT ( 'NONE', #39096 ) ;
#23571 = AXIS2_PLACEMENT_3D ( 'NONE', #22109, #17721, #27327 ) ;
#23572 = CARTESIAN_POINT ( 'NONE',  ( -11.35800195117484535, 128.2076764602477681, 0.1601657033123586593 ) ) ;
#23573 = CARTESIAN_POINT ( 'NONE',  ( 2.466063760571058250, -15.50753052345275940, 5.840068263025540496 ) ) ;
#23574 = DIRECTION ( 'NONE',  ( 0.8745520943968235761, -0.4849315768086558398, 0.000000000000000000 ) ) ;
#23575 = CARTESIAN_POINT ( 'NONE',  ( -4.304088219600741283, 111.0463454453284555, -3.212841137876927711 ) ) ;
#23576 = EDGE_LOOP ( 'NONE', ( #29447, #27060, #7134, #15338 ) ) ;
#23577 = CARTESIAN_POINT ( 'NONE',  ( 12.33952200554331569, 155.1253022143813496, 2.231822996700852269 ) ) ;
#23578 = CARTESIAN_POINT ( 'NONE',  ( 13.85159022459153988, 59.63164443796365077, -5.016499999999999737 ) ) ;
#23579 = CARTESIAN_POINT ( 'NONE',  ( -29.90236731146035609, 69.13284574330884880, -1.270000000000007123 ) ) ;
#23580 = TOROIDAL_SURFACE ( 'NONE', #16098, 0.3810000000000002829, 0.2540000000000000036 ) ;
#23581 = CARTESIAN_POINT ( 'NONE',  ( -1.996658253870984723, 117.0827246868714013, 0.4092875891974779301 ) ) ;
#23582 = CARTESIAN_POINT ( 'NONE',  ( 5.527521262545286085, 2.498091250051501344, 6.371381250375013572 ) ) ;
#23583 = CARTESIAN_POINT ( 'NONE',  ( 0.5861964566936646026, 120.4790399057546182, 0.3305540093316995387 ) ) ;
#23584 = CYLINDRICAL_SURFACE ( 'NONE', #3605, 3.175000000000001155 ) ;
#23585 = CARTESIAN_POINT ( 'NONE',  ( 9.680782865131664749, 118.1749183431956425, -0.3159967629729716343 ) ) ;
#23586 = DIRECTION ( 'NONE',  ( 0.9849462604886048966, 0.000000000000000000, -0.1728608224830406881 ) ) ;
#23587 = AXIS2_PLACEMENT_3D ( 'NONE', #24849, #1665, #40842 ) ;
#23588 = CARTESIAN_POINT ( 'NONE',  ( -57.76462175338717486, 1.013803242785049630, 1.137036206963185414 ) ) ;
#23589 = CARTESIAN_POINT ( 'NONE',  ( -48.57236063951932437, 24.64054515024589165, -8.874850105164511634E-15 ) ) ;
#23591 = ADVANCED_FACE ( 'NONE', ( #9898 ), #7790, .T. ) ;
#23590 = DIRECTION ( 'NONE',  ( 5.188838149069472160E-16, -1.699382548006136559E-16, -1.000000000000000000 ) ) ;
#23592 = CARTESIAN_POINT ( 'NONE',  ( -52.30895062419047292, 13.66434875625866674, 4.401212925246481333 ) ) ;
#23593 = CARTESIAN_POINT ( 'NONE',  ( -57.77616480963058621, 1.544201637102598168, 1.578764309266320831 ) ) ;
#23594 = CARTESIAN_POINT ( 'NONE',  ( -4.532383222279214863, 118.1210121875601118, 0.4790102578777305498 ) ) ;
#23595 = CARTESIAN_POINT ( 'NONE',  ( 4.556421141688495879, 110.9173483060741887, -2.841207085095037943 ) ) ;
#23596 = CIRCLE ( 'NONE', #12060, 0.7620000000000015650 ) ;
#23597 = ORIENTED_EDGE ( 'NONE', *, *, #29018, .F. ) ;
#23598 = CARTESIAN_POINT ( 'NONE',  ( -43.82859865241511699, 24.63416949198730421, 1.523999999999993138 ) ) ;
#23599 = CARTESIAN_POINT ( 'NONE',  ( -8.299000378089440133, 119.9939463870335743, -1.448799010205415128 ) ) ;
#23600 = CARTESIAN_POINT ( 'NONE',  ( -6.114402651314438053, 119.5149100643186983, -0.5171552335003599676 ) ) ;
#23601 = CARTESIAN_POINT ( 'NONE',  ( 4.512626992550961447, 118.1142824865469834, 0.7004059809699817452 ) ) ;
#23602 = CARTESIAN_POINT ( 'NONE',  ( -7.725927843277678342, 122.1869765257964673, -0.7315739442948009374 ) ) ;
#23603 = CARTESIAN_POINT ( 'NONE',  ( -1.123231675714139177, 115.7029491485453292, -1.744269607945097667 ) ) ;
#23604 = CARTESIAN_POINT ( 'NONE',  ( 3.145428050085047555, 118.1651001541507355, -0.6645078962191128813 ) ) ;
#23605 = CARTESIAN_POINT ( 'NONE',  ( 4.074523107743381445, 109.7948460773305897, -3.525254900318187445 ) ) ;
#23606 = CARTESIAN_POINT ( 'NONE',  ( -10.62607977745490295, 123.8807653058400575, -1.354828998092944436 ) ) ;
#23607 = CARTESIAN_POINT ( 'NONE',  ( -4.333424916720135300, 104.6144662015457243, 3.954443799498177370 ) ) ;
#23608 = DIRECTION ( 'NONE',  ( 0.9998501190848629872, 0.01731298258490734585, 8.537024980200777445E-16 ) ) ;
#23609 = CARTESIAN_POINT ( 'NONE',  ( 8.323020013683247953, 120.1269634747937545, -1.118279847563949270 ) ) ;
#23610 = CARTESIAN_POINT ( 'NONE',  ( -8.415924194183428853, 123.3149294549902493, -0.04043142641129342241 ) ) ;
#23611 = CARTESIAN_POINT ( 'NONE',  ( 4.998195222330234166, 117.4629589511271348, -0.7743079785927495795 ) ) ;
#23612 = CARTESIAN_POINT ( 'NONE',  ( -0.005431400947739826145, 116.8580640273661118, 0.2718095133625909043 ) ) ;
#23613 = CARTESIAN_POINT ( 'NONE',  ( 18.35410564743290607, 77.35382415001784295, -5.016499999999999737 ) ) ;
#23614 = CARTESIAN_POINT ( 'NONE',  ( 1.977593594988821479, -15.25598227308876176, 5.283756247048868815 ) ) ;
#23615 = CARTESIAN_POINT ( 'NONE',  ( -18.60513690094820305, 148.0519089404264150, 1.698284372519642371 ) ) ;
#23616 = CARTESIAN_POINT ( 'NONE',  ( 0.8497018901738310204, -5.914940278964642140, -0.4796499176142879906 ) ) ;
#23617 = CARTESIAN_POINT ( 'NONE',  ( -15.50334291652352370, 121.0440340969820596, -0.8284681841690884063 ) ) ;
#23618 = AXIS2_PLACEMENT_3D ( 'NONE', #25538, #25332, #25121 ) ;
#23619 = CARTESIAN_POINT ( 'NONE',  ( -0.09873697212813982438, -3.591044343564580910, 0.9733856795103970061 ) ) ;
#23620 = ORIENTED_EDGE ( 'NONE', *, *, #39798, .T. ) ;
#23621 = CARTESIAN_POINT ( 'NONE',  ( -53.80167111242602118, 9.145755618221249605, 3.362987294923124537 ) ) ;
#23622 = CARTESIAN_POINT ( 'NONE',  ( 4.310423192638969780, 113.1344509532474376, 2.465321907391796241 ) ) ;
#23623 = ITEM_DEFINED_TRANSFORMATION ( 'NONE', 'NONE', #3297,  #3275 ) ;
#23624 = CARTESIAN_POINT ( 'NONE',  ( -1.542034982439734581, 120.6610732671444595, 0.2472410911860531690 ) ) ;
#23625 = CARTESIAN_POINT ( 'NONE',  ( 4.627184959846470491, -11.70336558297383611, 0.7419505617825855603 ) ) ;
#23626 = CARTESIAN_POINT ( 'NONE',  ( 3.718565865971962925, 156.7231754051992425, -1.451222330515914871 ) ) ;
#23627 = ORIENTED_EDGE ( 'NONE', *, *, #7122, .F. ) ;
#23628 = CARTESIAN_POINT ( 'NONE',  ( -19.50074546578255053, 147.2819018089465715, -2.521100153936117305 ) ) ;
#23629 = CARTESIAN_POINT ( 'NONE',  ( -4.722986921643055780, 104.6144662015457527, 1.042082362937506002 ) ) ;
#23630 = CARTESIAN_POINT ( 'NONE',  ( 3.212496809824684441, -14.25148094350509353, 2.370051959060230473 ) ) ;
#23631 = CARTESIAN_POINT ( 'NONE',  ( -4.863397889133672436, 117.6413937367854174, -1.052647808288214026 ) ) ;
#23632 = CARTESIAN_POINT ( 'NONE',  ( 11.86471938700702466, 151.9842433124228762, 0.02191723269355114190 ) ) ;
#23633 = VECTOR ( 'NONE', #21135, 1000.000000000000114 ) ;
#23634 = ORIENTED_EDGE ( 'NONE', *, *, #31919, .T. ) ;
#23635 = CARTESIAN_POINT ( 'NONE',  ( -2.933932892823386318, 107.6238140763627484, 4.446886960255170607 ) ) ;
#23636 = CARTESIAN_POINT ( 'NONE',  ( 2.445884319531578033, 107.2200259173994112, 4.733447966000433382 ) ) ;
#23637 = CARTESIAN_POINT ( 'NONE',  ( 1.650612623617701651E-15, 17.14499999999999957, 0.000000000000000000 ) ) ;
#23638 = CARTESIAN_POINT ( 'NONE',  ( 4.758755041966881372, 116.8068435238802465, -0.07043225793504322152 ) ) ;
#23639 = LINE ( 'NONE', #36662, #30191 ) ;
#23640 = TOROIDAL_SURFACE ( 'NONE', #34560, 0.3810000000000002829, 0.2540000000000000036 ) ;
#23641 = CARTESIAN_POINT ( 'NONE',  ( 1.878570595667757193, -15.26290889022100039, 5.982895072476400955 ) ) ;
#23642 = CARTESIAN_POINT ( 'NONE',  ( 11.58677707360117282, 55.41127257906217807, 4.474811398756911807 ) ) ;
#23643 = CARTESIAN_POINT ( 'NONE',  ( -2.667392527469405916, 31.33771804890096746, 0.9893360403373154810 ) ) ;
#23644 = CARTESIAN_POINT ( 'NONE',  ( 5.842949248259128758, 118.5625182843610617, 1.130067629703343624 ) ) ;
#23645 = ORIENTED_EDGE ( 'NONE', *, *, #25006, .F. ) ;
#23646 = CARTESIAN_POINT ( 'NONE',  ( -2.728255833603390190, 14.33847684266025801, 7.992727065595903291 ) ) ;
#23647 = CARTESIAN_POINT ( 'NONE',  ( 5.529981148835290128, 117.6928892124895896, -0.7912142295696815708 ) ) ;
#23648 = CARTESIAN_POINT ( 'NONE',  ( -4.134812325682042378, 122.5143120247930142, -0.2378952825278685956 ) ) ;
#23649 = CARTESIAN_POINT ( 'NONE',  ( -6.472048963935522405E-14, 69.43546620154573645, -1.207165458941418601E-19 ) ) ;
#23650 = LINE ( 'NONE', #480, #24979 ) ;
#23651 = CARTESIAN_POINT ( 'NONE',  ( -5.284088079744258870, 105.1223998609899724, 0.8090923337965348905 ) ) ;
#23652 = ADVANCED_FACE ( 'NONE', ( #23084 ), #35664, .T. ) ;
#23653 = CARTESIAN_POINT ( 'NONE',  ( 4.440015753948663324, -2.305524871907271400, 1.325333094644747245 ) ) ;
#23654 = DIRECTION ( 'NONE',  ( -0.9454731675810359448, 0.3256999990547780333, -5.459396135145339171E-16 ) ) ;
#23655 = CARTESIAN_POINT ( 'NONE',  ( -5.249547377000530979, 56.51499999999963109, -4.563748390634326135 ) ) ;
#23656 = B_SPLINE_CURVE_WITH_KNOTS ( 'NONE', 3,
 ( #26345, #19951, #29555, #1017 ),
 .UNSPECIFIED., .F., .F.,
 ( 4, 4 ),
 ( 0.000000000000000000, 0.5643836377221603806 ),
 .UNSPECIFIED. ) ;
#23657 = CARTESIAN_POINT ( 'NONE',  ( 3.398501971686946010, -13.69110397484313246, 2.823423868610629217 ) ) ;
#23658 = CARTESIAN_POINT ( 'NONE',  ( 0.2179432916432262890, 106.0530876078258586, -5.262233728842789837 ) ) ;
#23659 = CARTESIAN_POINT ( 'NONE',  ( -4.841477346016104910, 117.1414559920645644, 0.3963857013944136476 ) ) ;
#23660 = CARTESIAN_POINT ( 'NONE',  ( 4.801256233860562439, 117.4019745851689152, -1.015743786222129907 ) ) ;
#23661 = LINE ( 'NONE', #27293, #526 ) ;
#23662 = ORIENTED_EDGE ( 'NONE', *, *, #11563, .F. ) ;
#23663 = FACE_OUTER_BOUND ( 'NONE', #27797, .T. ) ;
#23664 = CARTESIAN_POINT ( 'NONE',  ( 2.674787014790545481, -15.76824019788006304, 5.299902074303234123 ) ) ;
#23665 = CARTESIAN_POINT ( 'NONE',  ( -2.650128318467547928, 158.3255140430775043, 1.577873239259485860 ) ) ;
#23666 = CARTESIAN_POINT ( 'NONE',  ( 2.862861873098513588, -10.07698056833738320, -3.640125809621840069 ) ) ;
#23667 = ORIENTED_EDGE ( 'NONE', *, *, #32062, .F. ) ;
#23668 = DIRECTION ( 'NONE',  ( -5.188838149069472160E-16, 1.699382548006136559E-16, 1.000000000000000000 ) ) ;
#23669 = CARTESIAN_POINT ( 'NONE',  ( 1.058122102717250934, 124.9344662015457459, 0.02114379780294273203 ) ) ;
#23670 = CARTESIAN_POINT ( 'NONE',  ( -10.06555281207545782, 123.2077283916686525, 0.8929836319946563572 ) ) ;
#23671 = CARTESIAN_POINT ( 'NONE',  ( -6.263959367015712765, 28.84083519579221999, 0.1566845698765544637 ) ) ;
#23672 =( BOUNDED_CURVE ( )  B_SPLINE_CURVE ( 3, ( #28985, #42002, #25790, #38795, #26853, #30460, #20231 ),
 .UNSPECIFIED., .F., .T. ) 
 B_SPLINE_CURVE_WITH_KNOTS ( ( 4, 3, 4 ),
 ( 0.4997054356531658859, 0.5000000000001099121, 0.5508374472049354376 ),
 .UNSPECIFIED. ) 
 CURVE ( )  GEOMETRIC_REPRESENTATION_ITEM ( )  RATIONAL_B_SPLINE_CURVE ( ( 0.9988224367574590756, 0.9992147264565607312, 0.9996072475374077060, 1.000000000000000000, 0.9322167370602015835, 0.8713253302225519858, 0.8173257794870510962 ) ) 
 REPRESENTATION_ITEM ( '' )  );
#23673 = CARTESIAN_POINT ( 'NONE',  ( 10.44084688387110837, 122.0805278159965610, -1.176281030686837203 ) ) ;
#23674 = CARTESIAN_POINT ( 'NONE',  ( -13.15656197906106684, 122.1656469061080514, -1.777190774585285071 ) ) ;
#23675 = CARTESIAN_POINT ( 'NONE',  ( -13.79703500197643073, 79.79115557309579287, 1.269999999999998685 ) ) ;
#23676 = VERTEX_POINT ( 'NONE', #26297 ) ;
#23677 = CARTESIAN_POINT ( 'NONE',  ( 4.267851022923248472, 118.2240358439523362, -0.2903317238581183957 ) ) ;
#23678 = CARTESIAN_POINT ( 'NONE',  ( 1.653377498379587696, 156.2910218135955631, -0.4236837486942555131 ) ) ;
#23679 = ORIENTED_EDGE ( 'NONE', *, *, #30320, .F. ) ;
#23680 = CARTESIAN_POINT ( 'NONE',  ( 3.172822981795960562, -14.65879537465078464, 0.2101774045261552148 ) ) ;
#23681 = CARTESIAN_POINT ( 'NONE',  ( -4.866602953137410204, 117.4089747018453238, 0.9905608030323003188 ) ) ;
#23682 = CARTESIAN_POINT ( 'NONE',  ( -48.97544177848091351, 17.83334834807254055, 5.075951225175634463 ) ) ;
#23683 = CARTESIAN_POINT ( 'NONE',  ( 4.531904421025400254, 4.026177021345840323, -0.9239884639389631671 ) ) ;
#23684 = CARTESIAN_POINT ( 'NONE',  ( 1.432854634133363891, 120.0849730816093910, 0.5085234606245938593 ) ) ;
#23685 = CARTESIAN_POINT ( 'NONE',  ( -1.474725677411676372, 32.11469766029267703, 1.198063404855159275 ) ) ;
#23686 = AXIS2_PLACEMENT_3D ( 'NONE', #29000, #12813, #35404 ) ;
#23687 = EDGE_CURVE ( 'NONE', #16908, #18068, #13220, .T. ) ;
#23688 = CARTESIAN_POINT ( 'NONE',  ( -4.492784857928645792, 12.16275517495587977, -1.104450737933446725 ) ) ;
#23689 = CARTESIAN_POINT ( 'NONE',  ( 15.72575858332438870, 145.6903699455376113, 0.3657738730356401846 ) ) ;
#23690 = PLANE ( 'NONE',  #37179 ) ;
#23691 = ADVANCED_FACE ( 'NONE', ( #38467 ), #22450, .T. ) ;
#23692 = CARTESIAN_POINT ( 'NONE',  ( -51.60883138897295908, 11.95321700621929040, -1.992363451474707947 ) ) ;
#23693 = CARTESIAN_POINT ( 'NONE',  ( -8.792762063912906711, 117.6983032061184957, -0.2971417965732215394 ) ) ;
#23694 = CARTESIAN_POINT ( 'NONE',  ( -11.73534362491071903, 82.73994711668952107, -1.524000000000000021 ) ) ;
#23695 = CARTESIAN_POINT ( 'NONE',  ( -4.466782427718574588, 71.06098887363195615, 1.270000000000005791 ) ) ;
#23696 = DIRECTION ( 'NONE',  ( -0.8745520943968241312, 0.4849315768086548406, -5.691349986800536046E-16 ) ) ;
#23697 = CARTESIAN_POINT ( 'NONE',  ( -28.89366501045254765, 63.08038031660233003, -1.524000000000005128 ) ) ;
#23698 = CARTESIAN_POINT ( 'NONE',  ( 3.113543590025587005, -0.1312883392403825233, -7.836836066719057747 ) ) ;
#23699 = CARTESIAN_POINT ( 'NONE',  ( -46.43586784920008625, 25.95560800814362423, 1.524002373413926303 ) ) ;
#23700 = FACE_OUTER_BOUND ( 'NONE', #3055, .T. ) ;
#23701 = CARTESIAN_POINT ( 'NONE',  ( -58.29256068059346063, 1.279866164410503604, 0.9167068831667634088 ) ) ;
#23702 = CARTESIAN_POINT ( 'NONE',  ( -4.999405966312342464, 117.3993846663101266, -0.8267122116642939833 ) ) ;
#23703 = CARTESIAN_POINT ( 'NONE',  ( -15.95511372484729051, 121.3860667298135070, 0.1093881341078833946 ) ) ;
#23704 = ORIENTED_EDGE ( 'NONE', *, *, #29579, .F. ) ;
#23705 = CARTESIAN_POINT ( 'NONE',  ( -58.00234944525002589, 2.059104932340308114, -0.8980956459801348046 ) ) ;
#23706 = CARTESIAN_POINT ( 'NONE',  ( 6.053201463129273208, 121.4432835561000985, 0.09870068995202660456 ) ) ;
#23707 = CIRCLE ( 'NONE', #29152, 0.6350000000000006750 ) ;
#23708 = EDGE_LOOP ( 'NONE', ( #36727, #19350, #30240, #29303 ) ) ;
#23709 = CARTESIAN_POINT ( 'NONE',  ( 3.657801486795293044, 115.7029491485453008, -1.477931297577026459 ) ) ;
#23710 = CARTESIAN_POINT ( 'NONE',  ( -11.06205061746909024, 128.0319838675845290, -0.2615737156286699339 ) ) ;
#23711 = CARTESIAN_POINT ( 'NONE',  ( 4.841517317049865987, -14.78816330421856051, 4.356870016251622957 ) ) ;
#23712 = CIRCLE ( 'NONE', #34616, 2.540000000000000480 ) ;
#23713 = CARTESIAN_POINT ( 'NONE',  ( -20.94193450296710068, 149.6610172957225586, 1.461262285038966047 ) ) ;
#23714 = CARTESIAN_POINT ( 'NONE',  ( -0.8080508600641239658, 24.25718022715097533, 4.550674767031389401 ) ) ;
#23715 = CARTESIAN_POINT ( 'NONE',  ( 15.09710430809799853, 156.1437908837410191, 0.6951944926208392106 ) ) ;
#23716 = CARTESIAN_POINT ( 'NONE',  ( 15.75500244940657524, 145.8995334253134217, 0.5165061539673916347 ) ) ;
#23717 = CARTESIAN_POINT ( 'NONE',  ( 0.6857505489063979720, -9.425274534614802135, -0.6942005185601292094 ) ) ;
#23718 = B_SPLINE_CURVE_WITH_KNOTS ( 'NONE', 3,
 ( #6496, #5883, #39089, #15857, #13089, #15646, #25869, #6089 ),
 .UNSPECIFIED., .F., .F.,
 ( 4, 2, 2, 4 ),
 ( 0.000000000000000000, 0.0002285670694212123722, 0.0004571341388424247443, 0.0009142682776848494886 ),
 .UNSPECIFIED. ) ;
#23719 = CARTESIAN_POINT ( 'NONE',  ( -18.60568445592648601, 154.1511370093759865, -0.5871577710369983993 ) ) ;
#23720 = CARTESIAN_POINT ( 'NONE',  ( -11.58677707360137532, 55.98894877578615592, 4.474811398758257397 ) ) ;
#23721 = DIRECTION ( 'NONE',  ( -0.8745520943968240202, 0.4849315768086552292, -5.361993529360572958E-16 ) ) ;
#23722 = ORIENTED_EDGE ( 'NONE', *, *, #36658, .F. ) ;
#23723 = CARTESIAN_POINT ( 'NONE',  ( 5.529640237942972547, 117.0347480979416019, 0.6524371917319816694 ) ) ;
#23724 = CARTESIAN_POINT ( 'NONE',  ( -18.00357552251037063, 146.8415343102147972, 1.578964580512863369 ) ) ;
#23725 = CARTESIAN_POINT ( 'NONE',  ( -58.24246139542360368, -0.02011471684311166505, -0.4719173402914386695 ) ) ;
#23726 = CARTESIAN_POINT ( 'NONE',  ( 14.14688762606133388, 122.0820592118662091, 1.654226634644705873 ) ) ;
#23727 = CARTESIAN_POINT ( 'NONE',  ( 1.263959281924152966, 118.7146927282448132, -0.6429003683496401500 ) ) ;
#23728 = CARTESIAN_POINT ( 'NONE',  ( -0.5179912613141952615, -13.03896268189918217, -0.8249499322734266116 ) ) ;
#23729 = CARTESIAN_POINT ( 'NONE',  ( 0.009513433763454561681, 117.6614778598761291, -0.4760911276077178234 ) ) ;
#23730 = CARTESIAN_POINT ( 'NONE',  ( -47.07934102874902749, 22.98505637820369429, -3.579966862081945145 ) ) ;
#23731 = CARTESIAN_POINT ( 'NONE',  ( 3.853311296320406587, 104.6144662015434932, 3.705097815587511167 ) ) ;
#23732 = ADVANCED_FACE ( 'NONE', ( #42093 ), #12888, .F. ) ;
#23733 = CARTESIAN_POINT ( 'NONE',  ( 16.49265603038150374, 146.0252812507985141, -0.9509463687623791461 ) ) ;
#23734 = CARTESIAN_POINT ( 'NONE',  ( -8.981069108608934926, 123.9698733229553937, -0.1794631345465899919 ) ) ;
#23735 = ORIENTED_EDGE ( 'NONE', *, *, #37593, .T. ) ;
#23736 = CARTESIAN_POINT ( 'NONE',  ( -9.734001924785522064, 155.3230018269108825, -2.058186707467866139 ) ) ;
#23737 = CARTESIAN_POINT ( 'NONE',  ( 4.357275237516622823, -15.68314232965556343, 3.240836981083619062 ) ) ;
#23738 = DIRECTION ( 'NONE',  ( 5.188838149069472160E-16, -1.699382548006136559E-16, -1.000000000000000000 ) ) ;
#23739 = CARTESIAN_POINT ( 'NONE',  ( -4.612168628140729254, 117.9566741055143524, -0.9390375305927243232 ) ) ;
#23740 = CARTESIAN_POINT ( 'NONE',  ( -55.11216289415786207, 6.786895728730008237, -3.177266426849177705 ) ) ;
#23741 = CARTESIAN_POINT ( 'NONE',  ( 4.107391299159643516, 118.2429491485453497, 0.3509127516616104003 ) ) ;
#23742 = CARTESIAN_POINT ( 'NONE',  ( 16.90821003499434383, 140.1729163700083518, 2.280195664865559912 ) ) ;
#23743 = CARTESIAN_POINT ( 'NONE',  ( -4.432242455686237648, 32.76553509196318004, 1.287969469385144006 ) ) ;
#23744 = AXIS2_PLACEMENT_3D ( 'NONE', #13670, #7289, #28857 ) ;
#23745 = AXIS2_PLACEMENT_3D ( 'NONE', #1321, #33059, #40303 ) ;
#23746 = CARTESIAN_POINT ( 'NONE',  ( 13.70496720262315193, 119.6480011847128253, 0.2738578607176475055 ) ) ;
#23747 = CARTESIAN_POINT ( 'NONE',  ( 0.7770267621822702919, 9.899933826931993863, -8.437367074289049640 ) ) ;
#23748 = CARTESIAN_POINT ( 'NONE',  ( 5.901573779631297256, 121.4708175001875077, 0.3521552259516175232 ) ) ;
#23749 = CARTESIAN_POINT ( 'NONE',  ( 8.102197167284966639, 117.9965348323767671, -0.5618759090088266683 ) ) ;
#23750 = CARTESIAN_POINT ( 'NONE',  ( 5.305748947172212127, 57.14999999999998437, 5.247078976224250013 ) ) ;
#23751 = CARTESIAN_POINT ( 'NONE',  ( 0.1669061836184802250, 115.6909491485452719, 1.766429643240662095 ) ) ;
#23752 = ADVANCED_FACE ( 'NONE', ( #9694 ), #9922, .T. ) ;
#23753 = CARTESIAN_POINT ( 'NONE',  ( -0.0008202526018428905668, 159.6052337359418800, 0.04104879434819971862 ) ) ;
#23754 = ORIENTED_EDGE ( 'NONE', *, *, #41075, .F. ) ;
#23755 = CARTESIAN_POINT ( 'NONE',  ( -47.17284909187768704, 24.49633334977720978, -1.858123130129392564 ) ) ;
#23756 = CARTESIAN_POINT ( 'NONE',  ( 5.532952480631610825, 120.7401383209704733, -0.5099206179826454299 ) ) ;
#23757 = CARTESIAN_POINT ( 'NONE',  ( -46.70722035912778125, 25.99002130463116700, -1.524000028481488522 ) ) ;
#23758 = DIRECTION ( 'NONE',  ( 1.011795553208986377E-16, 1.000000000000000000, -0.000000000000000000 ) ) ;
#23759 = CARTESIAN_POINT ( 'NONE',  ( -8.672603809708856915, 123.3259068333282755, -0.4768435845110673976 ) ) ;
#23760 = CARTESIAN_POINT ( 'NONE',  ( 3.520038346949750707, -14.46602075298747359, 5.128058278438484052 ) ) ;
#23761 = CARTESIAN_POINT ( 'NONE',  ( -17.11036550247955290, 125.2153959547233910, 0.9255656842583632749 ) ) ;
#23762 = FACE_OUTER_BOUND ( 'NONE', #19118, .T. ) ;
#23763 = CARTESIAN_POINT ( 'NONE',  ( 9.813487807256207063, 117.9943556427423488, 0.2419611575297473949 ) ) ;
#23764 = VERTEX_POINT ( 'NONE', #10326 ) ;
#23765 = CARTESIAN_POINT ( 'NONE',  ( 4.611808778022512989, -11.57686662695173929, 0.3579861242195471194 ) ) ;
#23766 = CARTESIAN_POINT ( 'NONE',  ( -23.11127252101368867, 149.9001116002701224, -0.4618182267416073850 ) ) ;
#23767 = DIRECTION ( 'NONE',  ( -1.000000000000000000, 9.627370216492862708E-17, 0.000000000000000000 ) ) ;
#23768 = CIRCLE ( 'NONE', #16990, 0.7620000000000015650 ) ;
#23769 = FACE_OUTER_BOUND ( 'NONE', #37797, .T. ) ;
#23770 = ORIENTED_EDGE ( 'NONE', *, *, #12017, .T. ) ;
#23771 = CARTESIAN_POINT ( 'NONE',  ( -5.640823739553852079, 119.8537775533140604, 0.8705914987587907161 ) ) ;
#23772 = EDGE_CURVE ( 'NONE', #18200, #21005, #7352, .T. ) ;
#23773 = CIRCLE ( 'NONE', #10158, 0.6349999999999998979 ) ;
#23774 = CARTESIAN_POINT ( 'NONE',  ( -4.324967070706027705, -0.5217348546298696821, 1.653223044864502222 ) ) ;
#23775 = CARTESIAN_POINT ( 'NONE',  ( 12.63141193514819705, 156.8164516032445306, 1.520932111850479496 ) ) ;
#23776 = CARTESIAN_POINT ( 'NONE',  ( -58.03077483564815964, 0.4858688437076191247, -1.087158688094550296 ) ) ;
#23778 = CARTESIAN_POINT ( 'NONE',  ( 12.83522892222227085, 121.3369795956499928, -1.134461614517290551 ) ) ;
#23777 = DIRECTION ( 'NONE',  ( -0.7548010569845216011, -0.6559537821943317581, -2.801824109679580762E-16 ) ) ;
#23779 = CARTESIAN_POINT ( 'NONE',  ( -1.319288878716189828, -8.717950886928733212, 4.428293336331323715 ) ) ;
#23780 = CARTESIAN_POINT ( 'NONE',  ( -22.54106487284180105, 146.4122051224262577, -1.767531409769413253 ) ) ;
#23781 = ORIENTED_EDGE ( 'NONE', *, *, #40789, .T. ) ;
#23782 = B_SPLINE_CURVE_WITH_KNOTS ( 'NONE', 3,
 ( #12396, #25584, #16408, #9200, #25386, #32612, #38389, #34988 ),
 .UNSPECIFIED., .F., .F.,
 ( 4, 2, 2, 4 ),
 ( 0.003986743484052250597, 0.004242962777773736337, 0.004499182071495222077, 0.005011620658938190087 ),
 .UNSPECIFIED. ) ;
#23783 = CARTESIAN_POINT ( 'NONE',  ( -8.132787923797444307, 122.8458379852381910, 0.04721391815988599389 ) ) ;
#23784 = ADVANCED_FACE ( 'NONE', ( #16921 ), #7088, .T. ) ;
#23785 = CARTESIAN_POINT ( 'NONE',  ( 6.471342906213767066, -13.19865009487615559, 0.2853922585125314715 ) ) ;
#23786 = CARTESIAN_POINT ( 'NONE',  ( -26.51793118801306548, 72.98537704160715123, -1.524000000000006017 ) ) ;
#23787 = EDGE_CURVE ( 'NONE', #27418, #33914, #17287, .T. ) ;
#23788 = CARTESIAN_POINT ( 'NONE',  ( -0.3349390595691898453, 117.3993832489317128, -1.495620772394688602 ) ) ;
#23789 = ORIENTED_EDGE ( 'NONE', *, *, #7400, .T. ) ;
#23790 = CARTESIAN_POINT ( 'NONE',  ( 11.78639615006484576, 122.5845257805695923, 1.760937685738447556 ) ) ;
#23791 = CARTESIAN_POINT ( 'NONE',  ( -26.37263903973852663, 72.23735686029533554, 1.523999999999993582 ) ) ;
#23792 = CARTESIAN_POINT ( 'NONE',  ( -30.15519950990045572, 69.97033940222175374, -1.270000000000007123 ) ) ;
#23793 = CARTESIAN_POINT ( 'NONE',  ( -4.883164212476821753, 117.4312795728108227, 0.5545796311387337640 ) ) ;
#23794 = CARTESIAN_POINT ( 'NONE',  ( -5.788041011255496748, 9.848169244510268427, 6.116426545680356597 ) ) ;
#23795 = CARTESIAN_POINT ( 'NONE',  ( 7.827001302695538953, 121.9903164032602518, 0.9115841697347605299 ) ) ;
#23796 = DIRECTION ( 'NONE',  ( 0.9336303900108815501, 0.3582377630124009560, 4.235673982319039874E-16 ) ) ;
#23797 = AXIS2_PLACEMENT_3D ( 'NONE', #30876, #19128, #194 ) ;
#23798 = ADVANCED_FACE ( 'NONE', ( #36333 ), #38403, .T. ) ;
#23799 = CARTESIAN_POINT ( 'NONE',  ( 19.82178279981176061, 128.7876384977266468, -0.3398896782655024817 ) ) ;
#23800 = DIRECTION ( 'NONE',  ( -0.8745520943968235761, 0.4849315768086558398, -4.268512490100410909E-16 ) ) ;
#23801 = CARTESIAN_POINT ( 'NONE',  ( -56.94799265811163025, 2.765196624222747701, 1.846149193847710368 ) ) ;
#23802 = CARTESIAN_POINT ( 'NONE',  ( -47.69778088985397346, 22.45332703829874887, 3.190613414150596405 ) ) ;
#23803 = CARTESIAN_POINT ( 'NONE',  ( -50.15972161391664486, 17.13814111569220699, 4.955022299345067438 ) ) ;
#23804 = CARTESIAN_POINT ( 'NONE',  ( -58.41428929413609694, 0.1660174354409331698, 0.8423104164767426516 ) ) ;
#23805 = CARTESIAN_POINT ( 'NONE',  ( -4.361853176623482042, 118.1815349744495762, 0.4500548209967693003 ) ) ;
#23806 = CARTESIAN_POINT ( 'NONE',  ( 1.205487064955253595, 106.0888231320280255, -5.200672005475023063 ) ) ;
#23807 = ORIENTED_EDGE ( 'NONE', *, *, #25636, .F. ) ;
#23808 = CARTESIAN_POINT ( 'NONE',  ( -45.68084146533627887, 21.25878370237693815, 4.188014402015102000 ) ) ;
#23809 = CARTESIAN_POINT ( 'NONE',  ( 6.118303280479630679, 119.4740638505368509, -1.016964802927776468 ) ) ;
#23810 = CARTESIAN_POINT ( 'NONE',  ( -7.301789825441274751, 123.0387167848234355, -0.2146691528375950508 ) ) ;
#23811 = CARTESIAN_POINT ( 'NONE',  ( 4.575203770056261554, 118.0775004785955957, 0.7114012580090923743 ) ) ;
#23812 = CARTESIAN_POINT ( 'NONE',  ( -15.16020740373479292, 148.9716719698033387, -1.401450122450045077 ) ) ;
#23813 = CARTESIAN_POINT ( 'NONE',  ( -0.3140675500742723947, 115.7030945160809665, -1.764426291103405653 ) ) ;
#23814 = AXIS2_PLACEMENT_3D ( 'NONE', #14712, #14921, #5164 ) ;
#23815 = DIRECTION ( 'NONE',  ( -5.463695987328526437E-16, -1.000000000000000000, -1.672774450599033775E-31 ) ) ;
#23816 = CARTESIAN_POINT ( 'NONE',  ( 7.140971181236829501, 122.4194348751405101, 0.03314210641492772169 ) ) ;
#23817 = ADVANCED_FACE ( 'NONE', ( #39737 ), #17938, .T. ) ;
#23818 = CARTESIAN_POINT ( 'NONE',  ( -12.69811389000567026, 152.1353413313561305, -1.627698677231679270 ) ) ;
#23819 = DIRECTION ( 'NONE',  ( -4.017660918040594346E-17, 1.000000000000000000, 2.376309959284834438E-19 ) ) ;
#23820 = CARTESIAN_POINT ( 'NONE',  ( -47.61073963479441318, 19.67761866749937028, 5.209507068477045699 ) ) ;
#23821 = EDGE_CURVE ( 'NONE', #41231, #37437, #13735, .T. ) ;
#23822 = CARTESIAN_POINT ( 'NONE',  ( 8.438003980598413278, 119.5616927475980305, -1.071839762751809033 ) ) ;
#23823 = CARTESIAN_POINT ( 'NONE',  ( -8.948733625370710598, 124.0488388276255591, -0.04532362284662430629 ) ) ;
#23824 = CARTESIAN_POINT ( 'NONE',  ( -3.682264917456324671, 97.37546620154573418, -0.07358041635423968885 ) ) ;
#23825 = CARTESIAN_POINT ( 'NONE',  ( -0.005915287708770879636, 116.9295063353193882, 0.2960251855814710065 ) ) ;
#23826 = CARTESIAN_POINT ( 'NONE',  ( 1.734723475976807094E-15, 17.14499999999999957, 0.000000000000000000 ) ) ;
#23827 = CARTESIAN_POINT ( 'NONE',  ( 3.320832222217961593, -15.07605257934231702, 3.106094183260712516 ) ) ;
#23828 = AXIS2_PLACEMENT_3D ( 'NONE', #4131, #6470, #36078 ) ;
#23829 = CARTESIAN_POINT ( 'NONE',  ( -1.009415275228709108, 157.6350123088122359, 1.589207162029932174 ) ) ;
#23830 = CARTESIAN_POINT ( 'NONE',  ( -0.1719059670432218079, -9.367746741450257986, 0.9581547781327369728 ) ) ;
#23831 = CARTESIAN_POINT ( 'NONE',  ( -10.62864291685186480, 157.9324367681937815, -0.7848347606367999107 ) ) ;
#23832 = CARTESIAN_POINT ( 'NONE',  ( -0.9568942166608355171, -5.529307923341535869, 0.1941686039811585662 ) ) ;
#23833 = ORIENTED_EDGE ( 'NONE', *, *, #1224, .F. ) ;
#23834 = CARTESIAN_POINT ( 'NONE',  ( -47.89521659674720411, 15.90546175020217312, 0.7967971578063748339 ) ) ;
#23835 = CARTESIAN_POINT ( 'NONE',  ( 7.669310211018360413, 124.7206709383052043, 0.1531702926821041921 ) ) ;
#23836 = SHAPE_DEFINITION_REPRESENTATION ( #40242, #26424 ) ;
#23837 = CARTESIAN_POINT ( 'NONE',  ( -6.495086324198092065, 121.6155390319085683, 0.2579311815284318077 ) ) ;
#23838 = CARTESIAN_POINT ( 'NONE',  ( 4.589616127059429118, -13.46842606041413681, 3.597705605327369494 ) ) ;
#23839 = CARTESIAN_POINT ( 'NONE',  ( 9.755129750886695206, 122.6450757329969434, -0.9482731561257333741 ) ) ;
#23840 = ORIENTED_EDGE ( 'NONE', *, *, #4860, .F. ) ;
#23841 = CARTESIAN_POINT ( 'NONE',  ( -8.582646176848058417, 120.3810071108087243, -1.481269161951472402 ) ) ;
#23842 = CARTESIAN_POINT ( 'NONE',  ( 3.907822414802752942, 115.7034623327353700, 1.591805045670572571 ) ) ;
#23843 = ADVANCED_FACE ( 'NONE', ( #14140 ), #7149, .T. ) ;
#23844 = AXIS2_PLACEMENT_3D ( 'NONE', #33571, #36762, #4188 ) ;
#23845 = CARTESIAN_POINT ( 'NONE',  ( 2.461817612451524084, -15.00653475910608492, 4.866425834902347702 ) ) ;
#23846 = CARTESIAN_POINT ( 'NONE',  ( -4.768865426206803093, 117.4736200371610124, -1.192916987142205398 ) ) ;
#23847 = CARTESIAN_POINT ( 'NONE',  ( 2.914310908016687129, 156.0868537499222839, -0.09385809996612891337 ) ) ;
#23848 = EDGE_CURVE ( 'NONE', #26111, #30817, #28168, .T. ) ;
#23849 = ORIENTED_EDGE ( 'NONE', *, *, #34679, .F. ) ;
#23850 = CARTESIAN_POINT ( 'NONE',  ( -3.945671927095251164, 109.6290767857811517, 3.598460797816132928 ) ) ;
#23851 = CARTESIAN_POINT ( 'NONE',  ( 2.754021448042122344, 107.6241103294158421, 4.560424122646145051 ) ) ;
#23852 = CARTESIAN_POINT ( 'NONE',  ( -14.91134437184023653, 120.3281135999119158, -0.2979641475767019765 ) ) ;
#23853 = CIRCLE ( 'NONE', #5507, 0.5080000000000000071 ) ;
#23854 = DIRECTION ( 'NONE',  ( 0.9816537812491075154, 0.1906721105965147323, 1.009874931538509940E-14 ) ) ;
#23855 = CARTESIAN_POINT ( 'NONE',  ( 23.35661798279346613, 142.7586093370927074, 0.2368412396931510178 ) ) ;
#23856 = FACE_OUTER_BOUND ( 'NONE', #14067, .T. ) ;
#23857 = CIRCLE ( 'NONE', #4156, 0.7619999999999976792 ) ;
#23858 = CARTESIAN_POINT ( 'NONE',  ( 1.650148621069484456, -15.47745783346181270, 5.677412139331382335 ) ) ;
#23859 = CARTESIAN_POINT ( 'NONE',  ( 11.58677707360137354, 55.24500000000000455, 4.474811398758258285 ) ) ;
#23860 = CARTESIAN_POINT ( 'NONE',  ( 2.711364258112227255, 37.31625399494021877, -1.095520810760639119 ) ) ;
#23861 = CARTESIAN_POINT ( 'NONE',  ( 18.06424110348773837, 131.7244750738095149, 2.230326231357608879 ) ) ;
#23862 = ORIENTED_EDGE ( 'NONE', *, *, #28742, .T. ) ;
#23863 = CARTESIAN_POINT ( 'NONE',  ( -8.304712878168881929, 22.30428017260781459, 1.495267265505846765 ) ) ;
#23864 = CARTESIAN_POINT ( 'NONE',  ( -5.525388478442741835, 117.9263796157108999, -1.079542212685845382 ) ) ;
#23865 = CARTESIAN_POINT ( 'NONE',  ( -2.282361306983861748, 118.7862729053988318, -0.7764855222020031755 ) ) ;
#23866 = CARTESIAN_POINT ( 'NONE',  ( -5.177913976931298734, 78.94499979771843812, 5.372100000000002318 ) ) ;
#23867 = CARTESIAN_POINT ( 'NONE',  ( -4.224169503853285157, 111.8944061756419899, -2.913215179389268439 ) ) ;
#23868 = DIRECTION ( 'NONE',  ( 5.188838149069472160E-16, -1.699382548006136559E-16, -1.000000000000000000 ) ) ;
#23869 = CARTESIAN_POINT ( 'NONE',  ( -0.8823465807374654135, 5.041073445128725794, 4.537322665494407659 ) ) ;
#23870 = DIRECTION ( 'NONE',  ( -0.4849315768086480682, -0.8745520943968280170, -1.030032898892941538E-16 ) ) ;
#23871 = CARTESIAN_POINT ( 'NONE',  ( -4.880629475887630520, 56.51998046905276141, -4.886937129208420494 ) ) ;
#23872 = CARTESIAN_POINT ( 'NONE',  ( 3.011490660845400402, -14.57542554230247056, 4.052385860498629810 ) ) ;
#23873 = CARTESIAN_POINT ( 'NONE',  ( 4.584908976607962927, 124.7699485019152945, 0.08702032153807698345 ) ) ;
#23874 = CARTESIAN_POINT ( 'NONE',  ( -22.84463062875821038, 149.4631731099488832, 0.5130293307460866981 ) ) ;
#23875 = CARTESIAN_POINT ( 'NONE',  ( 1.551849484730043249, 37.27687219050756084, 1.848690871642290734 ) ) ;
#23876 = DIRECTION ( 'NONE',  ( 6.353134868986659519E-16, -1.000000000000000000, -0.000000000000000000 ) ) ;
#23877 = EDGE_LOOP ( 'NONE', ( #16722, #7810 ) ) ;
#23878 = CARTESIAN_POINT ( 'NONE',  ( -36.98328822617348521, 27.82293856516310981, 1.269999999999995355 ) ) ;
#23879 = CARTESIAN_POINT ( 'NONE',  ( 4.790902082350968705, -15.53225359860559074, 1.708430371912022849 ) ) ;
#23880 = CARTESIAN_POINT ( 'NONE',  ( -0.4701463269445154691, 118.5593716040226724, 0.5956656855050136423 ) ) ;
#23881 = CIRCLE ( 'NONE', #29328, 0.2540000000000012248 ) ;
#23882 = CARTESIAN_POINT ( 'NONE',  ( 0.6634555152105963138, 29.00466287695533296, -0.7151348822165174424 ) ) ;
#23883 = B_SPLINE_CURVE_WITH_KNOTS ( 'NONE', 3,
 ( #10053, #7293, #3472, #23233, #279, #910, #16434, #23445 ),
 .UNSPECIFIED., .F., .F.,
 ( 4, 2, 2, 4 ),
 ( 0.000000000000000000, 0.2500000000000000000, 0.5000000000000000000, 1.000000000000000000 ),
 .UNSPECIFIED. ) ;
#23884 = VERTEX_POINT ( 'NONE', #35396 ) ;
#23885 = DIRECTION ( 'NONE',  ( -1.000000000000000000, 0.000000000000000000, 0.000000000000000000 ) ) ;
#23886 = CARTESIAN_POINT ( 'NONE',  ( 0.2286055872008740109, 108.3383513567250986, 4.353007566726655675 ) ) ;
#23887 = PRODUCT_DEFINITION_SHAPE ( 'NONE', 'NONE',  #42168 ) ;
#23888 = CARTESIAN_POINT ( 'NONE',  ( -8.809140270325823252, 122.1986804192922875, 0.8245386672919369220 ) ) ;
#23889 = CARTESIAN_POINT ( 'NONE',  ( -33.42971872652992005, 49.93539301574497102, 1.269999999999993578 ) ) ;
#23890 = CARTESIAN_POINT ( 'NONE',  ( 18.60513690094807160, 148.0519089404264150, -1.698284372519642149 ) ) ;
#23891 = AXIS2_PLACEMENT_3D ( 'NONE', #14002, #20589, #30401 ) ;
#23892 = CARTESIAN_POINT ( 'NONE',  ( -11.41340492329623402, 156.2473422840488979, -2.091747920666957139 ) ) ;
#23893 = DIRECTION ( 'NONE',  ( 0.6850534820564753158, -0.7284927773988556510, -1.146843430008118057E-15 ) ) ;
#23894 = CARTESIAN_POINT ( 'NONE',  ( 4.160584620051752225, 118.2392938275661862, -0.2307419219016439149 ) ) ;
#23895 = CARTESIAN_POINT ( 'NONE',  ( 0.003756957834416090915, 120.7746249494737896, -0.1880135328902412806 ) ) ;
#23896 = EDGE_LOOP ( 'NONE', ( #8587, #10523 ) ) ;
#23897 = CARTESIAN_POINT ( 'NONE',  ( 3.178195937486941958, -14.44740043277138675, 1.484392166672811930 ) ) ;
#23898 = AXIS2_PLACEMENT_3D ( 'NONE', #13457, #20246, #17683 ) ;
#23899 = CARTESIAN_POINT ( 'NONE',  ( 11.08653569745442091, 56.26057688450584493, -4.438844214435508029 ) ) ;
#23900 = CARTESIAN_POINT ( 'NONE',  ( -58.34682947232719386, -0.2434262655763852479, 0.1887554165967793296 ) ) ;
#23901 = CARTESIAN_POINT ( 'NONE',  ( -3.984361711520921556, 7.699456178644025428, -2.362637291489932068 ) ) ;
#23902 = CARTESIAN_POINT ( 'NONE',  ( 10.36176036692635627, 123.5464890276372785, 1.327270239784479333 ) ) ;
#23903 = CARTESIAN_POINT ( 'NONE',  ( -0.6138949730159162232, 32.89880662442777748, 0.9453277557968443601 ) ) ;
#23904 = CARTESIAN_POINT ( 'NONE',  ( -0.8068095026012097604, 106.0274289318137306, 5.250488437364327687 ) ) ;
#23905 = CIRCLE ( 'NONE', #6941, 18.13811525448111439 ) ;
#23906 = CIRCLE ( 'NONE', #16424, 0.5080000000000002292 ) ;
#23907 = CARTESIAN_POINT ( 'NONE',  ( -0.6244342276652131707, 19.93415720681881353, -4.586363120317934694 ) ) ;
#23908 = CARTESIAN_POINT ( 'NONE',  ( 15.64343260727701868, 147.2205073051419504, 0.4407941163815357610 ) ) ;
#23909 = CARTESIAN_POINT ( 'NONE',  ( 8.798071512540863282, 117.6842349196870572, 0.1758064070670784795 ) ) ;
#23910 = CARTESIAN_POINT ( 'NONE',  ( -53.75865956017525349, 9.373754164828760338, -3.697140908559944261 ) ) ;
#23911 = CARTESIAN_POINT ( 'NONE',  ( 8.797820204909040598, 117.6963758506564659, 0.06379098981978209570 ) ) ;
#23912 = LINE ( 'NONE', #11135, #33292 ) ;
#23913 = DIRECTION ( 'NONE',  ( -6.353134868986659519E-16, 1.000000000000000000, 0.000000000000000000 ) ) ;
#23914 = CARTESIAN_POINT ( 'NONE',  ( 2.081416901521091933, -15.50639809317535089, 5.943648939154567934 ) ) ;
#23915 = CARTESIAN_POINT ( 'NONE',  ( -29.14841176368481257, 63.09186355668505541, -1.270000000000006013 ) ) ;
#23916 = CARTESIAN_POINT ( 'NONE',  ( -7.781828003681788175, 2.241565531857627303, -3.240848859074576094 ) ) ;
#23917 = DIRECTION ( 'NONE',  ( 5.188838149069472160E-16, -1.699382548006136559E-16, -1.000000000000000000 ) ) ;
#23918 = DIRECTION ( 'NONE',  ( 9.627370216492862708E-17, 1.000000000000000000, -0.000000000000000000 ) ) ;
#23919 = CARTESIAN_POINT ( 'NONE',  ( -57.96050266256141725, 2.261623006455215634, 0.4698253072426024635 ) ) ;
#23920 = CARTESIAN_POINT ( 'NONE',  ( -58.43690671596436914, -0.4125963578781866037, 0.2423173958219003998 ) ) ;
#23921 = CARTESIAN_POINT ( 'NONE',  ( -18.56067064112295739, 154.1690995007799927, 0.05235235476399380250 ) ) ;
#23922 = EDGE_LOOP ( 'NONE', ( #4636, #24518, #28179, #424 ) ) ;
#23923 = CARTESIAN_POINT ( 'NONE',  ( -57.73934301000005576, 2.737667398473711433, -1.050169850737068478 ) ) ;
#23924 = CARTESIAN_POINT ( 'NONE',  ( 6.995241510662618900, 121.9554695571096516, 0.1163068145497427736 ) ) ;
#23925 =( BOUNDED_SURFACE ( )  B_SPLINE_SURFACE ( 3, 2, ( 
 ( #29252, #22628, #12233 ),
 ( #22420, #22837, #6474 ),
 ( #38850, #38440, #3287 ),
 ( #38229, #28840, #96 ),
 ( #2455, #6067, #28626 ),
 ( #9043, #13063, #29042 ) ),
 .UNSPECIFIED., .F., .F., .T. ) 
 B_SPLINE_SURFACE_WITH_KNOTS ( ( 4, 2, 4 ),
 ( 3, 3 ),
 ( 0.000000000000000000, 0.0007381999790946839474, 0.001476399958189367895 ),
 ( 0.000000000000000000, 1.000000000000000000 ),
 .UNSPECIFIED. ) 
 GEOMETRIC_REPRESENTATION_ITEM ( )  RATIONAL_B_SPLINE_SURFACE ( (
 ( 1.000000000000000000, 0.7071067811865388020, 1.000000000000000000),
 ( 1.000000000000000000, 0.7071031648627850164, 1.000000000000000000),
 ( 1.000000000000000000, 0.7049885726730517055, 1.000000000000000000),
 ( 1.000000000000000000, 0.6987948356720484755, 1.000000000000000000),
 ( 1.000000000000000000, 0.6949210395580179833, 1.000000000000000000),
 ( 1.000000000000000000, 0.6916534930270952231, 1.000000000000000000) ) ) 
 REPRESENTATION_ITEM ( '' )  SURFACE ( )  );
#23926 = ORIENTED_EDGE ( 'NONE', *, *, #35977, .T. ) ;
#23927 = CARTESIAN_POINT ( 'NONE',  ( 16.60960244842765832, 17.14499999999999957, 2.034089647357696937E-15 ) ) ;
#23928 = CARTESIAN_POINT ( 'NONE',  ( -8.770618086121094947, 123.6813396614493712, -0.1752578222716850986 ) ) ;
#23929 = CARTESIAN_POINT ( 'NONE',  ( 2.079616623477898329, -15.54617723206731839, 5.925385729176050553 ) ) ;
#23930 = CARTESIAN_POINT ( 'NONE',  ( -20.71566368020606319, 149.2407879669073054, 1.563226885547172929 ) ) ;
#23931 = CARTESIAN_POINT ( 'NONE',  ( 2.832181158176134250, 116.7549172960530939, 0.3515502119895596023 ) ) ;
#23932 = DIRECTION ( 'NONE',  ( -6.353134868986659519E-16, 1.000000000000000000, -0.000000000000000000 ) ) ;
#23933 = CARTESIAN_POINT ( 'NONE',  ( -4.559029627765868398, 31.49133049583988253, -0.6947656260628575220 ) ) ;
#23934 = CARTESIAN_POINT ( 'NONE',  ( -21.47487836045326048, 132.5742979909900328, -0.7254175812904735121 ) ) ;
#23935 = CARTESIAN_POINT ( 'NONE',  ( -50.39203423948032423, 15.66273372407933273, -4.838163006325442161 ) ) ;
#23936 = CARTESIAN_POINT ( 'NONE',  ( 4.812022206586005879, 117.4092931151362933, 1.196645100868244604 ) ) ;
#23937 = CARTESIAN_POINT ( 'NONE',  ( -2.199325300168501585, 116.2221077253555137, 0.01996347552337981307 ) ) ;
#23938 = CARTESIAN_POINT ( 'NONE',  ( -12.06094766868699431, 124.3217332413628640, 1.226997676231849077 ) ) ;
#23939 = CARTESIAN_POINT ( 'NONE',  ( -58.22348609355718452, 0.02088251804533911363, -0.5098280860662359748 ) ) ;
#23940 = CARTESIAN_POINT ( 'NONE',  ( 19.50591060256576270, 149.0830822498907082, -1.724197071773047485 ) ) ;
#23941 = CARTESIAN_POINT ( 'NONE',  ( 0.3740510792576948185, -8.494654975422754717, 0.8997923438783246297 ) ) ;
#23942 = CARTESIAN_POINT ( 'NONE',  ( -20.18025034597674860, 150.8812763393641490, -2.199297964380012349 ) ) ;
#23943 = CARTESIAN_POINT ( 'NONE',  ( -47.61549956331938205, 19.66157307908738261, -5.197827534590572895 ) ) ;
#23944 = AXIS2_PLACEMENT_3D ( 'NONE', #8583, #31999, #2838 ) ;
#23945 = CARTESIAN_POINT ( 'NONE',  ( 4.307098852976651848, 104.6144662015478701, 3.166141611896306607 ) ) ;
#23946 = CARTESIAN_POINT ( 'NONE',  ( 10.15138120625587348, 123.9924233945428682, -0.7101534938561538945 ) ) ;
#23947 = CARTESIAN_POINT ( 'NONE',  ( -17.68910244842765778, 0.6350000000000018963, 2.166290269325653984E-15 ) ) ;
#23948 = VERTEX_POINT ( 'NONE', #25795 ) ;
#23949 = CARTESIAN_POINT ( 'NONE',  ( -11.39530606461031326, 123.1738952066917534, -1.661446624139454542 ) ) ;
#23950 = CARTESIAN_POINT ( 'NONE',  ( 4.496247062743834455, -15.66418688627994804, 3.575535799018406014 ) ) ;
#23951 = DIRECTION ( 'NONE',  ( 0.1906721105965043517, -0.9816537812491096249, 2.657572025465705161E-16 ) ) ;
#23952 = CARTESIAN_POINT ( 'NONE',  ( -4.434103822380226489, 118.1614506541414897, -0.6149899926561507302 ) ) ;
#23953 = CARTESIAN_POINT ( 'NONE',  ( -50.29507671575587580, 15.72791930032350827, -4.796563717952114558 ) ) ;
#23954 = CARTESIAN_POINT ( 'NONE',  ( -4.792324638262704717, 56.51998046905272588, -4.972049999962482758 ) ) ;
#23955 = CARTESIAN_POINT ( 'NONE',  ( 17.78478073489614886, 148.4245508482893854, 2.330447787059698239 ) ) ;
#23956 = CARTESIAN_POINT ( 'NONE',  ( -36.43259636504752308, 28.15155085495446485, 1.269999999999994911 ) ) ;
#23957 = VECTOR ( 'NONE', #17318, 999.9999999999998863 ) ;
#23958 = CARTESIAN_POINT ( 'NONE',  ( 8.216926545874459364, 117.5004104479096583, 0.1641937475849289951 ) ) ;
#23959 = CARTESIAN_POINT ( 'NONE',  ( 7.433834689873759061, 17.99627214424885580, -4.034796628604029323 ) ) ;
#23960 = CARTESIAN_POINT ( 'NONE',  ( 8.161245858290078203, 122.8283871457973362, 0.4521822771171598032 ) ) ;
#23961 = CARTESIAN_POINT ( 'NONE',  ( 14.88832262945823537, 121.0052616771249347, -0.5340607732653416262 ) ) ;
#23962 = DIRECTION ( 'NONE',  ( 4.017660918040594346E-17, -1.000000000000000000, -2.376309959284834438E-19 ) ) ;
#23963 = CARTESIAN_POINT ( 'NONE',  ( -3.630816577625875226E-14, 57.14999999999999147, 0.000000000000000000 ) ) ;
#23964 = AXIS2_PLACEMENT_3D ( 'NONE', #14177, #4625, #8011 ) ;
#23965 = CARTESIAN_POINT ( 'NONE',  ( -57.35932467317038430, 1.578336987915054834, 0.2403330148843857983 ) ) ;
#23966 = CARTESIAN_POINT ( 'NONE',  ( -23.38383716176070948, 142.7868430859564626, -0.3143897558744216947 ) ) ;
#23967 = ORIENTED_EDGE ( 'NONE', *, *, #36211, .F. ) ;
#23968 = CARTESIAN_POINT ( 'NONE',  ( -46.71787546252079437, 26.08696747599453047, -0.2117558669993572784 ) ) ;
#23969 = CARTESIAN_POINT ( 'NONE',  ( -6.868495830644764766, 121.6811238109402211, -0.6472389319075357861 ) ) ;
#23970 = CARTESIAN_POINT ( 'NONE',  ( -8.618292403345975572, 118.6571538964700352, 0.8118115907003122800 ) ) ;
#23971 = ORIENTED_EDGE ( 'NONE', *, *, #38918, .F. ) ;
#23972 = CARTESIAN_POINT ( 'NONE',  ( 1.614075274083550671, 118.7629491485467952, -1.182329714217916106 ) ) ;
#23973 = CARTESIAN_POINT ( 'NONE',  ( -15.64569453857185977, 147.5723176251010784, -0.9037163853702844252 ) ) ;
#23974 = CARTESIAN_POINT ( 'NONE',  ( 4.939475803799734166, -12.60685243851100701, 2.184682653711520040 ) ) ;
#23975 = CARTESIAN_POINT ( 'NONE',  ( -22.39365319421761313, 148.6363688457942942, 0.9991490326925100973 ) ) ;
#23976 = CARTESIAN_POINT ( 'NONE',  ( -41.09670346151854403, 23.04688172093031895, 1.270085369932502095 ) ) ;
#23977 = CARTESIAN_POINT ( 'NONE',  ( 3.714261611334540358, 116.6275173757784813, 0.1151834636560012531 ) ) ;
#23978 = CARTESIAN_POINT ( 'NONE',  ( -24.46582648842864316, 82.15028593570633575, 1.269999999999993356 ) ) ;
#23979 = CARTESIAN_POINT ( 'NONE',  ( 2.862861873098513588, -10.07698056833738320, -3.640125809621840069 ) ) ;
#23980 = CARTESIAN_POINT ( 'NONE',  ( -20.69909148798433662, 152.5508394022679113, -0.4136171090298727537 ) ) ;
#23981 = FACE_OUTER_BOUND ( 'NONE', #34029, .T. ) ;
#23982 = AXIS2_PLACEMENT_3D ( 'NONE', #32034, #25439, #25842 ) ;
#23983 = CARTESIAN_POINT ( 'NONE',  ( -10.84307050033138431, 78.30450799593342026, -1.523999999999998911 ) ) ;
#23984 = ORIENTED_EDGE ( 'NONE', *, *, #42044, .F. ) ;
#23985 = CARTESIAN_POINT ( 'NONE',  ( 8.089976846435130042, 121.0247124080762120, 1.331332829722204680 ) ) ;
#23986 = CARTESIAN_POINT ( 'NONE',  ( -4.360315236241580017, -1.596229544307166348, -1.535301415559372940 ) ) ;
#23987 = CARTESIAN_POINT ( 'NONE',  ( 2.036215858770189513, 117.3535355059730705, 0.5825239229278259545 ) ) ;
#23988 = CARTESIAN_POINT ( 'NONE',  ( -48.98643424070617414, 17.83616253325781642, -5.099923142903347362 ) ) ;
#23989 = CARTESIAN_POINT ( 'NONE',  ( 13.44120003175020628, 122.0388263298542739, -1.206224284286116610 ) ) ;
#23990 = CARTESIAN_POINT ( 'NONE',  ( -4.434453077421578904, -10.21728329253013179, 1.368390957472948921 ) ) ;
#23991 = CARTESIAN_POINT ( 'NONE',  ( -14.92386488306811465, 121.2513550155162960, -1.224273950129214583 ) ) ;
#23992 = EDGE_CURVE ( 'NONE', #6508, #18747, #30878, .T. ) ;
#23993 = ORIENTED_EDGE ( 'NONE', *, *, #31869, .F. ) ;
#23994 = CARTESIAN_POINT ( 'NONE',  ( -3.725873884401474267, 121.0563512343167645, 0.03194638937107886073 ) ) ;
#23995 = CARTESIAN_POINT ( 'NONE',  ( 4.537411113424957065, -14.92057169651182846, 4.687841795668383327 ) ) ;
#23996 = CARTESIAN_POINT ( 'NONE',  ( 0.000000000000000000, -2.099656937138137170E-16, 0.000000000000000000 ) ) ;
#23997 = VECTOR ( 'NONE', #13204, 1000.000000000000000 ) ;
#23998 = CARTESIAN_POINT ( 'NONE',  ( -0.3344305141284643068, 117.9496053196974259, -1.408475212110079200 ) ) ;
#23999 = EDGE_CURVE ( 'NONE', #38197, #9800, #16613, .T. ) ;
#24000 = EDGE_LOOP ( 'NONE', ( #15614, #9050, #8236, #34472 ) ) ;
#24001 = CARTESIAN_POINT ( 'NONE',  ( 12.39214084994775966, 122.8403290575659526, 1.822206477283890624 ) ) ;
#24002 = CARTESIAN_POINT ( 'NONE',  ( 4.877618761170128714, 117.7099338327117550, 0.9252109555340380931 ) ) ;
#24003 = CARTESIAN_POINT ( 'NONE',  ( 4.756814333351318425, 117.4032681585794791, 1.206529664789174339 ) ) ;
#24004 = AXIS2_PLACEMENT_3D ( 'NONE', #27429, #14838, #21429 ) ;
#24005 = CARTESIAN_POINT ( 'NONE',  ( -21.96051921721475964, 150.3855106993079005, 0.8576051660729392401 ) ) ;
#24006 = CARTESIAN_POINT ( 'NONE',  ( 8.423846519715326053, 3.801276092563157682, 0.04266398729441032295 ) ) ;
#24007 = CARTESIAN_POINT ( 'NONE',  ( 16.00153516066838932, 147.3640369757652877, 1.286050259728349632 ) ) ;
#24008 = DIRECTION ( 'NONE',  ( 1.000000000000000000, -1.365923996832131856E-16, 0.000000000000000000 ) ) ;
#24009 = PRODUCT_DEFINITION ( 'UNKNOWN', '', #40070, #12917 ) ;
#24010 = CARTESIAN_POINT ( 'NONE',  ( 23.01821387067764846, 149.5377445326608665, -0.2676165590851171672 ) ) ;
#24011 = DIRECTION ( 'NONE',  ( -0.8745520943968130290, 0.4849315768086749356, -6.829619984160618603E-16 ) ) ;
#24012 = CARTESIAN_POINT ( 'NONE',  ( -57.51365629832210402, 1.555024991728927830, 1.385071661654051267 ) ) ;
#24013 =( LENGTH_UNIT ( ) NAMED_UNIT ( * ) SI_UNIT ( .MILLI., .METRE. ) );
#24014 = CARTESIAN_POINT ( 'NONE',  ( -57.81953393267934160, 1.609514594907199392, 1.636666387507130782 ) ) ;
#24015 = CARTESIAN_POINT ( 'NONE',  ( -58.52180102370724057, -0.06713305130389136954, 0.6434702267309780899 ) ) ;
#24016 = ADVANCED_FACE ( 'NONE', ( #19400 ), #35613, .T. ) ;
#24017 = CARTESIAN_POINT ( 'NONE',  ( -4.493334425098775675, 118.1300705548361378, 0.5259396578861340599 ) ) ;
#24018 = DIRECTION ( 'NONE',  ( -0.8745520943968240202, 0.4849315768086553402, -6.829619984160650158E-16 ) ) ;
#24019 = ORIENTED_EDGE ( 'NONE', *, *, #38059, .T. ) ;
#24020 = CARTESIAN_POINT ( 'NONE',  ( -42.09814309847200064, 23.46876350539121248, 1.523999999999994026 ) ) ;
#24021 = EDGE_CURVE ( 'NONE', #1232, #11667, #448, .T. ) ;
#24022 = CARTESIAN_POINT ( 'NONE',  ( -3.979033859436909459, 119.1284811785372426, -0.9228774962003568616 ) ) ;
#24023 = CARTESIAN_POINT ( 'NONE',  ( -5.947819151547508731, 118.9610140496397719, -0.5876226394569609157 ) ) ;
#24024 = VECTOR ( 'NONE', #10931, 1000.000000000000000 ) ;
#24025 = CARTESIAN_POINT ( 'NONE',  ( 4.157985138387068069, 118.2393596361145427, 0.3861799695154242706 ) ) ;
#24026 = CARTESIAN_POINT ( 'NONE',  ( -14.76847666019565253, 139.2804412874323248, -1.275673245633013320 ) ) ;
#24027 = CARTESIAN_POINT ( 'NONE',  ( -0.5849308179726303569, 115.7029860318907737, -1.760411360667945013 ) ) ;
#24028 = EDGE_CURVE ( 'NONE', #21265, #37727, #33628, .T. ) ;
#24029 = CARTESIAN_POINT ( 'NONE',  ( 1.042872747090432206, 117.9496053355046996, -1.352030660431440268 ) ) ;
#24030 = ORIENTED_EDGE ( 'NONE', *, *, #27647, .F. ) ;
#24031 = CARTESIAN_POINT ( 'NONE',  ( 6.742182786528933214, 121.2177056076135528, -0.07361405433131842924 ) ) ;
#24032 = CARTESIAN_POINT ( 'NONE',  ( -1.805426509874352048, 156.5029897098349636, -1.055579731365336116 ) ) ;
#24033 = CARTESIAN_POINT ( 'NONE',  ( -5.329450492226126990, 104.6144662015457243, -0.2809636609891541514 ) ) ;
#24034 = AXIS2_PLACEMENT_3D ( 'NONE', #41047, #17815, #18227 ) ;
#24035 = CARTESIAN_POINT ( 'NONE',  ( -45.60639265695088795, 20.98815520443602978, 4.238054969589494902 ) ) ;
#24036 = CARTESIAN_POINT ( 'NONE',  ( -17.14500000000466784, 71.11999999999886768, 1.523999999999998689 ) ) ;
#24037 = CARTESIAN_POINT ( 'NONE',  ( 6.079889191864811693, 121.4459138098642086, 0.1214906558318714913 ) ) ;
#24038 = DIRECTION ( 'NONE',  ( -1.000000000000000000, 0.000000000000000000, 0.000000000000000000 ) ) ;
#24039 = CARTESIAN_POINT ( 'NONE',  ( 15.29070941918896409, 121.1074504348956964, 0.9956366180447248082 ) ) ;
#24040 = DIRECTION ( 'NONE',  ( -1.000000000000000000, 0.000000000000000000, 0.000000000000000000 ) ) ;
#24041 = CARTESIAN_POINT ( 'NONE',  ( 3.231433726605559276, -14.53588044659766254, 1.883291753459793716 ) ) ;
#24042 = CARTESIAN_POINT ( 'NONE',  ( -18.09865239071517351, 149.0664087073519681, 1.700023788287825521 ) ) ;
#24043 = CARTESIAN_POINT ( 'NONE',  ( 0.5763570944828283471, -5.266575483494631449, -0.7860673829877594665 ) ) ;
#24044 = CARTESIAN_POINT ( 'NONE',  ( -22.11976774214192432, 136.9573810088325843, -1.270382039940954000 ) ) ;
#24045 = CIRCLE ( 'NONE', #5705, 0.6350000000000001199 ) ;
#24046 = CARTESIAN_POINT ( 'NONE',  ( 0.9581548452940278349, 12.22225311242794099, 0.1719060106794997322 ) ) ;
#24047 = ORIENTED_EDGE ( 'NONE', *, *, #27736, .T. ) ;
#24048 = CARTESIAN_POINT ( 'NONE',  ( -49.81365592435692236, 14.60358288955459294, 2.185970286000758822 ) ) ;
#24049 = ITEM_DEFINED_TRANSFORMATION ( 'NONE', 'NONE', #20268,  #3275 ) ;
#24050 = CARTESIAN_POINT ( 'NONE',  ( -16.03056103447438829, 147.0154580547469152, 0.5309802628845388117 ) ) ;
#24051 = CARTESIAN_POINT ( 'NONE',  ( 2.039565395400614989, -15.13835760176744571, 5.886961163765535687 ) ) ;
#24052 = CARTESIAN_POINT ( 'NONE',  ( 16.13547353508407411, 149.3012944676311804, -1.369731486774125040 ) ) ;
#24053 = ORIENTED_EDGE ( 'NONE', *, *, #8457, .F. ) ;
#24054 = CARTESIAN_POINT ( 'NONE',  ( 4.799643950526473191, 115.7029491485453292, 1.472414092453835588 ) ) ;
#24055 = CARTESIAN_POINT ( 'NONE',  ( 3.317891647977158076, -14.03051783662405327, 3.455980060616059113 ) ) ;
#24056 = CARTESIAN_POINT ( 'NONE',  ( -4.958175139285456723, 117.4049635120808972, -1.028653955280601773 ) ) ;
#24057 = CARTESIAN_POINT ( 'NONE',  ( 11.11302231477177394, 128.0707465396788507, 0.1214933242792291812 ) ) ;
#24058 = EDGE_LOOP ( 'NONE', ( #25243, #1663, #7886, #21716 ) ) ;
#24059 = CARTESIAN_POINT ( 'NONE',  ( 20.37866581877382544, 147.6366098820875266, 2.483541293540720840 ) ) ;
#24060 = CARTESIAN_POINT ( 'NONE',  ( 3.009822844306053735, 107.7309519196189882, 4.394584667970089065 ) ) ;
#24061 = CIRCLE ( 'NONE', #35634, 3.175000000000001155 ) ;
#24062 = CARTESIAN_POINT ( 'NONE',  ( -3.932819197772146946, 27.98301002373794333, 0.4898618918306564263 ) ) ;
#24063 = LINE ( 'NONE', #1926, #15675 ) ;
#24064 = EDGE_CURVE ( 'NONE', #7720, #32811, #41107, .T. ) ;
#24065 = AXIS2_PLACEMENT_3D ( 'NONE', #1361, #734, #1577 ) ;
#24066 = CARTESIAN_POINT ( 'NONE',  ( 8.212232005054447725, 117.5299140688306352, -0.02651185805045432747 ) ) ;
#24067 = EDGE_CURVE ( 'NONE', #1690, #4252, #988, .T. ) ;
#24068 = CARTESIAN_POINT ( 'NONE',  ( -24.57769139521899149, 76.70147894597536720, -1.524000000000005572 ) ) ;
#24069 = AXIS2_PLACEMENT_3D ( 'NONE', #24476, #37480, #4503 ) ;
#24070 = CARTESIAN_POINT ( 'NONE',  ( 1.929093603856297579, -15.52458459146700775, 5.992193855007914571 ) ) ;
#24071 = DIRECTION ( 'NONE',  ( 6.829619984160660610E-15, 0.000000000000000000, 1.000000000000000000 ) ) ;
#24072 = CARTESIAN_POINT ( 'NONE',  ( -4.973366403791914081, 117.3993836135847459, -0.9761750303810099449 ) ) ;
#24073 = CARTESIAN_POINT ( 'NONE',  ( 20.59518377851916426, 148.5655811199389689, 2.440016074255365819 ) ) ;
#24074 = ORIENTED_EDGE ( 'NONE', *, *, #23543, .F. ) ;
#24075 = CARTESIAN_POINT ( 'NONE',  ( -8.412017540776835389, 12.59877214424737524, 0.8828606482577823211 ) ) ;
#24076 = CARTESIAN_POINT ( 'NONE',  ( -2.262502884342421527, 117.0718098024412086, -0.6252834037462153827 ) ) ;
#24077 = CARTESIAN_POINT ( 'NONE',  ( -3.352959238113231155, 119.3320731715853782, -0.6187547705018832112 ) ) ;
#24079 = DIRECTION ( 'NONE',  ( 0.9998004120163609398, 0.000000000000000000, 0.01997839162482749689 ) ) ;
#24078 = VECTOR ( 'NONE', #19537, 999.9999999999998863 ) ;
#24080 = DIRECTION ( 'NONE',  ( 6.353134868986659519E-16, -1.000000000000000000, 0.000000000000000000 ) ) ;
#24081 = CARTESIAN_POINT ( 'NONE',  ( -0.0002200197270972112785, 124.8375573595198063, 0.01101068683960106966 ) ) ;
#24082 = CARTESIAN_POINT ( 'NONE',  ( 2.267534764145236803, 6.115564135048844108, 4.037922524061999141 ) ) ;
#24083 = ADVANCED_FACE ( 'NONE', ( #19195 ), #26596, .F. ) ;
#24084 = CARTESIAN_POINT ( 'NONE',  ( -28.36525985791271154, 77.02308833105713859, -1.524000000000007571 ) ) ;
#24085 = CARTESIAN_POINT ( 'NONE',  ( -5.176291933393869726, 115.6909491485453003, 1.072167014217356051 ) ) ;
#24086 = CARTESIAN_POINT ( 'NONE',  ( 3.202083396006969895, -13.65749169606385394, 1.964591208077046902 ) ) ;
#24087 = CARTESIAN_POINT ( 'NONE',  ( 4.418733742721376423, 119.2572634999566930, -0.4175613206465202398 ) ) ;
#24088 = CARTESIAN_POINT ( 'NONE',  ( 2.445139878417788015, 38.86123358755037316, 1.352914556568929116 ) ) ;
#24089 = DIRECTION ( 'NONE',  ( 0.6559537821943262070, -0.7548010569845264861, 8.537024980200723210E-16 ) ) ;
#24090 = ORIENTED_EDGE ( 'NONE', *, *, #8464, .T. ) ;
#24091 = CARTESIAN_POINT ( 'NONE',  ( -3.265249574949038891, 104.6144662015457243, -3.566735880799804637 ) ) ;
#24092 = VECTOR ( 'NONE', #29074, 1000.000000000000114 ) ;
#24093 = CARTESIAN_POINT ( 'NONE',  ( 3.468122426543017500, -15.77657449013483770, 4.627414140463686820 ) ) ;
#24094 = CARTESIAN_POINT ( 'NONE',  ( -12.91500497980672968, 122.5866728308148055, 1.316509475493082393 ) ) ;
#24095 = EDGE_CURVE ( 'NONE', #6738, #16059, #29546, .T. ) ;
#24096 = CARTESIAN_POINT ( 'NONE',  ( 0.3213417908193094141, 16.26526798020547204, 0.9222100932699727194 ) ) ;
#24097 = VERTEX_POINT ( 'NONE', #31098 ) ;
#24098 = ORIENTED_EDGE ( 'NONE', *, *, #35051, .T. ) ;
#24099 = CARTESIAN_POINT ( 'NONE',  ( -6.559134203278485842, 78.24119908707510263, 1.524000000000002908 ) ) ;
#24100 = CARTESIAN_POINT ( 'NONE',  ( 2.327304502367511851, 119.2037781873646622, 0.6856724729282703823 ) ) ;
#24101 = CARTESIAN_POINT ( 'NONE',  ( -16.74402619291562289, 146.1290494286844819, 1.112937342747913894 ) ) ;
#24102 = CARTESIAN_POINT ( 'NONE',  ( 6.984999999999963904, 57.14999999999999858, 8.554157892044261576E-16 ) ) ;
#24103 = CARTESIAN_POINT ( 'NONE',  ( 0.03066982525775350035, 157.3074135339440147, -1.534843470138540500 ) ) ;
#24104 = CARTESIAN_POINT ( 'NONE',  ( -11.75177080394836615, 120.8928578745602209, -1.619740935434792251 ) ) ;
#24105 = DIRECTION ( 'NONE',  ( 0.1906721105965055174, -0.9816537812491091808, 0.000000000000000000 ) ) ;
#24106 = ORIENTED_EDGE ( 'NONE', *, *, #2446, .T. ) ;
#24107 = CARTESIAN_POINT ( 'NONE',  ( 4.157314486619299920, 118.2390909874852269, -0.2343065005310382420 ) ) ;
#24108 = CARTESIAN_POINT ( 'NONE',  ( 9.006799368204273293, 123.6974368934138226, -0.1328627719367737048 ) ) ;
#24109 = ORIENTED_EDGE ( 'NONE', *, *, #2466, .T. ) ;
#24110 = CARTESIAN_POINT ( 'NONE',  ( 3.131015516031846690, -14.62848841321586946, 3.524024012273756501 ) ) ;
#24111 = CARTESIAN_POINT ( 'NONE',  ( 12.16475753114684011, 55.74362973025083079, -5.016500000000000625 ) ) ;
#24112 = CARTESIAN_POINT ( 'NONE',  ( -55.76611385812141464, 5.250064693407802352, 2.603441191288020207 ) ) ;
#24113 = CARTESIAN_POINT ( 'NONE',  ( 1.173990663012069113, -13.46572784750561880, -4.469126434461346165 ) ) ;
#24114 = CARTESIAN_POINT ( 'NONE',  ( 16.97388159461585388, 146.7604995623492243, 1.927701477367710803 ) ) ;
#24115 = CARTESIAN_POINT ( 'NONE',  ( -0.8695339520022613566, 32.00309925763205854, 2.544523118616357937 ) ) ;
#24116 = CARTESIAN_POINT ( 'NONE',  ( -4.798759560708047545, 116.6039038697339549, 0.9352253033319917197 ) ) ;
#24117 = CARTESIAN_POINT ( 'NONE',  ( 3.465721614298269415, 18.43485028915299750, -3.064284189100199729 ) ) ;
#24118 = CARTESIAN_POINT ( 'NONE',  ( 0.6448247514296147065, 156.3042436901572216, 0.08557349692115868989 ) ) ;
#24119 = CARTESIAN_POINT ( 'NONE',  ( 4.760771785401275658, 118.7629491485453030, 0.9361126076443277988 ) ) ;
#24120 = CARTESIAN_POINT ( 'NONE',  ( -57.63883995378735392, 1.113466886629776997, -0.4249547484444705647 ) ) ;
#24121 = CARTESIAN_POINT ( 'NONE',  ( 8.793698859918160693, 117.7268288381244901, -0.04247273347103042163 ) ) ;
#24122 = CARTESIAN_POINT ( 'NONE',  ( -20.83467972660109169, 65.95194780259438971, 5.016499999999999737 ) ) ;
#24123 = DIRECTION ( 'NONE',  ( 5.188838149069472160E-16, -1.699382548006136559E-16, -1.000000000000000000 ) ) ;
#24124 = DIRECTION ( 'NONE',  ( -0.9575201071113191853, 0.2883665106726643890, 1.122696976216276426E-15 ) ) ;
#24125 = DIRECTION ( 'NONE',  ( -0.9816537812491089587, -0.1906721105965065444, -4.769617732184475162E-16 ) ) ;
#24126 = CARTESIAN_POINT ( 'NONE',  ( -7.580879709009198386, 3.543476842659112780, 3.722543307504006194 ) ) ;
#24127 = EDGE_CURVE ( 'NONE', #35799, #12743, #11583, .T. ) ;
#24128 = CARTESIAN_POINT ( 'NONE',  ( 5.326632231018254338, 115.7029491485453150, 0.4166893323572425367 ) ) ;
#24129 = DIRECTION ( 'NONE',  ( -4.017660918040594346E-17, 1.000000000000000000, 2.376309959284834438E-19 ) ) ;
#24130 = CARTESIAN_POINT ( 'NONE',  ( -58.16194989728258946, 1.772972946764553193, -1.047404914941014506E-14 ) ) ;
#24131 = CARTESIAN_POINT ( 'NONE',  ( 0.009645608629770095407, 120.9711055683165597, -0.4827056984856004096 ) ) ;
#24132 = CARTESIAN_POINT ( 'NONE',  ( -23.27509581586244636, 146.7258352529021863, 0.1368228026537803843 ) ) ;
#24133 = ORIENTED_EDGE ( 'NONE', *, *, #1717, .F. ) ;
#24134 = CARTESIAN_POINT ( 'NONE',  ( -57.70501761738805158, 2.967533670478833763, -0.5494564739991270041 ) ) ;
#24135 = EDGE_CURVE ( 'NONE', #4116, #34378, #24699, .T. ) ;
#24136 = ORIENTED_EDGE ( 'NONE', *, *, #8389, .T. ) ;
#24137 = CARTESIAN_POINT ( 'NONE',  ( -45.09675090430819466, 21.02858785303356370, -3.680331723257411092 ) ) ;
#24138 = CARTESIAN_POINT ( 'NONE',  ( -15.21351360038804579, 143.4186079242267340, -0.3040022078858841126 ) ) ;
#24139 = CARTESIAN_POINT ( 'NONE',  ( 4.031817627494778122, -15.29123897636591778, 5.054998095871475527 ) ) ;
#24140 = CARTESIAN_POINT ( 'NONE',  ( -0.4301208033650349982, 117.9789173577105572, 0.5453690669796715795 ) ) ;
#24141 = CARTESIAN_POINT ( 'NONE',  ( 2.968319594835611142, 117.2422168882539211, -0.4889809032577732140 ) ) ;
#24142 = CARTESIAN_POINT ( 'NONE',  ( -30.55012479247526613, 56.28806726182424569, 1.269999999999993801 ) ) ;
#24143 = CARTESIAN_POINT ( 'NONE',  ( -18.58235751530899549, 154.1615476314759974, -0.6802042707109061670 ) ) ;
#24144 = CARTESIAN_POINT ( 'NONE',  ( -49.49989884566186049, 17.08151615281530056, -5.027407696123642467 ) ) ;
#24145 = ORIENTED_EDGE ( 'NONE', *, *, #16295, .T. ) ;
#24146 = CARTESIAN_POINT ( 'NONE',  ( -2.184363492873007573, 116.1951706087090628, -0.02372223639846659723 ) ) ;
#24147 = CARTESIAN_POINT ( 'NONE',  ( -12.17146470397786473, 153.5325627063460843, 1.540419412064476301 ) ) ;
#24148 = CARTESIAN_POINT ( 'NONE',  ( -58.28173089090353187, -0.1048243024652170952, -0.3852004869047068181 ) ) ;
#24149 = CARTESIAN_POINT ( 'NONE',  ( 13.20509474233022473, 123.8872625266795211, -1.378179767694161173 ) ) ;
#24150 = CARTESIAN_POINT ( 'NONE',  ( 0.1022289226565744474, -8.938468249466058779, 0.9708619238636220228 ) ) ;
#24151 = CARTESIAN_POINT ( 'NONE',  ( -14.06037840947783657, 121.6707806233237363, -1.579157835890536710 ) ) ;
#24152 = CARTESIAN_POINT ( 'NONE',  ( -47.02779878473986486, 24.11651466984139702, -2.637840241488492943 ) ) ;
#24153 = CARTESIAN_POINT ( 'NONE',  ( 12.52894620082560806, 152.0704867801853766, -0.9584603128924421567 ) ) ;
#24154 = DIRECTION ( 'NONE',  ( -1.000000000000000000, 0.000000000000000000, 5.329070518200751394E-15 ) ) ;
#24155 =( GEOMETRIC_REPRESENTATION_CONTEXT ( 3 ) GLOBAL_UNCERTAINTY_ASSIGNED_CONTEXT ( ( #38916 ) ) GLOBAL_UNIT_ASSIGNED_CONTEXT ( ( #19777, #32797, #35785 ) ) REPRESENTATION_CONTEXT ( 'NONE', 'WORKASPACE' ) );
#24156 = EDGE_LOOP ( 'NONE', ( #22859, #8033, #7054, #23069, #25205 ) ) ;
#24157 = CARTESIAN_POINT ( 'NONE',  ( -15.09997037988956592, 131.2890697635526465, -2.122864649987122654 ) ) ;
#24158 = CARTESIAN_POINT ( 'NONE',  ( 4.790902082350968705, -15.53225359860559074, 1.708430371912022849 ) ) ;
#24159 = CARTESIAN_POINT ( 'NONE',  ( 10.92199999999999704, 17.14499999999999957, -5.850485014536587995E-17 ) ) ;
#24160 = CARTESIAN_POINT ( 'NONE',  ( -4.280007282747122055, 118.2143720721413302, -0.5181209095560703748 ) ) ;
#24161 = CARTESIAN_POINT ( 'NONE',  ( -54.32300027520380326, 9.724537220608771904, -3.743864951777645445 ) ) ;
#24162 = CARTESIAN_POINT ( 'NONE',  ( 4.112716839357073439, 118.2429491485453354, 0.3453384130802144014 ) ) ;
#24163 = CARTESIAN_POINT ( 'NONE',  ( 3.383623802199790642, 119.6896249646678569, 0.8128912582704553857 ) ) ;
#24164 = DIRECTION ( 'NONE',  ( 0.9998004120163609398, 4.016384292689130894E-17, 0.01997839162482749689 ) ) ;
#24165 = CARTESIAN_POINT ( 'NONE',  ( 20.69909148798420517, 152.5508394022679113, 0.4136171090298729758 ) ) ;
#24166 = CARTESIAN_POINT ( 'NONE',  ( 2.985612812371020386, 19.08565862607713370, -7.890306666671915714 ) ) ;
#24167 = CARTESIAN_POINT ( 'NONE',  ( 15.83762317627076044, 145.9541952667573810, 0.7712195890315687308 ) ) ;
#24168 = CARTESIAN_POINT ( 'NONE',  ( -58.07447437077728125, 1.735896131820596766, -1.499107834811110429 ) ) ;
#24169 = CARTESIAN_POINT ( 'NONE',  ( -45.61851195612273813, 20.88128798641513129, -4.109017096224391707 ) ) ;
#24170 = DIRECTION ( 'NONE',  ( -4.017660918040594346E-17, 1.000000000000000000, 2.376309959284834438E-19 ) ) ;
#24171 = CARTESIAN_POINT ( 'NONE',  ( -58.37241122568487128, -0.2962816677227753104, 0.2416009568453807155 ) ) ;
#24172 = EDGE_CURVE ( 'NONE', #35654, #27477, #27694, .T. ) ;
#24173 = CARTESIAN_POINT ( 'NONE',  ( -0.3004615168032563344, 116.4565202671238069, 0.06108086412306423102 ) ) ;
#24174 = CIRCLE ( 'NONE', #37804, 0.5079999999999997851 ) ;
#24175 = ORIENTED_EDGE ( 'NONE', *, *, #22711, .T. ) ;
#24176 = CARTESIAN_POINT ( 'NONE',  ( -47.15184857521119710, 25.06101562935922900, -0.8929867115423409940 ) ) ;
#24177 = CARTESIAN_POINT ( 'NONE',  ( -6.859007239851394822, 121.6278763642771139, -0.6877149167539079455 ) ) ;
#24178 = CARTESIAN_POINT ( 'NONE',  ( -8.799660282941871969, 117.6859426315424599, -0.07877357120237717114 ) ) ;
#24179 = EDGE_LOOP ( 'NONE', ( #8660, #3736, #21053, #5013 ) ) ;
#24180 = CARTESIAN_POINT ( 'NONE',  ( 0.5329804096432148031, 115.7033785807872448, -1.742916349601860704 ) ) ;
#24181 = CARTESIAN_POINT ( 'NONE',  ( -9.099523502024201349, 123.9936668703698075, -0.3412791990392151642 ) ) ;
#24182 = CARTESIAN_POINT ( 'NONE',  ( 3.112015045868556928, -14.86597822091932564, 5.561823117377171499 ) ) ;
#24183 = CARTESIAN_POINT ( 'NONE',  ( -21.68796372492899849, 149.3076860495818323, 1.274097349589627726 ) ) ;
#24184 = CARTESIAN_POINT ( 'NONE',  ( 5.565035070531680006, 78.91452218770625393, -5.089667964246464393 ) ) ;
#24185 = CARTESIAN_POINT ( 'NONE',  ( 10.80923569951294461, 157.9177219752764358, 0.3353067243844873313 ) ) ;
#24186 = CARTESIAN_POINT ( 'NONE',  ( 14.67500508075654508, 148.8517222230099719, 0.2932415260845993576 ) ) ;
#24187 = ORIENTED_EDGE ( 'NONE', *, *, #32062, .T. ) ;
#24188 = CARTESIAN_POINT ( 'NONE',  ( -0.9756124605737610533, 22.95965383878278843, 0.006055453616918176837 ) ) ;
#24189 = CARTESIAN_POINT ( 'NONE',  ( -1.797937260761374167, 116.4670535197835051, -0.04904229828524075269 ) ) ;
#24190 = DIRECTION ( 'NONE',  ( 6.208586974181048556E-14, 1.531143599749384201E-13, -1.000000000000000000 ) ) ;
#24191 = EDGE_LOOP ( 'NONE', ( #24725, #28846, #34017, #5624 ) ) ;
#24192 = CARTESIAN_POINT ( 'NONE',  ( 4.799643950525145364, 115.7029491485460824, 1.472414092458888879 ) ) ;
#24193 = VERTEX_POINT ( 'NONE', #15319 ) ;
#24194 = CARTESIAN_POINT ( 'NONE',  ( 6.714516028680165505, 120.2572718181749849, 1.207797431051931492 ) ) ;
#24195 = CARTESIAN_POINT ( 'NONE',  ( -4.120466288800530563, -1.808681497221679590, -2.133573495687988597 ) ) ;
#24196 = CARTESIAN_POINT ( 'NONE',  ( 0.3765078121167834135, 117.5049145548240972, 0.4786851384288723366 ) ) ;
#24197 = CARTESIAN_POINT ( 'NONE',  ( -54.56827866224300294, 7.775013980778200384, -3.396949012670559487 ) ) ;
#24198 = CARTESIAN_POINT ( 'NONE',  ( 1.193991991012501419, 158.7113841514841681, -1.470390664574136030 ) ) ;
#24199 = CARTESIAN_POINT ( 'NONE',  ( 4.168288449772385995, -6.568960759998498489, 2.029292378399509378 ) ) ;
#24200 = CARTESIAN_POINT ( 'NONE',  ( -1.027358375535146306, 117.1967307433898640, -0.4586652788708820982 ) ) ;
#24201 = CARTESIAN_POINT ( 'NONE',  ( 4.805135882730054320, 117.7655461501371974, -0.8577152909912308942 ) ) ;
#24202 = ORIENTED_EDGE ( 'NONE', *, *, #10042, .F. ) ;
#24203 = CARTESIAN_POINT ( 'NONE',  ( -15.75440288366326413, 145.7063497038720925, -0.08391657230255379629 ) ) ;
#24204 = CARTESIAN_POINT ( 'NONE',  ( 4.209311184370442049, -15.24947937046475310, 4.910682269069504891 ) ) ;
#24205 = CARTESIAN_POINT ( 'NONE',  ( 5.218844378615158597, 115.6909491485453145, 1.134975959208344598 ) ) ;
#24206 = CYLINDRICAL_SURFACE ( 'NONE', #30821, 15.21260244842765808 ) ;
#24208 = ORIENTED_EDGE ( 'NONE', *, *, #33625, .F. ) ;
#24207 = CIRCLE ( 'NONE', #1802, 5.588000000000006295 ) ;
#24209 = CARTESIAN_POINT ( 'NONE',  ( 18.85642017384686753, 148.8558894138562039, 2.490767737705128493 ) ) ;
#24210 = PRESENTATION_STYLE_ASSIGNMENT (( #2508 ) ) ;
#24211 = ADVANCED_FACE ( 'NONE', ( #41334 ), #1938, .F. ) ;
#24212 = CARTESIAN_POINT ( 'NONE',  ( 10.92199999999999704, 56.51500000000000057, -4.381499999999999950 ) ) ;
#24213 = CARTESIAN_POINT ( 'NONE',  ( -7.640054841935688401, 158.5456267226934131, 0.8603666243017554782 ) ) ;
#24214 = CARTESIAN_POINT ( 'NONE',  ( 3.645047284007026267, 5.522537913078280347, -7.602695550683356451 ) ) ;
#24215 = CARTESIAN_POINT ( 'NONE',  ( -0.005430166084396237554, 120.5648899400503069, 0.2717477157510629904 ) ) ;
#24216 = DIRECTION ( 'NONE',  ( 1.000000000000000000, 0.000000000000000000, 0.000000000000000000 ) ) ;
#24217 = CARTESIAN_POINT ( 'NONE',  ( 18.19405586666655594, 125.1529741258727597, -0.3179404471852274594 ) ) ;
#24218 = DIRECTION ( 'NONE',  ( 5.188838149069472160E-16, -1.699382548006136559E-16, -1.000000000000000000 ) ) ;
#24219 = CARTESIAN_POINT ( 'NONE',  ( -57.90444776229139023, 0.7116094859540841311, 0.9800384988091017657 ) ) ;
#24220 = CARTESIAN_POINT ( 'NONE',  ( -14.38915334913366806, 80.27078028363496287, -1.524000000000001132 ) ) ;
#24221 = CARTESIAN_POINT ( 'NONE',  ( -58.24002838079472610, 0.001074765447070524793, 0.6562585879479657658 ) ) ;
#24222 = CARTESIAN_POINT ( 'NONE',  ( -58.46457299168318400, 0.05672257835903128653, 0.7533826903934722763 ) ) ;
#24223 = EDGE_CURVE ( 'NONE', #11069, #34925, #40442, .T. ) ;
#24224 = DIRECTION ( 'NONE',  ( 0.8745520943968472238, -0.4849315768086133738, -1.512686642312110832E-15 ) ) ;
#24225 = CARTESIAN_POINT ( 'NONE',  ( -4.162552958233026956, 118.2393839662436932, 0.2285457502593932766 ) ) ;
#24226 = CARTESIAN_POINT ( 'NONE',  ( 2.469092600939023274, 107.0260912999244880, -4.723304494335009984 ) ) ;
#24227 = VERTEX_POINT ( 'NONE', #14897 ) ;
#24228 = CARTESIAN_POINT ( 'NONE',  ( -48.65005484009959957, 18.46594748123760965, 5.297328305960426142 ) ) ;
#24229 = CARTESIAN_POINT ( 'NONE',  ( 6.189399099425992645, 119.6256119081757134, -1.002760702448228125 ) ) ;
#24230 = CARTESIAN_POINT ( 'NONE',  ( -5.227511188233297190, 116.2365830367532595, -1.175287748399642451 ) ) ;
#24231 = CARTESIAN_POINT ( 'NONE',  ( 4.439117808263670639, 118.1598832799868291, 0.6092663547203902574 ) ) ;
#24232 = CARTESIAN_POINT ( 'NONE',  ( -15.64597882779404259, 147.9168465093495399, -1.159024332450872663 ) ) ;
#24233 = CARTESIAN_POINT ( 'NONE',  ( 16.60960244842765832, -1.392917743221662552E-16, 0.000000000000000000 ) ) ;
#24234 = CIRCLE ( 'NONE', #29693, 0.2539999999999960067 ) ;
#24235 = ORIENTED_EDGE ( 'NONE', *, *, #10202, .T. ) ;
#24236 = CARTESIAN_POINT ( 'NONE',  ( 5.335400302754617741, 116.6867539651165373, -0.8102459553323388963 ) ) ;
#24237 = CARTESIAN_POINT ( 'NONE',  ( -0.7656893570839061747, 156.6562795458349910, -1.120391489380295313 ) ) ;
#24238 = EDGE_CURVE ( 'NONE', #38830, #28106, #21913, .T. ) ;
#24239 = CARTESIAN_POINT ( 'NONE',  ( -8.816700480405424756, 73.94613776634058411, 1.524000000000002464 ) ) ;
#24240 = CARTESIAN_POINT ( 'NONE',  ( -47.33874550351462318, 19.91900851599329414, 5.121984950673859061 ) ) ;
#24241 = AXIS2_PLACEMENT_3D ( 'NONE', #4824, #16951, #37181 ) ;
#24242 = CARTESIAN_POINT ( 'NONE',  ( -5.525052883313952279, 65.71034362490503611, -1.523999999999993804 ) ) ;
#24243 = CARTESIAN_POINT ( 'NONE',  ( -15.19897562098254618, 143.3954161896175492, -0.1009949650227405238 ) ) ;
#24244 = DIRECTION ( 'NONE',  ( -0.9998004120163609398, 0.000000000000000000, -0.01997839162482749689 ) ) ;
#24245 = CARTESIAN_POINT ( 'NONE',  ( 22.44014329066001423, 150.2745577238280816, 1.412889903812419856 ) ) ;
#24246 = FACE_OUTER_BOUND ( 'NONE', #15944, .T. ) ;
#24248 = CARTESIAN_POINT ( 'NONE',  ( 21.49647223597088797, 141.8478887571778273, -1.286173174470951253 ) ) ;
#24247 = CARTESIAN_POINT ( 'NONE',  ( 2.671714809844681238, -14.97371442308345380, 4.574436322856921144 ) ) ;
#24249 = CARTESIAN_POINT ( 'NONE',  ( -8.477251816686477426, 120.7201681212196291, 1.097727670418841672 ) ) ;
#24250 = CARTESIAN_POINT ( 'NONE',  ( -0.8109939492151988505, -12.39128985057688936, -0.5387275711561630986 ) ) ;
#24251 = CARTESIAN_POINT ( 'NONE',  ( -20.97948398557578642, 132.3427885975763161, -1.200284224572990555 ) ) ;
#24252 = CARTESIAN_POINT ( 'NONE',  ( 0.6214172073067296687, 11.15065110656550118, 0.7500636867869169278 ) ) ;
#24253 = VERTEX_POINT ( 'NONE', #17888 ) ;
#24254 = CARTESIAN_POINT ( 'NONE',  ( -48.50421218116025557, 14.67712143704001626, -7.357606598588287537E-15 ) ) ;
#24255 = CARTESIAN_POINT ( 'NONE',  ( -8.835859712557510903, 123.2701452714374568, 0.3110363621490747077 ) ) ;
#24256 = CARTESIAN_POINT ( 'NONE',  ( 2.546550616605329775, -14.95902107118821078, 5.737972450990987738 ) ) ;
#24257 = CARTESIAN_POINT ( 'NONE',  ( 8.008548550999964988, 121.6949282028273132, -0.7800530928440455591 ) ) ;
#24258 = VERTEX_POINT ( 'NONE', #40702 ) ;
#24259 = AXIS2_PLACEMENT_3D ( 'NONE', #19386, #18968, #31975 ) ;
#24260 = CARTESIAN_POINT ( 'NONE',  ( 0.5918605387268460749, 115.7030220337677378, 1.760228907466973913 ) ) ;
#24261 = CARTESIAN_POINT ( 'NONE',  ( 2.905753382753808900, -13.11311505661566557, 0.7091545436608904796 ) ) ;
#24262 = CARTESIAN_POINT ( 'NONE',  ( -26.01970228765382132, 72.88622078690372064, -1.270000000000005791 ) ) ;
#24263 = ADVANCED_FACE ( 'NONE', ( #40907 ), #5767, .T. ) ;
#24264 = CARTESIAN_POINT ( 'NONE',  ( 5.933842156842870530, 121.5392726388429168, 0.04747900449317096760 ) ) ;
#24265 = VERTEX_POINT ( 'NONE', #31731 ) ;
#24266 = CARTESIAN_POINT ( 'NONE',  ( 4.065609891792011155, 118.4217611105734846, 0.9713962693593600761 ) ) ;
#24267 = CARTESIAN_POINT ( 'NONE',  ( 1.903258124143570429, 106.6620211890854080, 4.980168853958236497 ) ) ;
#24268 = TOROIDAL_SURFACE ( 'NONE', #41992, 5.080000000000005400, 0.5080000000000000071 ) ;
#24269 = CARTESIAN_POINT ( 'NONE',  ( 16.87828382557106721, 17.14499999999999957, 5.016499999999999737 ) ) ;
#24270 = ADVANCED_FACE ( 'NONE', ( #21284 ), #34722, .T. ) ;
#24271 = CARTESIAN_POINT ( 'NONE',  ( 0.003550357975880899172, 159.5989787797044812, -0.1776744311461874171 ) ) ;
#24272 = CIRCLE ( 'NONE', #16114, 0.2540000000000040559 ) ;
#24273 = CARTESIAN_POINT ( 'NONE',  ( 23.34154082800037244, 148.8574307740229585, 0.2355990431193898949 ) ) ;
#24274 = CARTESIAN_POINT ( 'NONE',  ( 1.650612623617701257E-15, 17.14499999999999957, 0.000000000000000000 ) ) ;
#24275 = CARTESIAN_POINT ( 'NONE',  ( 1.954897501163971985, -15.70563665752769467, 5.595021366335008572 ) ) ;
#24276 = DIRECTION ( 'NONE',  ( -5.188838149069471174E-16, 1.699382548006136313E-16, 1.000000000000000000 ) ) ;
#24277 = CARTESIAN_POINT ( 'NONE',  ( -3.151918684035726947, 30.94949030248789157, -0.3028545185056354394 ) ) ;
#24278 = CARTESIAN_POINT ( 'NONE',  ( -4.725845587753020993, 117.9582415538433651, 0.6732661676528396422 ) ) ;
#24279 = ORIENTED_EDGE ( 'NONE', *, *, #10866, .T. ) ;
#24280 = FACE_OUTER_BOUND ( 'NONE', #38867, .T. ) ;
#24281 = CARTESIAN_POINT ( 'NONE',  ( -5.844880326603659526, 118.9651452168471621, -1.254347009492448262 ) ) ;
#24282 = CARTESIAN_POINT ( 'NONE',  ( -3.169910341315210989, 118.2446163226072713, -0.8422023655252530716 ) ) ;
#24283 = CARTESIAN_POINT ( 'NONE',  ( 4.764740839480360535, 117.6706990335958665, 1.115804577579641022 ) ) ;
#24284 = DIRECTION ( 'NONE',  ( -0.9998004120163610509, -4.016384292689131511E-17, -0.01997839162482749689 ) ) ;
#24285 = CARTESIAN_POINT ( 'NONE',  ( -0.02135216056130928922, 118.1497763966934258, 1.068549427312640132 ) ) ;
#24286 = CIRCLE ( 'NONE', #3210, 3.175000000000001155 ) ;
#24287 = CARTESIAN_POINT ( 'NONE',  ( -2.707926769430928804, 11.08828375386998033, -3.745406074561137721 ) ) ;
#24288 = FACE_OUTER_BOUND ( 'NONE', #20144, .T. ) ;
#24289 = CARTESIAN_POINT ( 'NONE',  ( -4.826036362034073157, 118.5264896598256854, 0.7768203749786585233 ) ) ;
#24290 = CARTESIAN_POINT ( 'NONE',  ( 3.884801864383396808, -13.20605796264157128, 2.953397552313849150 ) ) ;
#24291 = CARTESIAN_POINT ( 'NONE',  ( 3.075034626192812759, 115.9530684888725460, -1.465612804093755273 ) ) ;
#24292 = ADVANCED_FACE ( 'NONE', ( #41544, #24280 ), #34313, .F. ) ;
#24293 = CARTESIAN_POINT ( 'NONE',  ( -3.422508068727017960, 30.97603876469775130, 4.291008727245660737 ) ) ;
#24294 = CARTESIAN_POINT ( 'NONE',  ( -0.03519895178523997636, 115.7029491485446613, 1.761499482104069703 ) ) ;
#24295 = ORIENTED_EDGE ( 'NONE', *, *, #26687, .T. ) ;
#24296 = DIRECTION ( 'NONE',  ( -0.6825627711659331132, -0.7308269722843310223, -2.299753143848214142E-16 ) ) ;
#24297 = CARTESIAN_POINT ( 'NONE',  ( 4.206901174280650579, -15.33509931759592604, 0.05204670666830889247 ) ) ;
#24298 = CARTESIAN_POINT ( 'NONE',  ( -4.147108463826234548, 118.7489093234570561, 0.8374340306925344146 ) ) ;
#24299 = CARTESIAN_POINT ( 'NONE',  ( 0.9593126492114073534, 18.43563504644844642, -0.1793159252426369810 ) ) ;
#24300 = ORIENTED_EDGE ( 'NONE', *, *, #31808, .F. ) ;
#24301 = ORIENTED_EDGE ( 'NONE', *, *, #19302, .F. ) ;
#24302 = DIRECTION ( 'NONE',  ( -0.01731298258488772612, 0.9998501190848633202, -1.788962107505314604E-16 ) ) ;
#24303 = CIRCLE ( 'NONE', #14024, 6.349999999999999645 ) ;
#24304 = CARTESIAN_POINT ( 'NONE',  ( 3.291481622401924767, 124.4927030837263118, 0.08807361928342488655 ) ) ;
#24305 =( NAMED_UNIT ( * ) SI_UNIT ( $, .STERADIAN. ) SOLID_ANGLE_UNIT ( ) );
#24306 = CARTESIAN_POINT ( 'NONE',  ( -16.77072586670524501, 146.3384789841921361, 1.111521918641044548 ) ) ;
#24307 = EDGE_CURVE ( 'NONE', #12906, #6137, #37537, .T. ) ;
#24308 = CYLINDRICAL_SURFACE ( 'NONE', #97, 3.175000000000001155 ) ;
#24309 = CARTESIAN_POINT ( 'NONE',  ( 4.537180947476667114, 118.0682806366738049, -0.6375711883657442236 ) ) ;
#24310 = CARTESIAN_POINT ( 'NONE',  ( 2.469877670440021600, 119.5064228623769225, -0.6390414609872483442 ) ) ;
#24311 = CARTESIAN_POINT ( 'NONE',  ( -1.175363150376436350, 118.2527139659984101, -0.6673024542226160261 ) ) ;
#24312 = PLANE ( 'NONE',  #7283 ) ;
#24313 = CARTESIAN_POINT ( 'NONE',  ( 4.172632738300149136, 118.2392034709942976, -0.2169253999247517106 ) ) ;
#24314 = CARTESIAN_POINT ( 'NONE',  ( 15.78585801821209422, 147.2673792861271522, -0.2768292828507332715 ) ) ;
#24315 = ORIENTED_EDGE ( 'NONE', *, *, #38480, .F. ) ;
#24316 = CARTESIAN_POINT ( 'NONE',  ( 3.187143392547471255, -14.52651900126690876, 3.212499789951002604 ) ) ;
#24317 = EDGE_CURVE ( 'NONE', #35912, #449, #16172, .T. ) ;
#24318 = CARTESIAN_POINT ( 'NONE',  ( -4.901356651777482476, 117.4105916379840266, 0.9668049386046483340 ) ) ;
#24319 = VECTOR ( 'NONE', #1804, 1000.000000000000114 ) ;
#24320 = EDGE_CURVE ( 'NONE', #13736, #35500, #36371, .T. ) ;
#24321 = CARTESIAN_POINT ( 'NONE',  ( -57.02215525308559307, 2.672977372688998710, 2.026151568886835452 ) ) ;
#24322 = CARTESIAN_POINT ( 'NONE',  ( -4.540528814728789442, -1.371322978654152092, -0.8806307088788817294 ) ) ;
#24323 = CARTESIAN_POINT ( 'NONE',  ( 10.02184412846586525, 123.2077283916686525, 1.294377628214502751 ) ) ;
#24324 = CARTESIAN_POINT ( 'NONE',  ( -2.682217617217326211, 29.83982398439445305, 2.785746292651649192 ) ) ;
#24325 = CARTESIAN_POINT ( 'NONE',  ( -1.225173952871761118, 106.6134986179334589, 4.982835752217485314 ) ) ;
#24326 = CARTESIAN_POINT ( 'NONE',  ( 4.574821423538755205, -2.080616851812391310, 0.6590154617212384824 ) ) ;
#24327 = CARTESIAN_POINT ( 'NONE',  ( 14.67688973683548781, 148.8424012017631242, 0.4203365054377474763 ) ) ;
#24328 = CARTESIAN_POINT ( 'NONE',  ( -10.94257363143063166, 56.35470871607765275, 4.428493390990959178 ) ) ;
#24329 = CARTESIAN_POINT ( 'NONE',  ( -57.27679765945803325, 1.994406527888931135, -1.325560616021183025 ) ) ;
#24330 = CARTESIAN_POINT ( 'NONE',  ( -8.734361280028741348, 117.9425031322647612, -0.7137436082343942001 ) ) ;
#24331 = APPLICATION_CONTEXT ( 'automotive_design' ) ;
#24332 = CARTESIAN_POINT ( 'NONE',  ( 0.001862839608744629605, 124.0591982226671490, -0.09322411149286709275 ) ) ;
#24333 = CARTESIAN_POINT ( 'NONE',  ( -8.313969523394650452, 67.96940778435646280, 1.270000000000003348 ) ) ;
#24334 = CARTESIAN_POINT ( 'NONE',  ( -1.156216728506892499, 106.1802426532317725, 5.165773742336502217 ) ) ;
#24335 = CARTESIAN_POINT ( 'NONE',  ( -2.958531772299361595, 50.13146620154573441, -1.329372033065077119 ) ) ;
#24336 = CARTESIAN_POINT ( 'NONE',  ( -0.3997009428961929567, 0.5197794802236572753, -8.431077252154732804 ) ) ;
#24337 = DIRECTION ( 'NONE',  ( -0.000000000000000000, -0.000000000000000000, -1.000000000000000000 ) ) ;
#24338 = CARTESIAN_POINT ( 'NONE',  ( 0.01009854879914063273, 117.2429491485453070, -0.5053730761605219612 ) ) ;
#24339 = CARTESIAN_POINT ( 'NONE',  ( 5.177913976931217910, 56.99702125087949156, -5.372099999999997877 ) ) ;
#24340 = CARTESIAN_POINT ( 'NONE',  ( 0.03040743766744064339, 116.4813942609868178, -1.521712522323421579 ) ) ;
#24341 = CARTESIAN_POINT ( 'NONE',  ( -18.50641704078269711, 154.1703991122031994, 0.1853567545699120467 ) ) ;
#24342 = ORIENTED_EDGE ( 'NONE', *, *, #30339, .F. ) ;
#24343 = CARTESIAN_POINT ( 'NONE',  ( -58.73915225836901044, 0.1638436772961188170, -1.050014585470044348E-14 ) ) ;
#24344 = VERTEX_POINT ( 'NONE', #22536 ) ;
#24345 = CARTESIAN_POINT ( 'NONE',  ( 11.66725022231030984, 17.14499999999999957, 5.016499999999999737 ) ) ;
#24346 = CARTESIAN_POINT ( 'NONE',  ( -9.163388821854908883, 124.2347608867413413, -0.1831063163140473349 ) ) ;
#24347 = CARTESIAN_POINT ( 'NONE',  ( 4.537411113424957065, -14.92057169651182846, 4.687841795668383327 ) ) ;
#24348 = CARTESIAN_POINT ( 'NONE',  ( -1.211137314531200770, 158.8088198215516229, 1.425359051240900454 ) ) ;
#24349 = PRESENTATION_LAYER_ASSIGNMENT (  '', '', ( #4650 ) ) ;
#24350 = CARTESIAN_POINT ( 'NONE',  ( 14.55782549726406927, 156.0472725025049954, -0.8788902920476676650 ) ) ;
#24351 = CARTESIAN_POINT ( 'NONE',  ( -4.151662239014343392, 13.23730288530712862, 2.070234887608822572 ) ) ;
#24352 = CARTESIAN_POINT ( 'NONE',  ( -3.269635511691731722, 159.4655167044000166, -0.2664280249078421758 ) ) ;
#24353 = ADVANCED_FACE ( 'NONE', ( #22741 ), #34329, .T. ) ;
#24354 = CARTESIAN_POINT ( 'NONE',  ( -53.62081550738785296, 9.969973585557744045, -3.871466490782108139 ) ) ;
#24355 = ORIENTED_EDGE ( 'NONE', *, *, #30339, .T. ) ;
#24356 = CARTESIAN_POINT ( 'NONE',  ( 6.059261036834406866, 57.14999999999999858, 5.016499999999999737 ) ) ;
#24357 = CARTESIAN_POINT ( 'NONE',  ( -7.333780486663274090, 155.8804291298944236, 1.515250586328038995 ) ) ;
#24358 = CARTESIAN_POINT ( 'NONE',  ( -47.84356795211461844, 19.38525671449500010, -5.197506975155170572 ) ) ;
#24359 = CARTESIAN_POINT ( 'NONE',  ( 4.252934711844570614, 157.4559852174668322, -1.675102021473321656 ) ) ;
#24360 = CARTESIAN_POINT ( 'NONE',  ( -3.034986042679861828, 117.6993298527280984, -0.7527370910433333062 ) ) ;
#24361 = CARTESIAN_POINT ( 'NONE',  ( -47.87216941255763203, 19.82042534259524658, -5.426529464407940928 ) ) ;
#24362 = CARTESIAN_POINT ( 'NONE',  ( 16.26403174311770883, 147.1082353761072454, -0.7878939306839420897 ) ) ;
#24363 = VERTEX_POINT ( 'NONE', #38965 ) ;
#24364 = CARTESIAN_POINT ( 'NONE',  ( -8.349261126152672574, 120.8878392079396065, -1.399984990019641495 ) ) ;
#24365 = CARTESIAN_POINT ( 'NONE',  ( 3.591698533489739553, -15.62560650602327961, 3.738647084555763112 ) ) ;
#24366 = CARTESIAN_POINT ( 'NONE',  ( -4.506702721058643668, 118.1222639539786456, -0.6633736078232330691 ) ) ;
#24367 = ADVANCED_FACE ( 'NONE', ( #29151 ), #12351, .T. ) ;
#24368 = CARTESIAN_POINT ( 'NONE',  ( -8.576171974424218192, 74.02775907367175989, 1.270000000000001350 ) ) ;
#24369 = CARTESIAN_POINT ( 'NONE',  ( -14.38915334913366806, 80.27078028363496287, -1.524000000000001132 ) ) ;
#24370 = CARTESIAN_POINT ( 'NONE',  ( 9.190671247345989059, 121.6705353891887995, 1.423780222299954268 ) ) ;
#24371 = DIRECTION ( 'NONE',  ( -0.8745520943968235761, 0.4849315768086558398, -5.691349986800547879E-16 ) ) ;
#24372 = CARTESIAN_POINT ( 'NONE',  ( 16.14921358636486559, 121.2501203052637493, 0.2714571880805008441 ) ) ;
#24373 = CARTESIAN_POINT ( 'NONE',  ( 4.034796628256747120, -3.593727855734754950, 7.433834689985365785 ) ) ;
#24374 = CARTESIAN_POINT ( 'NONE',  ( 15.32629999177634872, 148.0267799683202554, 0.7554886701871541543 ) ) ;
#24375 = CARTESIAN_POINT ( 'NONE',  ( -30.19451713491628198, 70.61549828015994024, 1.269999999999991802 ) ) ;
#24376 = AXIS2_PLACEMENT_3D ( 'NONE', #9307, #12704, #16091 ) ;
#24377 = DIRECTION ( 'NONE',  ( 4.017660918040594346E-17, -1.000000000000000000, -2.376309959284834438E-19 ) ) ;
#24378 = CARTESIAN_POINT ( 'NONE',  ( -3.343419727707106492, 118.1588900059306440, 0.6560610098329158202 ) ) ;
#24379 = VECTOR ( 'NONE', #39015, 1000.000000000000000 ) ;
#24380 = CARTESIAN_POINT ( 'NONE',  ( -25.70569512491730180, 74.05161654054386133, -1.524000000000005794 ) ) ;
#24381 = CARTESIAN_POINT ( 'NONE',  ( -58.37241122568488549, -0.2962816677227891882, -1.041461608706327627E-14 ) ) ;
#24382 = CARTESIAN_POINT ( 'NONE',  ( -11.70725067560583099, 118.7242475115495495, -0.1376448473428154018 ) ) ;
#24383 = B_SPLINE_CURVE_WITH_KNOTS ( 'NONE', 3,
 ( #36569, #24178, #13970, #26974, #37187, #26552, #8009, #29954, #14175, #39775, #23548, #40193, #23970, #21385, #24387, #31200, #38245, #40600, #24813, #1631, #18628, #18411, #11609, #27591, #41230, #28438, #34210, #8633, #15008, #24593, #8426, #18199, #21182, #11400, #34411, #5038, #28007, #17995, #2043, #14797, #15435, #30993, #21811, #35056, #37600, #21596, #41016, #28224, #9062, #27800, #11824, #14586, #34624, #5451, #22027, #37392 ),
 .UNSPECIFIED., .F., .F.,
 ( 4, 2, 2, 2, 2, 1, 2, 2, 2, 2, 2, 2, 1, 2, 2, 2, 2, 2, 1, 1, 2, 2, 2, 2, 1, 1, 2, 2, 2, 2, 4 ),
 ( 0.000000000000000000, 0.06249999999998684386, 0.1249999999999736877, 0.1874999999999605316, 0.2187499999999565903, 0.2343749999999545919, 0.2421874999999535372, 0.2499999999999524825, 0.3749999999999020783, 0.4374999999998734901, 0.4687499999998556155, 0.4843749999998465117, 0.4921874999998457345, 0.4960937499998452904, 0.4999999999998448463, 0.6249999999998867573, 0.6874999999999077405, 0.7187499999999182876, 0.7343749999999272804, 0.7421874999999317213, 0.7460937499999302780, 0.7499999999999289457, 0.8124999999998901989, 0.8437499999998708811, 0.8593749999998642197, 0.8671874999998637756, 0.8710937499998634426, 0.8749999999998632205, 0.9374999999999336087, 0.9687499999999668043, 1.000000000000000000 ),
 .UNSPECIFIED. ) ;
#24384 = ORIENTED_EDGE ( 'NONE', *, *, #5071, .F. ) ;
#24385 = CARTESIAN_POINT ( 'NONE',  ( -48.57236063951932437, 24.64054515024589165, -1.011057066080545894E-14 ) ) ;
#24386 = CARTESIAN_POINT ( 'NONE',  ( -7.905494947253956184, 121.9601156449555219, -0.9643286209291552780 ) ) ;
#24387 = CARTESIAN_POINT ( 'NONE',  ( -8.561575482294372819, 118.9452303826418529, 0.9294693558781963461 ) ) ;
#24388 = ORIENTED_EDGE ( 'NONE', *, *, #33723, .F. ) ;
#24389 = CARTESIAN_POINT ( 'NONE',  ( 0.5401341148544321902, 115.6909491485452719, -1.744863588967870527 ) ) ;
#24390 = CARTESIAN_POINT ( 'NONE',  ( -15.29340151118749525, 148.0176312819745874, -0.6334265850898868067 ) ) ;
#24391 = CARTESIAN_POINT ( 'NONE',  ( 3.361239686659836856, -14.56070858809799162, 5.257229516148527182 ) ) ;
#24392 = CARTESIAN_POINT ( 'NONE',  ( -1.297493386698629125, 159.2526592949493534, 1.079139715401668420 ) ) ;
#24393 = CYLINDRICAL_SURFACE ( 'NONE', #23351, 5.588000000000006295 ) ;
#24394 = CARTESIAN_POINT ( 'NONE',  ( 13.41573142586483591, 156.9389434127184018, 0.3962193537810602684 ) ) ;
#24395 = CARTESIAN_POINT ( 'NONE',  ( 11.79002894202885265, 130.2874576319956361, 0.2924100448099202776 ) ) ;
#24396 = CARTESIAN_POINT ( 'NONE',  ( -5.028626460200799286, 117.3993840973718932, 0.6246689785710292098 ) ) ;
#24397 = CARTESIAN_POINT ( 'NONE',  ( -0.6395729929254629909, 24.25746453972198680, 0.7366970655621520869 ) ) ;
#24398 = CARTESIAN_POINT ( 'NONE',  ( -16.86029543505362227, 155.2078297922403465, -0.3599557924993777580 ) ) ;
#24399 = CARTESIAN_POINT ( 'NONE',  ( -17.65389921742010060, 84.42347906515803402, -1.524000000000003352 ) ) ;
#24400 = LINE ( 'NONE', #30177, #21030 ) ;
#24401 = VERTEX_POINT ( 'NONE', #25747 ) ;
#24402 = CARTESIAN_POINT ( 'NONE',  ( 8.314316052578815786, 119.9194173129146748, 1.447167333058394512 ) ) ;
#24403 = CARTESIAN_POINT ( 'NONE',  ( 3.417104117279694098, -14.34023910220586906, -3.129441506049576383 ) ) ;
#24404 = CARTESIAN_POINT ( 'NONE',  ( 22.03343284943298030, 146.2042277794223537, 2.039575571141828192 ) ) ;
#24405 = CARTESIAN_POINT ( 'NONE',  ( -49.99157512322356922, 16.20856241626062655, -4.827055480674552257 ) ) ;
#24406 = CARTESIAN_POINT ( 'NONE',  ( 20.46656357041385377, 147.8414448467482600, -1.666390110339677655 ) ) ;
#24407 = CARTESIAN_POINT ( 'NONE',  ( 6.480130183504051011, 21.94006803110874415, 5.378050974841823262 ) ) ;
#24408 = CARTESIAN_POINT ( 'NONE',  ( -21.46783008853691754, 136.6907720476960435, -1.692068800591147060 ) ) ;
#24409 = CARTESIAN_POINT ( 'NONE',  ( 4.948841739784780813, 117.6230884628553497, -0.7513042659447916050 ) ) ;
#24410 = ORIENTED_EDGE ( 'NONE', *, *, #25627, .T. ) ;
#24411 = CARTESIAN_POINT ( 'NONE',  ( -12.04197430995787954, 130.4833683797432684, 0.05493623226408311799 ) ) ;
#24413 = CARTESIAN_POINT ( 'NONE',  ( 6.479796796485603139, -13.80134569450770776, 0.08439370571411514144 ) ) ;
#24412 = CIRCLE ( 'NONE', #42138, 8.794749999999996959 ) ;
#24414 = CARTESIAN_POINT ( 'NONE',  ( -7.842268484490568348, 73.30875693322846587, -1.523999999999996247 ) ) ;
#24415 = CARTESIAN_POINT ( 'NONE',  ( -3.743775977915335229, 109.0594729580190005, -3.805242568780236478 ) ) ;
#24416 = ORIENTED_EDGE ( 'NONE', *, *, #35498, .F. ) ;
#24417 = CARTESIAN_POINT ( 'NONE',  ( 5.836180790127331264, 119.4106843418347950, 1.193569107438471333 ) ) ;
#24418 = FACE_OUTER_BOUND ( 'NONE', #22133, .T. ) ;
#24419 = DIRECTION ( 'NONE',  ( 0.01997839162482749689, 1.040247600000945640E-18, -0.9998004120163610509 ) ) ;
#24420 = CARTESIAN_POINT ( 'NONE',  ( -0.3199181899540057272, 107.4969721965504021, 4.676354563382915330 ) ) ;
#24421 = CARTESIAN_POINT ( 'NONE',  ( 1.285294229880325600, 5.975470260049262627, -8.359553334813638159 ) ) ;
#24422 = CARTESIAN_POINT ( 'NONE',  ( 6.483461908857734102, 121.4942169270607053, 0.6390524964423263121 ) ) ;
#24423 = CARTESIAN_POINT ( 'NONE',  ( -47.85244527695896011, 19.39403540832957518, 5.219971639306693056 ) ) ;
#24424 = CARTESIAN_POINT ( 'NONE',  ( 16.66487874612757736, 155.2617138006751532, -0.3247879035468687614 ) ) ;
#24425 = CARTESIAN_POINT ( 'NONE',  ( -9.665786669610962889, 55.24499999999999034, -0.1866227975165204167 ) ) ;
#24426 = CARTESIAN_POINT ( 'NONE',  ( -57.91476036080663903, 0.6893188445402892439, 0.9676700770145346686 ) ) ;
#24427 = LINE ( 'NONE', #37432, #11910 ) ;
#24428 = CARTESIAN_POINT ( 'NONE',  ( -49.52983867584422484, 17.03535102234312859, 5.021609156700045595 ) ) ;
#24429 = DIRECTION ( 'NONE',  ( 0.01997839162482749689, 1.040247600000945640E-18, -0.9998004120163610509 ) ) ;
#24430 = CARTESIAN_POINT ( 'NONE',  ( -4.115839894752868489, 118.2429491485453354, 0.1890361656430152582 ) ) ;
#24431 = CARTESIAN_POINT ( 'NONE',  ( 3.156006274272449286, 108.3452893864970150, -4.146484234041631467 ) ) ;
#24432 = ORIENTED_EDGE ( 'NONE', *, *, #34939, .T. ) ;
#24433 = CARTESIAN_POINT ( 'NONE',  ( -47.87216941255763203, 19.82042534259524658, 5.426529464407925829 ) ) ;
#24434 = VECTOR ( 'NONE', #21041, 1000.000000000000000 ) ;
#24435 = CARTESIAN_POINT ( 'NONE',  ( -8.276141957500152913, 120.1053043740212445, -1.449957327947475338 ) ) ;
#24436 = AXIS2_PLACEMENT_3D ( 'NONE', #17278, #11303, #7496 ) ;
#24437 = FACE_OUTER_BOUND ( 'NONE', #36105, .T. ) ;
#24438 = CARTESIAN_POINT ( 'NONE',  ( 4.407114152208388980, 118.1655186915589297, 0.6432706596802734156 ) ) ;
#24439 = CARTESIAN_POINT ( 'NONE',  ( -3.646880827531788327, 120.8687762150871379, -0.3676761613455564182 ) ) ;
#24440 = CARTESIAN_POINT ( 'NONE',  ( 5.009498726350964937, 117.5220155938639977, -0.6178361814830906074 ) ) ;
#24441 = CARTESIAN_POINT ( 'NONE',  ( 1.477727405461724555E-15, 14.60500000000000220, 0.000000000000000000 ) ) ;
#24442 = EDGE_LOOP ( 'NONE', ( #13394, #28394, #12175, #37597 ) ) ;
#24443 = CARTESIAN_POINT ( 'NONE',  ( -4.420329592304260480, 21.65838872207745425, -1.398650104627336743 ) ) ;
#24444 = CARTESIAN_POINT ( 'NONE',  ( -8.539651237459656485, 154.7538831414287870, -1.439145765679522571 ) ) ;
#24445 = DIRECTION ( 'NONE',  ( -0.8745520943968235761, 0.4849315768086558398, -5.691349986800547879E-16 ) ) ;
#24446 = CARTESIAN_POINT ( 'NONE',  ( -44.00561601145927426, 21.61144970255518771, 2.814601217462325167 ) ) ;
#24447 = CARTESIAN_POINT ( 'NONE',  ( -28.60507221318229298, 76.72702915747851193, -1.524000000000007793 ) ) ;
#24448 = CARTESIAN_POINT ( 'NONE',  ( -6.065173057319897865, 121.4418940636094391, -0.09687486233282362191 ) ) ;
#24449 = CARTESIAN_POINT ( 'NONE',  ( 4.915103509140258176, 117.7039392452923323, -0.7324920538677794912 ) ) ;
#24450 = CARTESIAN_POINT ( 'NONE',  ( 22.37507221999716478, 149.9331680011685251, 1.622875787667645842 ) ) ;
#24451 = CARTESIAN_POINT ( 'NONE',  ( 5.177913976931196594, 77.01756249999996840, -5.372100000000004094 ) ) ;
#24453 = CARTESIAN_POINT ( 'NONE',  ( 0.02615207601215380553, 159.0391464308674756, -1.308756824028193266 ) ) ;
#24452 = CARTESIAN_POINT ( 'NONE',  ( 2.985050690391415795, -14.25097394772453718, 0.5935303709388186633 ) ) ;
#24454 = CARTESIAN_POINT ( 'NONE',  ( -4.149433946629451420, 157.3082466949932723, 1.660590259719063599 ) ) ;
#24455 = CARTESIAN_POINT ( 'NONE',  ( -4.295268622494708310, 18.69437521248495671, 1.722957355393906598 ) ) ;
#24456 = CARTESIAN_POINT ( 'NONE',  ( -23.06261834269087174, 146.6371693212631158, -1.324134011023372581 ) ) ;
#24457 = CARTESIAN_POINT ( 'NONE',  ( 0.9708619386763404080, 12.65153173543952470, -0.1022289352641109206 ) ) ;
#24458 = EDGE_LOOP ( 'NONE', ( #10860, #29019, #18363, #26187 ) ) ;
#24459 = CARTESIAN_POINT ( 'NONE',  ( -50.60903162571948855, 13.45680032611325849, 2.107060282091932191 ) ) ;
#24460 = CARTESIAN_POINT ( 'NONE',  ( -10.06005632938197714, 124.8772485319846055, 0.3443025955426560758 ) ) ;
#24461 = CARTESIAN_POINT ( 'NONE',  ( 5.306636623844629419, -13.66766582561489152, 3.280230747366464694 ) ) ;
#24462 = CARTESIAN_POINT ( 'NONE',  ( 11.73912714423988390, 153.3684197651487580, -1.370860710263249960 ) ) ;
#24463 = ORIENTED_EDGE ( 'NONE', *, *, #26125, .F. ) ;
#24464 = CARTESIAN_POINT ( 'NONE',  ( 1.784244551060144124, 115.7029491485453292, 1.723397082296914684 ) ) ;
#24465 = ORIENTED_EDGE ( 'NONE', *, *, #5652, .T. ) ;
#24466 = CARTESIAN_POINT ( 'NONE',  ( 3.011490660845400402, -14.57542554230247056, 4.052385860498629810 ) ) ;
#24467 = CARTESIAN_POINT ( 'NONE',  ( -4.873043952982492044, 117.7164335358027216, -0.9339496037525177874 ) ) ;
#24468 = EDGE_CURVE ( 'NONE', #35513, #1265, #21364, .T. ) ;
#24469 = CARTESIAN_POINT ( 'NONE',  ( 15.23158847265882621, 143.4365109762209158, 0.1756275167766376266 ) ) ;
#24470 = AXIS2_PLACEMENT_3D ( 'NONE', #18974, #40379, #15572 ) ;
#24471 = EDGE_LOOP ( 'NONE', ( #29949, #34702, #7925, #39474 ) ) ;
#24472 = CARTESIAN_POINT ( 'NONE',  ( -0.03153870137021896197, 158.4432089348667319, 1.578325583784928154 ) ) ;
#24473 = FACE_OUTER_BOUND ( 'NONE', #30971, .T. ) ;
#24474 = CARTESIAN_POINT ( 'NONE',  ( 0.009747742627749139341, 156.3581291470199233, -0.4878169013068171522 ) ) ;
#24475 = CARTESIAN_POINT ( 'NONE',  ( 23.27479113596625382, 149.3390083238215595, 0.2346540593346971015 ) ) ;
#24476 = CARTESIAN_POINT ( 'NONE',  ( -28.69846420587789737, 77.20784726182124302, -1.270000000000007567 ) ) ;
#24477 = CARTESIAN_POINT ( 'NONE',  ( 1.774274676131157191, -15.12224598438900713, 5.803401512178314015 ) ) ;
#24478 = CARTESIAN_POINT ( 'NONE',  ( 10.62867326514804311, 56.48194529650096740, 4.405924061720294382 ) ) ;
#24479 = CARTESIAN_POINT ( 'NONE',  ( -6.059261036834473479, 56.58343591620776181, -4.712961528314683513 ) ) ;
#24480 = CARTESIAN_POINT ( 'NONE',  ( -4.839665964887291949, 117.8306912978229377, 0.7068891268956964957 ) ) ;
#24481 = B_SPLINE_SURFACE_WITH_KNOTS ( 'NONE', 1, 3, ( 
 ( #18440, #28252, #12065, #25052, #30608, #14408, #27415, #24205, #22057, #12279, #41684, #3336 ),
 ( #15667, #29090, #35084, #5905, #2501, #15880, #16305, #150, #29306, #9712, #22678, #2713 ) ),
 .UNSPECIFIED., .F., .F., .F.,
 ( 2, 2 ),
 ( 4, 3, 2, 3, 4 ),
 ( 0.000000000000000000, 1.000000000000000000 ),
 ( -0.01867714150337349693, 0.000000000000000000, 0.5000000000000000000, 1.000000000000000000, 1.010000000000000009 ),
 .UNSPECIFIED. ) ;
#24482 = EDGE_LOOP ( 'NONE', ( #9942, #4646, #10874, #15399 ) ) ;
#24483 = ORIENTED_EDGE ( 'NONE', *, *, #7382, .T. ) ;
#24484 = CARTESIAN_POINT ( 'NONE',  ( -4.855364188028922001, 117.4053679690828602, 1.004246593774441365 ) ) ;
#24485 = CARTESIAN_POINT ( 'NONE',  ( -2.609399678953878698, 117.6784490614926426, -0.7904977363455250039 ) ) ;
#24486 = CARTESIAN_POINT ( 'NONE',  ( -4.584725329088070289, 124.7699485019152945, -0.09621079440654284332 ) ) ;
#24487 = CARTESIAN_POINT ( 'NONE',  ( 4.872669516377786003, 117.7163985243862783, 0.9341506115307878222 ) ) ;
#24488 = CARTESIAN_POINT ( 'NONE',  ( -4.707492808873059431, 117.7228541735984066, -1.103909285615471081 ) ) ;
#24489 = CARTESIAN_POINT ( 'NONE',  ( -0.2858543223548531964, 109.4728569552520554, 3.914881836256077552 ) ) ;
#24490 = CARTESIAN_POINT ( 'NONE',  ( -4.637963820743935983, -6.603494994175692412, 0.1710436084038768345 ) ) ;
#24491 = CARTESIAN_POINT ( 'NONE',  ( 4.828127062081292387, 117.4060377263907213, -1.008211717711906541 ) ) ;
#24492 = CARTESIAN_POINT ( 'NONE',  ( -4.808499656004150857, 118.5264896598256854, 0.8103638877405311414 ) ) ;
#24493 = CARTESIAN_POINT ( 'NONE',  ( 3.497624268394256219, -13.57517324819364291, 2.900746184505403669 ) ) ;
#24494 = ADVANCED_FACE ( 'NONE', ( #9775 ), #32787, .F. ) ;
#24495 = CARTESIAN_POINT ( 'NONE',  ( 5.936300781872302146, 120.8604418758245487, -0.1421746502253221078 ) ) ;
#24496 = CARTESIAN_POINT ( 'NONE',  ( -4.734860929486131909, 29.02688818834038642, 2.807733122327669140 ) ) ;
#24497 = CARTESIAN_POINT ( 'NONE',  ( -6.519774838065697039E-14, 78.83346620154574680, 1.207165459601591275E-19 ) ) ;
#24498 = CARTESIAN_POINT ( 'NONE',  ( -0.01876340930523686876, 19.73428105357427853, -4.634220987317214657 ) ) ;
#24499 = EDGE_LOOP ( 'NONE', ( #13436, #24355, #8390, #10114, #36121, #32810 ) ) ;
#24500 = CARTESIAN_POINT ( 'NONE',  ( 2.199016089875075686, -15.62526216655714428, 5.252760144517266916 ) ) ;
#24501 = CARTESIAN_POINT ( 'NONE',  ( -4.169621149806146398, 118.9132445967212419, 0.8414384147219283738 ) ) ;
#24502 = CARTESIAN_POINT ( 'NONE',  ( 0.5584349385955980072, -2.506542431320444742, 0.8015440831694167212 ) ) ;
#24503 = CARTESIAN_POINT ( 'NONE',  ( 0.9733856798199480576, 17.99895565637743999, 0.09873697238165508872 ) ) ;
#24504 = ORIENTED_EDGE ( 'NONE', *, *, #16439, .F. ) ;
#24505 = EDGE_LOOP ( 'NONE', ( #5892, #33403, #4068, #3025 ) ) ;
#24506 = DIRECTION ( 'NONE',  ( -5.188838149069471174E-16, 1.699382548006136313E-16, 1.000000000000000000 ) ) ;
#24507 = CARTESIAN_POINT ( 'NONE',  ( 3.662133038521572903, 120.6652674781340551, 0.4257566204602385995 ) ) ;
#24508 = CARTESIAN_POINT ( 'NONE',  ( -16.34996387626505765, 143.9496486471311698, 1.129508837753296691 ) ) ;
#24509 = CARTESIAN_POINT ( 'NONE',  ( -3.682264917456324671, 97.88346620154572975, -0.07358041635423967497 ) ) ;
#24510 = CARTESIAN_POINT ( 'NONE',  ( 4.605456961276924943, 118.0199559457295067, -0.6871734479863592648 ) ) ;
#24511 = CARTESIAN_POINT ( 'NONE',  ( 4.278356142283907815, 119.7015364213435333, -0.7555980432150395387 ) ) ;
#24512 = CARTESIAN_POINT ( 'NONE',  ( -12.76651978940624410, 122.1393999080170971, -1.787974849574114122 ) ) ;
#24513 = LINE ( 'NONE', #11957, #33139 ) ;
#24514 = AXIS2_PLACEMENT_3D ( 'NONE', #7926, #30697, #17910 ) ;
#24515 = ADVANCED_FACE ( 'NONE', ( #6588 ), #9563, .F. ) ;
#24516 = CARTESIAN_POINT ( 'NONE',  ( -0.02537255736359545280, 39.20946620154573026, 1.269746523260778304 ) ) ;
#24517 = CARTESIAN_POINT ( 'NONE',  ( 9.945677869404924820, 124.8826105625126530, -0.2455395418728890944 ) ) ;
#24518 = ORIENTED_EDGE ( 'NONE', *, *, #22521, .T. ) ;
#24519 = CARTESIAN_POINT ( 'NONE',  ( 2.985050690391415795, -14.25097394772453718, 0.5935303709388186633 ) ) ;
#24520 = AXIS2_PLACEMENT_3D ( 'NONE', #28579, #15574, #2614 ) ;
#24521 = CARTESIAN_POINT ( 'NONE',  ( 4.841613500239096979, 117.7629961082686805, 0.9521891642859552363 ) ) ;
#24522 = CARTESIAN_POINT ( 'NONE',  ( -55.98935619762568194, 5.304184903327291423, 2.807757416346100765 ) ) ;
#24523 = EDGE_CURVE ( 'NONE', #22644, #1116, #4670, .T. ) ;
#24524 = CARTESIAN_POINT ( 'NONE',  ( -2.488979065607898722, -9.142725400274830605, 3.900846118434742493 ) ) ;
#24525 = CARTESIAN_POINT ( 'NONE',  ( 16.29178962149223864, 143.9496486471311698, 1.781768755694405071 ) ) ;
#24526 = CARTESIAN_POINT ( 'NONE',  ( 2.383384332998917721, 36.54265742952285478, 1.181390620739962483 ) ) ;
#24527 = CARTESIAN_POINT ( 'NONE',  ( -2.376338430377652688, 108.4767889311100362, 4.155189222081930644 ) ) ;
#24528 = CARTESIAN_POINT ( 'NONE',  ( 4.634220987317881679, -1.855718946426311078, -0.01876340930339078644 ) ) ;
#24529 = CARTESIAN_POINT ( 'NONE',  ( 15.78746250177961663, 146.2429432508320417, 0.4439881280938307029 ) ) ;
#24530 = CARTESIAN_POINT ( 'NONE',  ( 8.404578209848946102, -5.696077331678487177, -0.5057995593162113446 ) ) ;
#24531 = CARTESIAN_POINT ( 'NONE',  ( -57.80191396384030611, 0.8575073823135492823, -0.7186190270693895155 ) ) ;
#24532 = CARTESIAN_POINT ( 'NONE',  ( 2.156385823092337617, 116.5621172156812264, -0.3272761531281138669 ) ) ;
#24533 = CARTESIAN_POINT ( 'NONE',  ( 0.01111760956569015496, 120.5507043431653784, -0.5563706444132521245 ) ) ;
#24534 = CARTESIAN_POINT ( 'NONE',  ( -3.174366308152013705, 104.6144662015457243, -0.06343139340882732180 ) ) ;
#24535 = CARTESIAN_POINT ( 'NONE',  ( -13.46199999999999442, 13.84300000000000530, 1.648619521012166368E-15 ) ) ;
#24536 = CARTESIAN_POINT ( 'NONE',  ( -0.02244247360070318262, 39.09286639261657115, 1.286999615499952787 ) ) ;
#24537 = AXIS2_PLACEMENT_3D ( 'NONE', #39046, #2649, #9239 ) ;
#24538 = CARTESIAN_POINT ( 'NONE',  ( -8.332721659230562850, 3.087680552427906733, 1.359589815967415127 ) ) ;
#24539 = CARTESIAN_POINT ( 'NONE',  ( 4.367111786564722209, 117.9394488565217785, 1.183296878226660853 ) ) ;
#24540 = DIRECTION ( 'NONE',  ( 5.206863593109713045E-17, -1.000000000000000000, 1.077750396879097359E-30 ) ) ;
#24541 = CARTESIAN_POINT ( 'NONE',  ( 18.35410564743290607, 77.35382415001784295, -1.904999999999999583 ) ) ;
#24542 = ADVANCED_FACE ( 'NONE', ( #30419 ), #28940, .F. ) ;
#24543 = CARTESIAN_POINT ( 'NONE',  ( 0.01635612297673702184, 119.2343925067225427, -0.8185272769044250607 ) ) ;
#24544 = CARTESIAN_POINT ( 'NONE',  ( -11.52575769572330344, 118.8226552325407397, 0.2321966025152970570 ) ) ;
#24545 = ORIENTED_EDGE ( 'NONE', *, *, #3533, .F. ) ;
#24546 = DIRECTION ( 'NONE',  ( -0.8572391118119481179, -0.5149185422762151410, 0.000000000000000000 ) ) ;
#24547 = EDGE_CURVE ( 'NONE', #11330, #21134, #38526, .T. ) ;
#24548 = ORIENTED_EDGE ( 'NONE', *, *, #26450, .F. ) ;
#24549 = DIRECTION ( 'NONE',  ( 1.011795553208986377E-16, 1.000000000000000000, -0.000000000000000000 ) ) ;
#24551 = CARTESIAN_POINT ( 'NONE',  ( -15.76285804746354380, 145.9067145067653541, -0.3149794173055767699 ) ) ;
#24550 = VECTOR ( 'NONE', #4294, 1000.000000000000000 ) ;
#24552 = CARTESIAN_POINT ( 'NONE',  ( 2.449088499779481953, -15.60605025760848719, 5.768239595176595458 ) ) ;
#24553 = CARTESIAN_POINT ( 'NONE',  ( -13.62782584980156741, 121.9345505566020194, 1.161422094953211470 ) ) ;
#24554 = EDGE_CURVE ( 'NONE', #10652, #7108, #10722, .T. ) ;
#24555 = CARTESIAN_POINT ( 'NONE',  ( 17.38882309766589174, 125.1846915036903027, -0.8043053978789252989 ) ) ;
#24556 = CARTESIAN_POINT ( 'NONE',  ( 3.465721614298269415, 18.43485028915299750, -3.064284189100199729 ) ) ;
#24557 = CARTESIAN_POINT ( 'NONE',  ( -8.196043946343930742, 117.5568930537867800, -0.4237257472399767466 ) ) ;
#24558 = CARTESIAN_POINT ( 'NONE',  ( -51.03298409374609435, 14.59756979370895991, -4.682653388026000840 ) ) ;
#24559 = VERTEX_POINT ( 'NONE', #17112 ) ;
#24560 = CARTESIAN_POINT ( 'NONE',  ( -8.797854266432963755, 117.6962148302091293, -0.06373852044383021553 ) ) ;
#24561 = DIRECTION ( 'NONE',  ( -4.017660918040594346E-17, 1.000000000000000000, 2.376309959284834438E-19 ) ) ;
#24562 = CARTESIAN_POINT ( 'NONE',  ( -17.79400844405183335, 146.5573550606970628, 1.533700293046251995 ) ) ;
#24563 = DIRECTION ( 'NONE',  ( 0.9998004120163608288, 0.000000000000000000, 0.01997839162482760791 ) ) ;
#24564 = CARTESIAN_POINT ( 'NONE',  ( 18.05326814683158787, 150.0321773811041339, -1.740468527814021060 ) ) ;
#24565 = CARTESIAN_POINT ( 'NONE',  ( -2.141138273642896550, 117.8876587302075194, -0.7126953207602169105 ) ) ;
#24566 = CARTESIAN_POINT ( 'NONE',  ( -53.83456308493991571, 9.379524109395250164, -3.755176697756441140 ) ) ;
#24567 = CARTESIAN_POINT ( 'NONE',  ( 9.727312926402424509, 123.7664141286412871, -0.5879621312111033005 ) ) ;
#24568 = ORIENTED_EDGE ( 'NONE', *, *, #1463, .T. ) ;
#24569 = CARTESIAN_POINT ( 'NONE',  ( -18.33584167903968876, 146.8095856830544790, -2.399012226062094300 ) ) ;
#24570 = CARTESIAN_POINT ( 'NONE',  ( 4.169050558263453610, -15.30144204372030359, -0.4701337638493395255 ) ) ;
#24571 = CARTESIAN_POINT ( 'NONE',  ( -4.467274181827439072, 118.1153900419622431, -0.7451687554449282214 ) ) ;
#24572 = TOROIDAL_SURFACE ( 'NONE', #1466, 6.826249999999999929, 0.6350000000000000089 ) ;
#24573 = CARTESIAN_POINT ( 'NONE',  ( -57.95878807693440393, 1.295030275130740094, -1.504629864475988787 ) ) ;
#24574 = CARTESIAN_POINT ( 'NONE',  ( 3.682264917456192777, 82.64346620154573486, 0.07358041635423968885 ) ) ;
#24575 = CARTESIAN_POINT ( 'NONE',  ( 11.43271672892777602, 123.4929228318607386, 1.641276387634013290 ) ) ;
#24576 = DIRECTION ( 'NONE',  ( 0.9998004120163608288, 0.000000000000000000, 0.01997839162482749342 ) ) ;
#24577 = AXIS2_PLACEMENT_3D ( 'NONE', #7422, #4236, #20380 ) ;
#24578 = CARTESIAN_POINT ( 'NONE',  ( 5.270772580891830650, -0.5842219557417941411, -6.616342194954959233 ) ) ;
#24579 = CARTESIAN_POINT ( 'NONE',  ( 9.304959842724178642, 124.0984330410602183, 0.5077435198050488374 ) ) ;
#24580 = CARTESIAN_POINT ( 'NONE',  ( 4.646169936107913401, 117.9325745699973282, -0.7782960047779410306 ) ) ;
#24581 = EDGE_CURVE ( 'NONE', #4948, #20977, #40139, .T. ) ;
#24583 = VERTEX_POINT ( 'NONE', #30314 ) ;
#24582 = CARTESIAN_POINT ( 'NONE',  ( -42.98746435103614516, 21.25571956186866984, -0.9029888148949808402 ) ) ;
#24584 = CARTESIAN_POINT ( 'NONE',  ( -1.974101587913926981, 118.1588900521014409, 0.7857444796409881471 ) ) ;
#24585 = AXIS2_PLACEMENT_3D ( 'NONE', #35837, #6858, #9626 ) ;
#24586 = CARTESIAN_POINT ( 'NONE',  ( -7.844413229920568220, 122.2807544141772524, -0.7395612626406528056 ) ) ;
#24587 = CARTESIAN_POINT ( 'NONE',  ( -58.37241122568488549, -0.2962816677227891882, -1.042239624154175981E-14 ) ) ;
#24588 = CARTESIAN_POINT ( 'NONE',  ( -50.10414895690885828, 20.83497401302349061, 1.621381026025490613 ) ) ;
#24589 = CARTESIAN_POINT ( 'NONE',  ( -11.68775717287302740, 118.7263634577040676, -0.08842886322950098410 ) ) ;
#24590 = ORIENTED_EDGE ( 'NONE', *, *, #9982, .T. ) ;
#24591 = CARTESIAN_POINT ( 'NONE',  ( -50.73416975447392474, 21.22185706673585059, -0.7846160747445178885 ) ) ;
#24592 = CARTESIAN_POINT ( 'NONE',  ( -7.863154760065894422, 122.1805646130430745, -0.8209280068902528038 ) ) ;
#24593 = CARTESIAN_POINT ( 'NONE',  ( -8.131384943450896685, 121.0503350093196815, 0.9968526362124168205 ) ) ;
#24594 = ORIENTED_EDGE ( 'NONE', *, *, #17569, .F. ) ;
#24595 = CARTESIAN_POINT ( 'NONE',  ( 1.413592544884475721, 118.7629491485454025, -1.196437990151151709 ) ) ;
#24596 = CARTESIAN_POINT ( 'NONE',  ( -9.348637138742866171, 124.2740283646700306, -0.4211050520620435722 ) ) ;
#24597 = CARTESIAN_POINT ( 'NONE',  ( 2.834973442847717351, -15.21714937722351557, 5.773325752997570781 ) ) ;
#24598 = VECTOR ( 'NONE', #24652, 1000.000000000000000 ) ;
#24599 = CARTESIAN_POINT ( 'NONE',  ( -20.59913821282573565, 136.3738900553462372, 1.239205967624167792 ) ) ;
#24600 = DIRECTION ( 'NONE',  ( -5.188838149069471174E-16, 1.699382548006136313E-16, 1.000000000000000000 ) ) ;
#24601 = AXIS2_PLACEMENT_3D ( 'NONE', #23065, #19882, #39500 ) ;
#24602 = CARTESIAN_POINT ( 'NONE',  ( 1.824897337458711855, 116.5125207362610951, 0.1392185346034943982 ) ) ;
#24603 = EDGE_CURVE ( 'NONE', #35748, #6398, #8380, .T. ) ;
#24604 = CARTESIAN_POINT ( 'NONE',  ( 11.83539255247743149, 152.0195595274622349, 0.2364993098673506822 ) ) ;
#24605 = FACE_OUTER_BOUND ( 'NONE', #41772, .T. ) ;
#24606 = CARTESIAN_POINT ( 'NONE',  ( -0.9370761106581132482, 23.39645565634240043, 0.2812775048015344614 ) ) ;
#24607 = CARTESIAN_POINT ( 'NONE',  ( -14.83769995734848202, 120.3134675335783754, -0.3991467459773893056 ) ) ;
#24608 = CARTESIAN_POINT ( 'NONE',  ( -47.36402078847329733, 19.94680556959678697, -5.177108626122005397 ) ) ;
#24609 = ADVANCED_FACE ( 'NONE', ( #30113 ), #13684, .T. ) ;
#24610 = VERTEX_POINT ( 'NONE', #10417 ) ;
#24611 = CARTESIAN_POINT ( 'NONE',  ( 3.194789458502170110, 117.5549192558606251, 0.8028907591355466389 ) ) ;
#24612 = CARTESIAN_POINT ( 'NONE',  ( -24.49496359545907609, 76.94162913054094588, -1.270000000000005569 ) ) ;
#24613 = CARTESIAN_POINT ( 'NONE',  ( 17.48314440517386359, 153.9260871938423065, 1.866247694559708403 ) ) ;
#24614 = CARTESIAN_POINT ( 'NONE',  ( -58.45640570440971828, -0.4407481023139133147, -0.3169051027093325312 ) ) ;
#24615 = CARTESIAN_POINT ( 'NONE',  ( 8.948346978250095063, 119.7003323559047061, -1.088312767383050605 ) ) ;
#24616 = CARTESIAN_POINT ( 'NONE',  ( 7.043328640077428204, 23.89357186360551566, -4.653114003055315528 ) ) ;
#24617 = CARTESIAN_POINT ( 'NONE',  ( -1.305078825605850312, 159.4185946040361728, -0.8784184817623136299 ) ) ;
#24618 = CARTESIAN_POINT ( 'NONE',  ( 4.775642591496352729, 117.6653311871567382, -0.9390539395389304600 ) ) ;
#24619 = CARTESIAN_POINT ( 'NONE',  ( 0.1506203121292604419, 105.8833743670705445, 5.338473058816376238 ) ) ;
#24620 = ORIENTED_EDGE ( 'NONE', *, *, #29465, .F. ) ;
#24621 = CARTESIAN_POINT ( 'NONE',  ( -11.25890738108754263, 128.1602342495223468, 0.05278459517150006775 ) ) ;
#24622 = CARTESIAN_POINT ( 'NONE',  ( -13.39306239354274197, 123.7870877700634509, -1.917211633051635333 ) ) ;
#24623 = AXIS2_PLACEMENT_3D ( 'NONE', #34572, #15377, #18146 ) ;
#24624 = CARTESIAN_POINT ( 'NONE',  ( 4.954452526664399059, -15.13560178954495505, 4.019779494548574306 ) ) ;
#24625 = DIRECTION ( 'NONE',  ( 9.627370216492862708E-17, 1.000000000000000000, -0.000000000000000000 ) ) ;
#24626 = CARTESIAN_POINT ( 'NONE',  ( -3.960243126016221193, 117.9496055611373748, -1.231645824533994960 ) ) ;
#24627 = ORIENTED_EDGE ( 'NONE', *, *, #38665, .F. ) ;
#24628 = CARTESIAN_POINT ( 'NONE',  ( 10.36135117696309571, 155.6679353847891321, 2.160796112024522486 ) ) ;
#24629 = CARTESIAN_POINT ( 'NONE',  ( -17.14500000000466784, 71.11999999999886768, 1.269999999999998241 ) ) ;
#24630 = CARTESIAN_POINT ( 'NONE',  ( -5.319749943626951527, 115.6909491485453003, 0.5104040631377158022 ) ) ;
#24631 = VECTOR ( 'NONE', #15114, 1000.000000000000227 ) ;
#24632 = CARTESIAN_POINT ( 'NONE',  ( -2.311559032574000749, 118.7862729053988318, 0.6846880608948529012 ) ) ;
#24633 = CARTESIAN_POINT ( 'NONE',  ( -4.887076909682236625, -2.444604220856811505, -6.895871986673536291 ) ) ;
#24634 = CARTESIAN_POINT ( 'NONE',  ( 4.540840819607053547, 155.9125706774115940, 0.9348598387858672032 ) ) ;
#24635 = DIRECTION ( 'NONE',  ( 5.188838149069472160E-16, -1.699382548006136559E-16, -1.000000000000000000 ) ) ;
#24636 = CARTESIAN_POINT ( 'NONE',  ( 21.54968253652544519, 151.3526640061693342, -0.5241015958777708317 ) ) ;
#24637 = CARTESIAN_POINT ( 'NONE',  ( -23.34387769576312621, 77.71194901948682343, -1.524000000000005128 ) ) ;
#24638 = CARTESIAN_POINT ( 'NONE',  ( -58.07466396318727675, 0.3426375511560262321, 0.7560645715230442931 ) ) ;
#24639 = CARTESIAN_POINT ( 'NONE',  ( -4.469853575504566301, 31.48943071249222214, -0.6923489671027511783 ) ) ;
#24640 = FACE_OUTER_BOUND ( 'NONE', #21562, .T. ) ;
#24641 = CARTESIAN_POINT ( 'NONE',  ( -4.303542067741650712, 118.2142174830580359, 0.3397717045260155166 ) ) ;
#24642 = AXIS2_PLACEMENT_3D ( 'NONE', #7997, #11384, #37173 ) ;
#24643 = FACE_OUTER_BOUND ( 'NONE', #36074, .T. ) ;
#24644 = ORIENTED_EDGE ( 'NONE', *, *, #5173, .F. ) ;
#24645 = CARTESIAN_POINT ( 'NONE',  ( -47.43570116002442205, 20.37060963802031566, 5.342502768866032703 ) ) ;
#24646 = ADVANCED_FACE ( 'NONE', ( #29807 ), #39829, .T. ) ;
#24647 = CARTESIAN_POINT ( 'NONE',  ( -4.295590839325457821, 119.4259349426024386, -0.9270884132243183418 ) ) ;
#24648 = CARTESIAN_POINT ( 'NONE',  ( -5.306918775014303868, 116.0444662015457169, 1.063204892635948307 ) ) ;
#24649 = CARTESIAN_POINT ( 'NONE',  ( 4.266316740665818230, 118.2131443819900198, 0.5314761920156354513 ) ) ;
#24650 = CARTESIAN_POINT ( 'NONE',  ( -13.85976170726116585, 150.2454140652271803, -1.103110692033625995 ) ) ;
#24651 = FACE_OUTER_BOUND ( 'NONE', #18080, .T. ) ;
#24652 = DIRECTION ( 'NONE',  ( -1.000000000000000000, -6.353134868986659519E-16, 0.000000000000000000 ) ) ;
#24653 = ADVANCED_FACE ( 'NONE', ( #40040 ), #29140, .T. ) ;
#24654 = ORIENTED_EDGE ( 'NONE', *, *, #2459, .T. ) ;
#24655 = CARTESIAN_POINT ( 'NONE',  ( -0.6244342276652131707, 19.93415720681881353, -4.586363120317934694 ) ) ;
#24656 = CARTESIAN_POINT ( 'NONE',  ( -29.36430674031901944, 68.35616281593667054, 1.523999999999992472 ) ) ;
#24657 = DIRECTION ( 'NONE',  ( 5.188838149069472160E-16, -1.699382548006136559E-16, -1.000000000000000000 ) ) ;
#24658 = CARTESIAN_POINT ( 'NONE',  ( -42.47169588413780161, 21.98427696618763960, 1.915014136675358580 ) ) ;
#24659 = DIRECTION ( 'NONE',  ( 0.6559537821943239866, -0.7548010569845283735, 4.686333752532408853E-16 ) ) ;
#24660 = CARTESIAN_POINT ( 'NONE',  ( -6.063368700931957456, 121.4421655836107163, -0.07279211641118281395 ) ) ;
#24661 = CARTESIAN_POINT ( 'NONE',  ( -4.596079559025361583, 18.26954911218466648, 0.4757704999388879807 ) ) ;
#24662 = CARTESIAN_POINT ( 'NONE',  ( 4.831157780893915010, 117.2114307359545649, 0.6331281246675558583 ) ) ;
#24663 = DIRECTION ( 'NONE',  ( -4.017660918040594346E-17, 1.000000000000000000, 2.376309959284834438E-19 ) ) ;
#24665 = CARTESIAN_POINT ( 'NONE',  ( 0.4156903444692294225, 117.7785671674745771, -0.5149838300002415048 ) ) ;
#24664 = CARTESIAN_POINT ( 'NONE',  ( 2.931439949929583122, -14.82325452411255640, 4.117531814738872420 ) ) ;
#24666 = CARTESIAN_POINT ( 'NONE',  ( -14.54156464587795661, 128.5519869857110393, 1.481139062272948337 ) ) ;
#24667 = CARTESIAN_POINT ( 'NONE',  ( 2.233585966345281282, 24.54162662436292308, -4.064490141941544898 ) ) ;
#24668 = CARTESIAN_POINT ( 'NONE',  ( -20.39753840605640178, 152.5480347002736607, -1.233721349276552637 ) ) ;
#24669 = AXIS2_PLACEMENT_3D ( 'NONE', #38764, #20348, #4204 ) ;
#24670 = CARTESIAN_POINT ( 'NONE',  ( 0.6786060095046909657, 20.86726683125115756, 0.6988831909418605770 ) ) ;
#24671 = ORIENTED_EDGE ( 'NONE', *, *, #41569, .F. ) ;
#24672 = CARTESIAN_POINT ( 'NONE',  ( -57.27679765945803325, 1.994406527888931135, 1.325560616021162597 ) ) ;
#24673 = CARTESIAN_POINT ( 'NONE',  ( -15.60301224545410825, 143.6313904367523833, 0.5515178422673751024 ) ) ;
#24674 = CARTESIAN_POINT ( 'NONE',  ( 2.652408316642993480, -15.27006336626107696, 5.836003982494253783 ) ) ;
#24675 = CARTESIAN_POINT ( 'NONE',  ( 17.21539028065161148, 147.4900653055648547, -1.363477025422524802 ) ) ;
#24676 = ORIENTED_EDGE ( 'NONE', *, *, #15903, .F. ) ;
#24677 = CARTESIAN_POINT ( 'NONE',  ( 0.8957990821136506687, 115.7029491485453150, 1.751259771659311237 ) ) ;
#24678 = CIRCLE ( 'NONE', #6331, 3.111499999999999932 ) ;
#24679 = EDGE_LOOP ( 'NONE', ( #14184, #20361, #6778, #25520 ) ) ;
#24680 = CARTESIAN_POINT ( 'NONE',  ( 3.301452709780442252, -13.00349394711965090, 1.536261971075179478 ) ) ;
#24681 = CARTESIAN_POINT ( 'NONE',  ( -4.734399331529842492, 117.8958854344520262, -0.9305720750720559709 ) ) ;
#24682 = CARTESIAN_POINT ( 'NONE',  ( 11.85733017202526440, 130.3381101163291760, 0.1934038552275229028 ) ) ;
#24683 = AXIS2_PLACEMENT_3D ( 'NONE', #13804, #6634, #36817 ) ;
#24684 = VERTEX_POINT ( 'NONE', #1944 ) ;
#24685 = CARTESIAN_POINT ( 'NONE',  ( 12.98660267081546138, 122.0079276396459704, 1.762897954238471954 ) ) ;
#24686 = CARTESIAN_POINT ( 'NONE',  ( -5.177913976931285411, 57.14999999999998437, 5.372100000000002318 ) ) ;
#24687 = CARTESIAN_POINT ( 'NONE',  ( -9.909999474182706436, 76.95545850745379823, 1.524000000000001576 ) ) ;
#24688 = CARTESIAN_POINT ( 'NONE',  ( 0.02969037535068572500, 158.7301711276701894, -1.485827791648137053 ) ) ;
#24689 = CARTESIAN_POINT ( 'NONE',  ( 23.39020171064277065, 146.7932648766621639, 0.1331748977937668443 ) ) ;
#24690 = CARTESIAN_POINT ( 'NONE',  ( -23.43300365160792964, 82.12916405548841681, -1.270000000000006013 ) ) ;
#24691 = PRESENTATION_LAYER_ASSIGNMENT (  '', '', ( #17219 ) ) ;
#24692 = VECTOR ( 'NONE', #3259, 1000.000000000000000 ) ;
#24693 = CARTESIAN_POINT ( 'NONE',  ( 1.924448629921342357, -15.15080081298969539, 5.916077864091418448 ) ) ;
#24694 = DIRECTION ( 'NONE',  ( 0.9998004120163609398, 4.016384292689130894E-17, 0.01997839162482749689 ) ) ;
#24695 = CARTESIAN_POINT ( 'NONE',  ( -7.921807157844599878, 72.80702234259206307, -1.269999999999996021 ) ) ;
#24696 = CARTESIAN_POINT ( 'NONE',  ( -4.811373471701494431, 117.8747111989650875, 0.6665432265399071632 ) ) ;
#24697 = VERTEX_POINT ( 'NONE', #21920 ) ;
#24698 = ORIENTED_EDGE ( 'NONE', *, *, #29088, .F. ) ;
#24699 = LINE ( 'NONE', #8528, #13884 ) ;
#24700 = CARTESIAN_POINT ( 'NONE',  ( 5.810495312042946559, 118.7618932863102401, -1.004714121124453241 ) ) ;
#24701 = CARTESIAN_POINT ( 'NONE',  ( -3.839037681459759987, 115.3331674797404247, -1.733041430519539183 ) ) ;
#24702 = CARTESIAN_POINT ( 'NONE',  ( 4.916126448754050138, 117.5420021306158418, 1.049297650600119258 ) ) ;
#24703 = DIRECTION ( 'NONE',  ( -5.188838149069472160E-16, 1.699382548006136559E-16, 1.000000000000000000 ) ) ;
#24704 = CARTESIAN_POINT ( 'NONE',  ( -1.052442600544543749, 124.5996987749017109, 0.008430925479885411494 ) ) ;
#24705 = AXIS2_PLACEMENT_3D ( 'NONE', #38847, #39270, #22416 ) ;
#24706 = CARTESIAN_POINT ( 'NONE',  ( -0.2095918955067871126, -8.989892990265463624, -4.636818132431064221 ) ) ;
#24707 = DIRECTION ( 'NONE',  ( 9.627370216492862708E-17, 1.000000000000000000, -0.000000000000000000 ) ) ;
#24708 = CARTESIAN_POINT ( 'NONE',  ( -14.81953868692883702, 57.78499999999998948, 0.4987879908248463168 ) ) ;
#24709 = CARTESIAN_POINT ( 'NONE',  ( 2.175557056806384448, -14.94057515128023539, 5.440454282391695706 ) ) ;
#24710 = CARTESIAN_POINT ( 'NONE',  ( 4.883585300477370161, 117.2937442104795593, -0.7242188414070881430 ) ) ;
#24711 = ADVANCED_FACE ( 'NONE', ( #14903 ), #18306, .T. ) ;
#24712 = DIRECTION ( 'NONE',  ( -1.000000000000000000, 0.000000000000000000, 0.000000000000000000 ) ) ;
#24713 = CARTESIAN_POINT ( 'NONE',  ( -38.65395868481546415, 29.38327706004843876, -1.270000000000004903 ) ) ;
#24714 = CARTESIAN_POINT ( 'NONE',  ( -1.749991611943370051, 115.7029018373826545, 1.658182375568262312 ) ) ;
#24715 = CARTESIAN_POINT ( 'NONE',  ( 2.267534764145236803, 6.115564135048844108, 4.037922524061999141 ) ) ;
#24717 = ORIENTED_EDGE ( 'NONE', *, *, #41947, .F. ) ;
#24716 = CARTESIAN_POINT ( 'NONE',  ( 22.69296959717475559, 150.3666470947781022, 1.044501570340798713 ) ) ;
#24718 = CARTESIAN_POINT ( 'NONE',  ( -0.1040029800483648487, 104.6144662015455964, -4.835167297233627259 ) ) ;
#24719 = CARTESIAN_POINT ( 'NONE',  ( 2.909835405328949687, -15.65209430229147536, 4.668939894544173796 ) ) ;
#24720 = CARTESIAN_POINT ( 'NONE',  ( -8.613587046216272469, 156.7723266660784986, 1.729508645372233255 ) ) ;
#24721 = CARTESIAN_POINT ( 'NONE',  ( -0.4796499176084361160, 15.67505972103439049, -0.8497018901732851237 ) ) ;
#24722 = CARTESIAN_POINT ( 'NONE',  ( -0.4212773433310383342, 21.23346528477927819, -0.8800754956890687319 ) ) ;
#24723 = ORIENTED_EDGE ( 'NONE', *, *, #38040, .T. ) ;
#24724 = MANIFOLD_SOLID_BREP ( 'Stock-MAS-162-1', #27830 ) ;
#24725 = ORIENTED_EDGE ( 'NONE', *, *, #24776, .T. ) ;
#24726 = CARTESIAN_POINT ( 'NONE',  ( 1.400628584307200167E-15, 13.84300000000000352, 0.000000000000000000 ) ) ;
#24727 = CARTESIAN_POINT ( 'NONE',  ( 1.549819036667637873, 118.0223913815010377, 1.039293717761402558 ) ) ;
#24728 = FILL_AREA_STYLE_COLOUR ( '', #1931 ) ;
#24729 = CARTESIAN_POINT ( 'NONE',  ( -2.625396581831559661, 120.2926465633240127, 0.4415429531236471083 ) ) ;
#24730 = CARTESIAN_POINT ( 'NONE',  ( -41.28107547821694112, 23.22158991241130011, 1.523999999999988475 ) ) ;
#24731 = CARTESIAN_POINT ( 'NONE',  ( 1.889397806843069905, -15.09730794468430659, 5.542604807410119072 ) ) ;
#24732 = CARTESIAN_POINT ( 'NONE',  ( 16.17691485933963946, 135.1141785778430346, -1.596016904437364659 ) ) ;
#24733 = VECTOR ( 'NONE', #3310, 1000.000000000000114 ) ;
#24734 = CARTESIAN_POINT ( 'NONE',  ( -20.36154792711273842, 148.1475078817917961, -2.480623434655589765 ) ) ;
#24735 = FACE_OUTER_BOUND ( 'NONE', #20868, .T. ) ;
#24736 = CARTESIAN_POINT ( 'NONE',  ( -1.386537629721184883, 36.36735770096321829, 2.585368322340787284 ) ) ;
#24737 = CARTESIAN_POINT ( 'NONE',  ( 8.684730043605602745, 123.3259068333282755, -0.1300027459630655191 ) ) ;
#24738 = ORIENTED_EDGE ( 'NONE', *, *, #24238, .F. ) ;
#24739 = CARTESIAN_POINT ( 'NONE',  ( 2.971193505762239617, -14.05637172046637851, 0.8995351626913862253 ) ) ;
#24740 = CARTESIAN_POINT ( 'NONE',  ( -3.958300029084214522, 28.23836431654049761, 1.224951011016432556 ) ) ;
#24741 = AXIS2_PLACEMENT_3D ( 'NONE', #34096, #36876, #30253 ) ;
#24742 = CARTESIAN_POINT ( 'NONE',  ( -58.45128286774038884, -0.4309378487369980304, 0.3205346425638702090 ) ) ;
#24743 = CARTESIAN_POINT ( 'NONE',  ( -3.029891238501105644, -9.367638731076009861, 3.490193963561483148 ) ) ;
#24744 = CARTESIAN_POINT ( 'NONE',  ( 6.507413728077992232, 121.1369950346570192, 0.8796459533030992484 ) ) ;
#24745 = CARTESIAN_POINT ( 'NONE',  ( -2.854324211611072304, 29.11572452856798776, 0.7926346486988061768 ) ) ;
#24746 = CARTESIAN_POINT ( 'NONE',  ( -6.089625701343511111, 119.5347744825833871, 0.2725575997743532874 ) ) ;
#24747 = AXIS2_PLACEMENT_3D ( 'NONE', #1782, #4982, #27332 ) ;
#24748 = AXIS2_PLACEMENT_3D ( 'NONE', #6567, #25524, #38524 ) ;
#24749 = CARTESIAN_POINT ( 'NONE',  ( -4.399545650080316506, 2.442302885307133131, -1.471791394725967095 ) ) ;
#24750 = CARTESIAN_POINT ( 'NONE',  ( 11.03183784343224616, 128.0124916018596650, 0.2204423744267036411 ) ) ;
#24751 = ADVANCED_FACE ( 'NONE', ( #35779 ), #31308, .T. ) ;
#24752 = CARTESIAN_POINT ( 'NONE',  ( 6.742867120194277142, -6.769607736128188336, 5.057590804256700601 ) ) ;
#24753 = CARTESIAN_POINT ( 'NONE',  ( -57.65203525413342334, 1.118929822212927361, -0.5921937322712454987 ) ) ;
#24754 = CARTESIAN_POINT ( 'NONE',  ( -2.144839993658618216, 116.4227009531578858, -0.3427478915012472371 ) ) ;
#24755 = CARTESIAN_POINT ( 'NONE',  ( 0.06282972276528790700, 111.5577547982949227, -3.144256248693278355 ) ) ;
#24756 = AXIS2_PLACEMENT_3D ( 'NONE', #34943, #25129, #30890 ) ;
#24757 = CARTESIAN_POINT ( 'NONE',  ( -2.958531772299362039, 50.42904571186020490, -1.329372033065077341 ) ) ;
#24758 = CARTESIAN_POINT ( 'NONE',  ( -7.483757832938788823, -7.479835662595867518, -3.861840502031824940 ) ) ;
#24759 = CARTESIAN_POINT ( 'NONE',  ( 0.3864482072712463467, 117.9394481662412062, 1.409681420816396580 ) ) ;
#24760 = CARTESIAN_POINT ( 'NONE',  ( -29.91139568370675761, 83.95719535527389610, 1.523999999999989807 ) ) ;
#24761 = CARTESIAN_POINT ( 'NONE',  ( -58.83227707057486811, -0.08366279997995551554, -1.533110566128066119E-14 ) ) ;
#24762 = ADVANCED_FACE ( 'NONE', ( #33010 ), #16155, .F. ) ;
#24763 = CARTESIAN_POINT ( 'NONE',  ( 0.9884870862448961182, 123.5966405200008325, -0.1018174175105950180 ) ) ;
#24764 = CARTESIAN_POINT ( 'NONE',  ( -2.843964318557778981, 116.7549172960530939, 0.2381273168889447012 ) ) ;
#24765 = ORIENTED_EDGE ( 'NONE', *, *, #10530, .F. ) ;
#24766 = CARTESIAN_POINT ( 'NONE',  ( -58.35673254475433680, 1.205555466438051893, -0.1480423017862652624 ) ) ;
#24767 = VERTEX_POINT ( 'NONE', #3838 ) ;
#24768 = CARTESIAN_POINT ( 'NONE',  ( -47.84356795211438396, 19.38525671449516352, -5.197506975155015141 ) ) ;
#24769 = CARTESIAN_POINT ( 'NONE',  ( -15.64207015331068185, 147.2204672151589193, -0.3125657877211906466 ) ) ;
#24770 = CARTESIAN_POINT ( 'NONE',  ( 6.422280156622033331, -13.89829431882434818, 0.3667318345078443564 ) ) ;
#24771 = CARTESIAN_POINT ( 'NONE',  ( -14.84487292597024499, 154.6636077862465015, 1.582666667450879805 ) ) ;
#24772 = CARTESIAN_POINT ( 'NONE',  ( 16.02745508617892867, 155.1095016151506911, -1.019363059911538638 ) ) ;
#24773 = CARTESIAN_POINT ( 'NONE',  ( -4.598301960400187127, 22.30806413504685537, 0.5496829067130363233 ) ) ;
#24774 = CARTESIAN_POINT ( 'NONE',  ( -16.76609992697674301, 155.2615993841311877, -0.7433399007605485664 ) ) ;
#24775 = CARTESIAN_POINT ( 'NONE',  ( -48.65109498377578490, 18.34191667582345175, -5.169736723450931493 ) ) ;
#24776 = EDGE_CURVE ( 'NONE', #40395, #25154, #29476, .T. ) ;
#24777 = ORIENTED_EDGE ( 'NONE', *, *, #22679, .F. ) ;
#24778 = CARTESIAN_POINT ( 'NONE',  ( -2.183037072706512483, 116.1872911837574947, -0.04021945895725198561 ) ) ;
#24779 = CYLINDRICAL_SURFACE ( 'NONE', #14790, 3.175000000000001155 ) ;
#24780 = CARTESIAN_POINT ( 'NONE',  ( -11.33340168069295650, 123.5700555580090594, 1.145074488444943528 ) ) ;
#24781 = CARTESIAN_POINT ( 'NONE',  ( -56.28088753042789705, 4.173514606889340506, -2.292216047950881297 ) ) ;
#24782 = CARTESIAN_POINT ( 'NONE',  ( 19.06441997122210452, 145.0145856610025987, -1.755053680361626345 ) ) ;
#24783 = CARTESIAN_POINT ( 'NONE',  ( -14.96081243412116990, 123.1914926142276130, -1.724312424550131562 ) ) ;
#24784 = CARTESIAN_POINT ( 'NONE',  ( -51.73272837791831336, 13.19950324185369794, -4.393710239503588078 ) ) ;
#24785 = CARTESIAN_POINT ( 'NONE',  ( 16.31827467517370422, 146.7930872653447523, -0.7884962901916309219 ) ) ;
#24786 = EDGE_CURVE ( 'NONE', #3481, #18999, #39060, .T. ) ;
#24787 = EDGE_LOOP ( 'NONE', ( #25421, #27210, #34696, #32747 ) ) ;
#24788 = CARTESIAN_POINT ( 'NONE',  ( -5.440231158483335605, 156.5946142756450570, -1.801097700867929419 ) ) ;
#24789 = CARTESIAN_POINT ( 'NONE',  ( 3.946041497568072653, -15.66665589675640646, 3.498282510246776500 ) ) ;
#24790 = CARTESIAN_POINT ( 'NONE',  ( -4.105086577347437427, 118.2429491485453070, -0.3532857226942683893 ) ) ;
#24791 = ADVANCED_FACE ( 'NONE', ( #27029 ), #10832, .T. ) ;
#24792 = CARTESIAN_POINT ( 'NONE',  ( -57.92346726745822849, 0.7446056814934959300, -1.206286704679871535 ) ) ;
#24793 = MANIFOLD_SOLID_BREP ( 'Stock-MAS-162-1', #38728 ) ;
#24794 = CARTESIAN_POINT ( 'NONE',  ( -29.81357423954495189, 70.62209452652477637, 1.523999999999992250 ) ) ;
#24795 = CARTESIAN_POINT ( 'NONE',  ( 7.267393677827311826, 155.8804291298944236, 1.807016794997827747 ) ) ;
#24796 = DIRECTION ( 'NONE',  ( -0.8745520943968249084, 0.4849315768086536194, -5.575199987069925217E-16 ) ) ;
#24797 =( BOUNDED_CURVE ( )  B_SPLINE_CURVE ( 3, ( #11871, #40852, #21642, #24639 ),
 .UNSPECIFIED., .F., .T. ) 
 B_SPLINE_CURVE_WITH_KNOTS ( ( 4, 4 ),
 ( 0.0002600131435865652915, 0.01144530851284875084 ),
 .UNSPECIFIED. ) 
 CURVE ( )  GEOMETRIC_REPRESENTATION_ITEM ( )  RATIONAL_B_SPLINE_CURVE ( ( 0.9989604882768124972, 0.9840622721794859418, 0.9694976849687608755, 0.9552667266446374095 ) ) 
 REPRESENTATION_ITEM ( '' )  );
#24798 = EDGE_CURVE ( 'NONE', #31688, #9144, #39006, .T. ) ;
#24799 = CARTESIAN_POINT ( 'NONE',  ( 0.6763034141103227981, -4.228338640871131204, 8.424193199533098309 ) ) ;
#24800 = CARTESIAN_POINT ( 'NONE',  ( 9.106360905785095383, 123.9337093609977529, 0.4112724569044294842 ) ) ;
#24801 = CARTESIAN_POINT ( 'NONE',  ( 4.801298557440690118, 117.4006788788929896, -1.015947269269607656 ) ) ;
#24802 = B_SPLINE_CURVE_WITH_KNOTS ( 'NONE', 3,
 ( #1674, #1044, #37228, #36610, #7638, #10606 ),
 .UNSPECIFIED., .F., .F.,
 ( 4, 2, 4 ),
 ( 0.000000000000000000, 0.0001552906547695077498, 0.0003105813095390154996 ),
 .UNSPECIFIED. ) ;
#24804 = ORIENTED_EDGE ( 'NONE', *, *, #6574, .T. ) ;
#24803 = CARTESIAN_POINT ( 'NONE',  ( -43.08902205111511563, 20.96483665317663991, -0.2987222196696421861 ) ) ;
#24805 = CARTESIAN_POINT ( 'NONE',  ( -16.62722885652246418, 62.94807988814252298, 4.514343177587269551 ) ) ;
#24806 = CARTESIAN_POINT ( 'NONE',  ( -7.805875142760556606, 122.5029850928241615, -0.4967190073759077951 ) ) ;
#24807 = DIRECTION ( 'NONE',  ( -0.8745520943968246863, 0.4849315768086537859, -5.361993529360573944E-16 ) ) ;
#24808 = CARTESIAN_POINT ( 'NONE',  ( -51.58376292578905975, 16.21309621351152330, 3.606096628736468634 ) ) ;
#24809 = CARTESIAN_POINT ( 'NONE',  ( -10.80084657379841495, 157.9251727141802633, -0.03745751586626412666 ) ) ;
#24810 = ORIENTED_EDGE ( 'NONE', *, *, #39334, .T. ) ;
#24811 = CARTESIAN_POINT ( 'NONE',  ( -47.69778088985397346, 22.45332703829874887, -3.190613414150612837 ) ) ;
#24812 = CARTESIAN_POINT ( 'NONE',  ( -6.854099372262661305, 121.6001605170599618, -0.7074379530687137096 ) ) ;
#24813 = CARTESIAN_POINT ( 'NONE',  ( -8.378245210821358313, 119.8566484287661353, 1.107698278211572740 ) ) ;
#24814 = VERTEX_POINT ( 'NONE', #31470 ) ;
#24815 = CARTESIAN_POINT ( 'NONE',  ( 0.4316031730808821409, 115.7034384546826686, -1.748259241455569546 ) ) ;
#24816 = CARTESIAN_POINT ( 'NONE',  ( -1.593749994916005885, 120.9451058151398399, -0.1271097986196581264 ) ) ;
#24817 = CARTESIAN_POINT ( 'NONE',  ( 4.653081906828674619, -14.28787889440780212, 4.403751634497075074 ) ) ;
#24818 = CARTESIAN_POINT ( 'NONE',  ( -9.329873057606407727, 118.8811571165754941, 0.8296725728930307575 ) ) ;
#24819 = CARTESIAN_POINT ( 'NONE',  ( 10.28897677580358305, 56.51500000000000057, -4.381500000000000838 ) ) ;
#24820 = CARTESIAN_POINT ( 'NONE',  ( -0.001640166039863760056, 159.6041700698465036, 0.08208061555506501739 ) ) ;
#24821 = CARTESIAN_POINT ( 'NONE',  ( 15.72247783716871083, 145.6852940966224708, 0.3814333285848034438 ) ) ;
#24822 = CARTESIAN_POINT ( 'NONE',  ( -17.64290547347870941, 83.78857423953914463, -1.270000000000003126 ) ) ;
#24823 = CARTESIAN_POINT ( 'NONE',  ( 0.9754839647580387796, 27.70931421350951496, 0.02445524045744520980 ) ) ;
#24824 = CARTESIAN_POINT ( 'NONE',  ( -21.64466742782801845, 132.7051459832101443, -0.4972030839502442068 ) ) ;
#24825 = CARTESIAN_POINT ( 'NONE',  ( -6.426369768295692736E-14, 159.6054662015457382, 1.032716915552223178E-16 ) ) ;
#24826 = CARTESIAN_POINT ( 'NONE',  ( 1.167505706004672243E-15, 11.53894877578617084, 0.000000000000000000 ) ) ;
#24827 = VERTEX_POINT ( 'NONE', #12302 ) ;
#24828 = AXIS2_PLACEMENT_3D ( 'NONE', #35995, #9993, #22336 ) ;
#24829 = CARTESIAN_POINT ( 'NONE',  ( -5.745771690987640845, 118.0751039679726659, 0.8607859349433016893 ) ) ;
#24830 = CARTESIAN_POINT ( 'NONE',  ( 4.543739712435177047, -15.19060223592207137, -0.8445694877862246486 ) ) ;
#24831 = CARTESIAN_POINT ( 'NONE',  ( 5.844042411599751574, 117.9059190437751141, 0.9510131463654533102 ) ) ;
#24832 = CARTESIAN_POINT ( 'NONE',  ( -48.43799250123969102, 18.62746361536592943, -5.176101822179832723 ) ) ;
#24833 = CARTESIAN_POINT ( 'NONE',  ( 13.21705611421139359, 122.1656469061080514, -1.250183119358982742 ) ) ;
#24834 = CARTESIAN_POINT ( 'NONE',  ( 2.538140519494355374, 21.06397054095828381, 8.048466014368985455 ) ) ;
#24835 = CARTESIAN_POINT ( 'NONE',  ( -15.93415399606969096, 122.8751182158008959, -1.397711951582541801 ) ) ;
#24836 = CARTESIAN_POINT ( 'NONE',  ( 4.783731562129573511, 117.6342719419094323, -0.9515537801535082219 ) ) ;
#24837 = CARTESIAN_POINT ( 'NONE',  ( 5.263686092533300886, 116.7134249176580028, 1.019678336081760506 ) ) ;
#24838 = ORIENTED_EDGE ( 'NONE', *, *, #26384, .T. ) ;
#24839 = EDGE_CURVE ( 'NONE', #31005, #5931, #18252, .T. ) ;
#24840 = CARTESIAN_POINT ( 'NONE',  ( -9.614588335866276481, 124.8310256250372277, -0.1039111448415539068 ) ) ;
#24841 = CARTESIAN_POINT ( 'NONE',  ( -12.24350972434462115, 123.0735437985678971, -1.806721486477698368 ) ) ;
#24842 = CARTESIAN_POINT ( 'NONE',  ( 4.975685353906630581, -15.32372399918348371, 3.685287151418908724 ) ) ;
#24843 = CARTESIAN_POINT ( 'NONE',  ( 13.51778232847667205, 17.08230797367789222, -5.016499999999999737 ) ) ;
#24844 = B_SPLINE_CURVE_WITH_KNOTS ( 'NONE', 3,
 ( #34951, #21495, #15326, #25136, #37712, #11505, #2368, #18518, #8535, #37496, #31108, #14904, #15543, #38140, #5354, #18307, #27907, #8954, #12361, #21085, #8321, #30898 ),
 .UNSPECIFIED., .F., .F.,
 ( 4, 1, 1, 1, 1, 1, 1, 1, 1, 1, 1, 1, 1, 1, 1, 1, 1, 1, 1, 4 ),
 ( 0.000000000000000000, 0.02298233349012935092, 0.04596466698025848674, 0.05745583372532304250, 0.06894700047038783419, 0.08043816721545261894, 0.09192933396051740369, 0.1034205007055817443, 0.1149116674506463071, 0.1838586679210341135, 0.2298233349012926141, 0.3217526688618093655, 0.3333333333333334259, 0.4136820028223265333, 0.5056113367828434235, 0.5975406707433602582, 0.6435053377236188421, 0.6664876712137480785, 0.6894700047038772039, 0.7354344192538687652 ),
 .UNSPECIFIED. ) ;
#24845 = CARTESIAN_POINT ( 'NONE',  ( -1.067625512720145942, 118.1651004991311851, -0.8760196487506567431 ) ) ;
#24846 = ORIENTED_EDGE ( 'NONE', *, *, #19130, .T. ) ;
#24847 = B_SPLINE_SURFACE_WITH_KNOTS ( 'NONE', 5, 5, ( 
 ( #17229, #1064, #14031, #24037, #27036, #37052 ),
 ( #28496, #34900, #24448, #11457, #34686, #9124 ),
 ( #5515, #8908, #24660, #21874, #27655, #37452 ),
 ( #38093, #22085, #18056, #18473, #5105, #2323 ),
 ( #24879, #5732, #37669, #18261, #18685, #37876 ),
 ( #27864, #31478, #38303, #31060, #31694, #40666 ),
 ( #21661, #1898, #41295, #35112, #40872, #11890 ),
 ( #15498, #2537, #14860, #8276, #8698, #41506 ),
 ( #12312, #25300, #5938, #21246, #34276, #15283 ),
 ( #30851, #28287, #1695, #8492, #14651, #11673 ),
 ( #21449, #34478, #12098, #5311, #31265, #25086 ),
 ( #2107, #15071, #28071, #41082, #9947, #36165 ),
 ( #23128, #41925, #35951, #32752, #10157, #18898 ),
 ( #42137, #28705, #6551, #25715, #29337, #16116 ),
 ( #15910, #35739, #22499, #15700, #9742, #22710 ),
 ( #19318, #2744, #178, #29119, #9328, #19526 ),
 ( #12933, #3586, #35527, #9530, #31907, #32533 ),
 ( #6348, #32323, #41714, #12520, #26348, #13358 ),
 ( #6763, #32115, #3152, #6143, #38511, #3364 ),
 ( #19108, #39142, #13148, #2946, #28910, #25511 ),
 ( #22290, #22920, #391, #19731, #16331, #35315 ),
 ( #25923, #12726, #26141, #38721, #38931, #16547 ),
 ( #29557, #39354, #23771, #27404, #39788, #29966 ),
 ( #29764, #40414, #33600, #33809, #601, #13574 ),
 ( #17391, #26563, #10583, #40208, #24194, #23985 ),
 ( #806, #37004, #20785, #11210, #6982, #20574 ),
 ( #16757, #36794, #13782, #30381, #4219, #1233 ),
 ( #7612, #23561, #3796, #40000, #10791, #36583 ),
 ( #32971, #14190, #17180, #39570, #4433, #19953 ),
 ( #4637, #7399, #20362, #10375, #27194, #17594 ),
 ( #33385, #23344, #36383, #14396, #1435, #26778 ),
 ( #7199, #20157, #33181, #4009, #11006, #16966 ),
 ( #30179, #1020, #13984, #26989, #7823, #30597 ),
 ( #20996, #40617, #34226, #25040, #37618, #8651 ),
 ( #41245, #15240, #8442, #21825, #21400, #2276 ),
 ( #40825, #11416, #31434, #21612, #11624, #24402 ),
 ( #5055, #34854, #38043, #34428, #5686, #18644 ),
 ( #37408, #5467, #15452, #18011, #18214, #28454 ),
 ( #8863, #8227, #30799, #31215, #31650, #2490 ),
 ( #41460, #12050, #21200, #5261, #31008, #14603 ),
 ( #27608, #1850, #28241, #12267, #14814, #27816 ),
 ( #17802, #2059, #34021, #24611, #15023, #37204 ),
 ( #34639, #28023, #8025, #4846, #41033, #1648 ),
 ( #11842, #24829, #37824, #18426, #19482, #38885 ),
 ( #28660, #6099, #22248, #22873, #13100, #25674 ),
 ( #35911, #2698, #29290, #35480, #16286, #26091 ),
 ( #35274, #19061, #9487, #19688, #41672, #6720 ),
 ( #9078, #32068, #39098, #2904, #25256, #12890 ),
 ( #12684, #19275, #38681, #22663, #32491, #42095 ),
 ( #15867, #28873, #25474, #3319, #25878, #15656 ),
 ( #35696, #9901, #22452, #38470, #29076, #133 ),
 ( #6303, #32705, #32283, #9288, #3112, #6507 ),
 ( #3539, #41886, #9696, #35072, #16072, #16500 ),
 ( #29507, #346, #38261, #22043, #5893, #18854 ),
 ( #12480, #31859, #19905, #20110, #23723, #16709 ),
 ( #7563, #13313, #29712, #39523, #33132, #23297 ),
 ( #10949, #10742, #39948, #26937, #972, #36741 ),
 ( #7775, #23507, #7353, #13737, #20523, #33553 ),
 ( #33763, #3962, #36334, #13529, #4385, #13939 ),
 ( #20738, #17343, #14142, #26731, #26516, #17131 ),
 ( #16923, #10327, #761, #40157, #20312, #7150 ),
 ( #4588, #17547, #30332, #36534, #23086, #1179 ),
 ( #27145, #10538, #23937, #29923, #30133, #39739 ),
 ( #4169, #36954, #33339, #30548, #39308, #26299 ),
 ( #10115, #36120, #6934, #554, #32920, #3751 ),
 ( #14764, #41195, #40985, #27975, #14974, #31170 ),
 ( #11161, #37992, #11574, #15187, #27353, #8816 ),
 ( #40366, #34591, #1387, #27766, #40777, #5003 ),
 ( #24560, #21775, #24146, #8391, #37155, #4798 ),
 ( #31384, #1803, #11787, #37564, #5420, #21563 ),
 ( #28190, #21353, #8600, #18375, #17962, #17749 ),
 ( #2226, #34379, #5213, #40572, #18167, #34801 ),
 ( #11999, #7977, #24778, #2011, #30749, #37775 ),
 ( #11369, #24992, #5635, #18593, #14343, #1599 ) ),
 .UNSPECIFIED., .F., .F., .F.,
 ( 6, 4, 4, 4, 4, 4, 4, 4, 4, 4, 4, 4, 4, 4, 4, 4, 4, 4, 6 ),
 ( 6, 6 ),
 ( 0.000000000000000000, 0.01562500000000000000, 0.03125000000000000000, 0.06250000000000000000, 0.1250000000000000000, 0.2500000000000000000, 0.3750000000000000000, 0.4375000000000000000, 0.5000000000000000000, 0.5625000000000000000, 0.6250000000000000000, 0.7500000000000000000, 0.8125000000000000000, 0.8750000000000000000, 0.9062500000000000000, 0.9375000000000000000, 0.9687500000000000000, 0.9843750000000000000, 1.000000000000000000 ),
 ( 0.000000000000000000, 1.000000000000000000 ),
 .UNSPECIFIED. ) ;
#24848 = CARTESIAN_POINT ( 'NONE',  ( 18.91839881582108518, 147.5601278813269914, 2.482394308196493871 ) ) ;
#24849 = CARTESIAN_POINT ( 'NONE',  ( -30.15642192025596202, 71.36377005712995469, -1.270000000000007345 ) ) ;
#24850 = EDGE_CURVE ( 'NONE', #929, #10361, #34013, .T. ) ;
#24851 = CARTESIAN_POINT ( 'NONE',  ( -1.914222150921244481, 118.1238929887923632, -0.9376219136777126373 ) ) ;
#24852 = CARTESIAN_POINT ( 'NONE',  ( -0.6988325576871788902, 114.3327162918516962, 2.155465965906840253 ) ) ;
#24853 = EDGE_CURVE ( 'NONE', #9260, #18326, #12090, .T. ) ;
#24854 = CARTESIAN_POINT ( 'NONE',  ( -5.887876509958990923, -9.367530720701759961, 6.022233148990229878 ) ) ;
#24855 = CARTESIAN_POINT ( 'NONE',  ( 3.128511139047426060, 156.1781389015385457, 0.8559903927114133060 ) ) ;
#24856 = CARTESIAN_POINT ( 'NONE',  ( -46.68395179480138779, 26.03198510454123848, -1.524000000000008459 ) ) ;
#24857 = AXIS2_PLACEMENT_3D ( 'NONE', #31262, #34683, #15280 ) ;
#24858 = CARTESIAN_POINT ( 'NONE',  ( 13.10540794497621597, 156.9444350391594014, -0.5617278846626184707 ) ) ;
#24859 = CARTESIAN_POINT ( 'NONE',  ( 5.449044798800651179, 56.51500000000380197, -5.145813327034902684 ) ) ;
#24860 = CARTESIAN_POINT ( 'NONE',  ( -58.09361251268546766, 0.3016395514430970093, 0.7289802440182748811 ) ) ;
#24861 = CARTESIAN_POINT ( 'NONE',  ( -29.18709815850009903, 67.04824513552235032, -1.524000000000005794 ) ) ;
#24862 = DIRECTION ( 'NONE',  ( 0.7770581983690837413, -0.6294287539884032556, 5.101669463485834765E-16 ) ) ;
#24863 = CARTESIAN_POINT ( 'NONE',  ( -4.269227857241942203, 118.2238376706496439, 0.2888421812383961118 ) ) ;
#24864 = CARTESIAN_POINT ( 'NONE',  ( 4.797736281515663670, 114.9758604107369138, -1.576599161239440772 ) ) ;
#24865 = ORIENTED_EDGE ( 'NONE', *, *, #39968, .T. ) ;
#24866 = CARTESIAN_POINT ( 'NONE',  ( -50.15972161391664486, 17.13814111569220699, 4.955022299345067438 ) ) ;
#24867 = CARTESIAN_POINT ( 'NONE',  ( 6.307464644398110387, 119.8761965894848771, -0.9734222780920257501 ) ) ;
#24868 = CARTESIAN_POINT ( 'NONE',  ( -0.1561264326628848120, 116.0444662015457027, 6.158975241439932802 ) ) ;
#24869 = CARTESIAN_POINT ( 'NONE',  ( 4.246284764148858137, 118.2248568323353481, 0.4675053700615026120 ) ) ;
#24870 = CARTESIAN_POINT ( 'NONE',  ( -8.892178686620095363, 123.2307073318660855, -0.7481024605839378117 ) ) ;
#24871 = DIRECTION ( 'NONE',  ( -0.8745520943968235761, 0.4849315768086558398, -5.691349986800547879E-16 ) ) ;
#24872 = CARTESIAN_POINT ( 'NONE',  ( 0.2348404565736222915, 117.9496055676323749, -1.400524049365383439 ) ) ;
#24873 = ORIENTED_EDGE ( 'NONE', *, *, #6991, .T. ) ;
#24874 = CARTESIAN_POINT ( 'NONE',  ( 1.790774717077139089, 25.13178105314743860, 4.274281468382033822 ) ) ;
#24875 = CARTESIAN_POINT ( 'NONE',  ( -31.80708539065861373, 53.04900798524919736, 1.269999999999994467 ) ) ;
#24876 = CYLINDRICAL_SURFACE ( 'NONE', #36456, 0.6350000000000006750 ) ;
#24877 = CARTESIAN_POINT ( 'NONE',  ( -7.772068811996249771, 69.25462295839062676, 1.270000000000003570 ) ) ;
#24878 = CARTESIAN_POINT ( 'NONE',  ( -47.87705743256026381, 19.40768263586563691, 5.264533221178260725 ) ) ;
#24879 = CARTESIAN_POINT ( 'NONE',  ( -7.788904331612559240, 122.6147083454303726, -0.08148215068823494445 ) ) ;
#24880 = CARTESIAN_POINT ( 'NONE',  ( 1.653223041919489544, 21.06826514481450729, 4.324967054831568625 ) ) ;
#24881 = CARTESIAN_POINT ( 'NONE',  ( 7.741078003750540226, 158.6130819278358501, 0.9685178112996220001 ) ) ;
#24882 = CARTESIAN_POINT ( 'NONE',  ( -3.260048740554739588, 104.6144662015456674, -3.571460647889730389 ) ) ;
#24884 = CARTESIAN_POINT ( 'NONE',  ( 9.191685830660368595, 119.1751624949753534, -0.9473905404949717335 ) ) ;
#24883 = CARTESIAN_POINT ( 'NONE',  ( 2.755019269514601632, -14.09852029293599784, -0.1464032776252038315 ) ) ;
#24885 = CARTESIAN_POINT ( 'NONE',  ( -18.09605103972953799, 148.5173242358814321, 1.660853775707743507 ) ) ;
#24886 = CARTESIAN_POINT ( 'NONE',  ( 3.707542801486926276, 23.89195667223011910, -2.776928957275885068 ) ) ;
#24887 = CARTESIAN_POINT ( 'NONE',  ( -14.96245403159076837, 120.9606250904355704, -1.059951836595168118 ) ) ;
#24888 = CARTESIAN_POINT ( 'NONE',  ( -0.08600706866453224075, 15.02498995931601122, -0.9728917428382349852 ) ) ;
#24889 = ORIENTED_EDGE ( 'NONE', *, *, #2710, .T. ) ;
#24890 = CARTESIAN_POINT ( 'NONE',  ( -56.90438685736649660, 2.765855619508456265, 1.561774844827657605 ) ) ;
#24891 = CARTESIAN_POINT ( 'NONE',  ( -9.339416610757488968, 123.9819092696984910, 0.2335442159362874082 ) ) ;
#24892 = CARTESIAN_POINT ( 'NONE',  ( 4.653081906828674619, -14.28787889440780212, 4.403751634497075074 ) ) ;
#24893 = CARTESIAN_POINT ( 'NONE',  ( 15.52878352361680214, 139.6011575924185877, -1.142358493343923920 ) ) ;
#24894 = VERTEX_POINT ( 'NONE', #41073 ) ;
#24895 = CARTESIAN_POINT ( 'NONE',  ( 0.6068092274946489395, 115.7030931646781511, 1.759830564766369232 ) ) ;
#24896 = ORIENTED_EDGE ( 'NONE', *, *, #42049, .T. ) ;
#24897 = CARTESIAN_POINT ( 'NONE',  ( -4.811659653300878858, 117.7644762915747378, -1.004442067184477594 ) ) ;
#24898 = CARTESIAN_POINT ( 'NONE',  ( 6.500720044509773921, 121.7799842514348541, 0.1008652220075046541 ) ) ;
#24899 = EDGE_LOOP ( 'NONE', ( #15594, #32674, #14197, #8124 ) ) ;
#24900 = CARTESIAN_POINT ( 'NONE',  ( 12.64856329662753076, 122.0451665396574725, 1.778165442619766834 ) ) ;
#24901 = DIRECTION ( 'NONE',  ( -0.4849315768086425726, -0.8745520943968309036, -1.030032898892908012E-16 ) ) ;
#24902 = PLANE ( 'NONE',  #28634 ) ;
#24903 = EDGE_CURVE ( 'NONE', #29093, #9109, #38333, .T. ) ;
#24904 = CARTESIAN_POINT ( 'NONE',  ( 0.01887972822138463125, 159.3676309965788960, -0.9448188026860500077 ) ) ;
#24905 = CARTESIAN_POINT ( 'NONE',  ( 6.916478980584438219, 117.2343425291504104, -0.1085122952249094053 ) ) ;
#24906 = CARTESIAN_POINT ( 'NONE',  ( 6.059261036834406866, 57.14999999999999858, -5.016499999999999737 ) ) ;
#24907 = CARTESIAN_POINT ( 'NONE',  ( 1.668644623944747662, -15.26291410520330771, 5.716625384245738850 ) ) ;
#24908 = CARTESIAN_POINT ( 'NONE',  ( 10.28897677580357950, 57.14999999999999858, 5.016499999999999737 ) ) ;
#24909 = CARTESIAN_POINT ( 'NONE',  ( -14.91798719394653538, 12.51401280605346145, 2.024102502787695046E-15 ) ) ;
#24910 = AXIS2_PLACEMENT_3D ( 'NONE', #21448, #8697, #41081 ) ;
#24911 = CARTESIAN_POINT ( 'NONE',  ( -4.732672620930323149, 117.8972391386454319, 0.7793045165695084986 ) ) ;
#24912 = VECTOR ( 'NONE', #12661, 1000.000000000000000 ) ;
#24913 = ORIENTED_EDGE ( 'NONE', *, *, #41725, .F. ) ;
#24914 = ORIENTED_EDGE ( 'NONE', *, *, #26749, .F. ) ;
#24915 = DIRECTION ( 'NONE',  ( 0.6559537821943240976, -0.7548010569845284845, 4.686333752532409839E-16 ) ) ;
#24916 = AXIS2_PLACEMENT_3D ( 'NONE', #4719, #34718, #31509 ) ;
#24917 = CARTESIAN_POINT ( 'NONE',  ( 8.556114498411417912, 118.9718870934816692, -0.9297341161968202261 ) ) ;
#24918 = CARTESIAN_POINT ( 'NONE',  ( -3.975629016402025151, 111.5999093057820772, -3.028662833142258037 ) ) ;
#24919 = CARTESIAN_POINT ( 'NONE',  ( 4.956589549431869912, 117.4692179202435938, 0.9991419478834157042 ) ) ;
#24920 = CARTESIAN_POINT ( 'NONE',  ( 6.475684456959278634, -13.49251406434824574, 0.1304084665236045215 ) ) ;
#24921 = CARTESIAN_POINT ( 'NONE',  ( -0.9126123168629748372, 122.5862318000603182, 0.2067773319678724020 ) ) ;
#24922 = CARTESIAN_POINT ( 'NONE',  ( -1.825063964020108065, -4.879331645356781877, 4.256838567046823840 ) ) ;
#24923 = CARTESIAN_POINT ( 'NONE',  ( -4.855072294470597072, 115.7029491485453718, 1.279409886141102071 ) ) ;
#24924 = LINE ( 'NONE', #5562, #32157 ) ;
#24925 = CARTESIAN_POINT ( 'NONE',  ( 2.715028358135622266, -14.64271907847003362, 5.065740987199049528 ) ) ;
#24926 = CARTESIAN_POINT ( 'NONE',  ( 6.983131083342589029, 124.7321584522365896, 0.1385298619991069402 ) ) ;
#24927 = CARTESIAN_POINT ( 'NONE',  ( -17.31991401741520775, 147.8988302317391117, -2.155506138210265821 ) ) ;
#24928 = CARTESIAN_POINT ( 'NONE',  ( 5.155022408837186987, 116.8361691014224277, 0.02608676839127775648 ) ) ;
#24929 = DIRECTION ( 'NONE',  ( -5.188838149069472160E-16, 1.699382548006136559E-16, 1.000000000000000000 ) ) ;
#24930 = CARTESIAN_POINT ( 'NONE',  ( -1.835695816207170594, 115.7029480714724627, 1.651914411509646241 ) ) ;
#24931 = CARTESIAN_POINT ( 'NONE',  ( 3.263621351691376571, 8.939281053574255509, -3.290156819607050753 ) ) ;
#24933 = ORIENTED_EDGE ( 'NONE', *, *, #13629, .F. ) ;
#24932 = CARTESIAN_POINT ( 'NONE',  ( 15.04006788896544222, 156.1474796653986630, 0.8176042244810640680 ) ) ;
#24934 = CARTESIAN_POINT ( 'NONE',  ( -1.150111429288084519, 105.1233927192594564, -5.219387141699733057 ) ) ;
#24935 = CARTESIAN_POINT ( 'NONE',  ( 4.184971198371238543, -15.30562903706386635, -0.2021278847381603183 ) ) ;
#24936 = CARTESIAN_POINT ( 'NONE',  ( -16.79779972313721359, 131.5287050380659082, 1.642352026799754672 ) ) ;
#24937 = CARTESIAN_POINT ( 'NONE',  ( 0.8610934044332675397, -11.37225059697985863, 0.4573394443077089533 ) ) ;
#24938 = CARTESIAN_POINT ( 'NONE',  ( 0.05241920358452190065, 15.83596528477922405, 0.9742995972537078497 ) ) ;
#24939 = ORIENTED_EDGE ( 'NONE', *, *, #39977, .T. ) ;
#24940 = VERTEX_POINT ( 'NONE', #8267 ) ;
#24941 = DIRECTION ( 'NONE',  ( -5.188838149069471174E-16, 1.699382548006136313E-16, 1.000000000000000000 ) ) ;
#24942 = CARTESIAN_POINT ( 'NONE',  ( 1.569662112149277977, 118.6366899268033279, 0.8670489899392762601 ) ) ;
#24943 = CARTESIAN_POINT ( 'NONE',  ( -14.29925251870378489, 150.3563008155378213, 0.9573768768026652554 ) ) ;
#24944 = DIRECTION ( 'NONE',  ( -5.206863593109713661E-17, 1.000000000000000000, -1.077750396879097183E-30 ) ) ;
#24945 = CARTESIAN_POINT ( 'NONE',  ( 3.456814872816273088, -13.76118077623555891, 3.223863823609153023 ) ) ;
#24946 = CARTESIAN_POINT ( 'NONE',  ( 0.02969003158472209580, 157.1787724364823760, -1.485810588193620330 ) ) ;
#24947 = AXIS2_PLACEMENT_3D ( 'NONE', #23364, #36398, #20174 ) ;
#24948 = CARTESIAN_POINT ( 'NONE',  ( -1.195985117830571820, 118.4063602595805946, -0.6806364119286731906 ) ) ;
#24949 = CARTESIAN_POINT ( 'NONE',  ( 4.646169936107913401, 117.9325745699973282, -0.7782960047779410306 ) ) ;
#24950 = CARTESIAN_POINT ( 'NONE',  ( -5.309060684617390516E-14, 83.56599999999998829, 0.000000000000000000 ) ) ;
#24951 = CARTESIAN_POINT ( 'NONE',  ( -5.922169694189452827, 31.30785624307803872, 2.619824438689082768 ) ) ;
#24952 = CARTESIAN_POINT ( 'NONE',  ( 15.86984883002227242, 146.9522167609303267, -0.2762592943789937694 ) ) ;
#24953 = AXIS2_PLACEMENT_3D ( 'NONE', #13911, #10710, #20077 ) ;
#24954 = ORIENTED_EDGE ( 'NONE', *, *, #7451, .F. ) ;
#24955 = CARTESIAN_POINT ( 'NONE',  ( 2.755344442395651683, -14.11966664619605716, -0.1083093155031689958 ) ) ;
#24956 = DIRECTION ( 'NONE',  ( -0.9998004120163608288, -4.016384292689131511E-17, -0.01997839162482749342 ) ) ;
#24957 = CARTESIAN_POINT ( 'NONE',  ( -14.94465077092626970, 61.74681991364688827, 5.072843609925764774 ) ) ;
#24958 = CARTESIAN_POINT ( 'NONE',  ( -58.21232023750257412, 0.08677210334570391315, 0.8315773506257112535 ) ) ;
#24959 = CARTESIAN_POINT ( 'NONE',  ( -1.404924415901314561, -12.60368214249519703, -4.422195601339041993 ) ) ;
#24960 = CARTESIAN_POINT ( 'NONE',  ( 16.68619938060333396, 146.1290494286844819, 1.780952809221992394 ) ) ;
#24961 = DIRECTION ( 'NONE',  ( -0.9998004120163608288, 0.000000000000000000, -0.01997839162482749342 ) ) ;
#24962 = CARTESIAN_POINT ( 'NONE',  ( -5.597156320496795345, 117.9391977826196296, 0.5238424959023465499 ) ) ;
#24963 = CIRCLE ( 'NONE', #23618, 0.2539999999999981162 ) ;
#24964 = CARTESIAN_POINT ( 'NONE',  ( 3.345514242732226418, 6.565394131763864216, 3.211428121085859733 ) ) ;
#24965 = CARTESIAN_POINT ( 'NONE',  ( 15.72550100231850223, 145.6881679641610674, 0.3142329346387552902 ) ) ;
#24966 = CARTESIAN_POINT ( 'NONE',  ( -6.970347610136101046, -0.07026165769430378627, 4.770677917868129114 ) ) ;
#24967 = CARTESIAN_POINT ( 'NONE',  ( -57.29531047346088712, 2.067549486662559222, -1.749273462387502809 ) ) ;
#24968 = CARTESIAN_POINT ( 'NONE',  ( -2.143470464290757604, 116.4405123390714891, -0.3531553464187269786 ) ) ;
#24969 = AXIS2_PLACEMENT_3D ( 'NONE', #26114, #16520, #6118 ) ;
#24970 = CARTESIAN_POINT ( 'NONE',  ( 0.02887436318418984751, 106.7790779034713324, -4.972892908546473478 ) ) ;
#24971 = CARTESIAN_POINT ( 'NONE',  ( -6.059261036834082681, 78.87450423423038615, -5.016499999999999737 ) ) ;
#24972 = CARTESIAN_POINT ( 'NONE',  ( -0.02537255736359465483, 39.20946620154573736, 1.269746523260778082 ) ) ;
#24973 = CARTESIAN_POINT ( 'NONE',  ( 8.141433899912401628, -11.15112405914982219, -2.164028758433363286 ) ) ;
#24974 = CARTESIAN_POINT ( 'NONE',  ( 4.378691870267736874, 117.3993836135368980, 1.268072117453972636 ) ) ;
#24975 = DIRECTION ( 'NONE',  ( 5.188838149069472160E-16, -1.699382548006136559E-16, -1.000000000000000000 ) ) ;
#24976 = DIRECTION ( 'NONE',  ( 0.9998004120163609398, 0.000000000000000000, 0.01997839162482749689 ) ) ;
#24977 = CARTESIAN_POINT ( 'NONE',  ( 0.8881552493050030028, 122.2453746293775652, -0.2465857446897831984 ) ) ;
#24978 = CARTESIAN_POINT ( 'NONE',  ( -23.13757068712599718, 148.9583646262859133, 0.2674444443938936988 ) ) ;
#24979 = VECTOR ( 'NONE', #7281, 1000.000000000000000 ) ;
#24980 = VERTEX_POINT ( 'NONE', #31685 ) ;
#24981 = CARTESIAN_POINT ( 'NONE',  ( -58.03428750496623678, 2.144022121626051991, -0.09394692876221440170 ) ) ;
#24982 = ORIENTED_EDGE ( 'NONE', *, *, #31794, .F. ) ;
#24983 = CARTESIAN_POINT ( 'NONE',  ( -42.22422426686775765, 22.06987237837593696, -1.558155077124144583 ) ) ;
#24984 = CARTESIAN_POINT ( 'NONE',  ( -6.513455546617618275, 121.7797256742974383, -0.05434986243196536504 ) ) ;
#24985 = CARTESIAN_POINT ( 'NONE',  ( 6.296695397805594396, -14.23921929796089003, 0.5540845800015932188 ) ) ;
#24986 = CARTESIAN_POINT ( 'NONE',  ( -3.150705211532708994, 118.1710492231644736, 0.7255832847742740288 ) ) ;
#24987 = CARTESIAN_POINT ( 'NONE',  ( 22.39365319421748168, 148.6363688457942942, -0.9991490326925096532 ) ) ;
#24988 = CARTESIAN_POINT ( 'NONE',  ( -0.01876340930523686876, 19.73428105357427853, -4.634220987317214657 ) ) ;
#24989 = CARTESIAN_POINT ( 'NONE',  ( -22.90211176506270974, 150.1344166263168347, -0.9094179090926686193 ) ) ;
#24990 = CARTESIAN_POINT ( 'NONE',  ( -58.43714447420092739, 0.1158066806379677849, -0.8009346905749505918 ) ) ;
#24991 = EDGE_LOOP ( 'NONE', ( #41884, #17546, #12377, #36434 ) ) ;
#24992 = CARTESIAN_POINT ( 'NONE',  ( -5.562407735369756523, 116.6996333467660634, -0.1111501472963731668 ) ) ;
#24993 = LINE ( 'NONE', #15188, #40675 ) ;
#24994 = CARTESIAN_POINT ( 'NONE',  ( -10.78650420462579618, 154.3566586077636487, 1.536168652981084515 ) ) ;
#24995 = CARTESIAN_POINT ( 'NONE',  ( -53.68617469749651860, 9.442005736215490330, -3.589663193476668290 ) ) ;
#24996 = CARTESIAN_POINT ( 'NONE',  ( 15.49426794143295893, 128.5596447653542498, -1.561415741013213898 ) ) ;
#24997 = CARTESIAN_POINT ( 'NONE',  ( -5.844153588741496819, 118.3130479344264501, -1.074361049658993705 ) ) ;
#24998 = CARTESIAN_POINT ( 'NONE',  ( -49.56090548067184898, 17.87959676410238430, -5.165259844110624776 ) ) ;
#24999 = AXIS2_PLACEMENT_3D ( 'NONE', #2439, #25423, #5214 ) ;
#25000 = CARTESIAN_POINT ( 'NONE',  ( 11.19133892028634136, 126.1638007343821641, -0.6664143115430058995 ) ) ;
#25001 = ORIENTED_EDGE ( 'NONE', *, *, #23149, .T. ) ;
#25002 = CARTESIAN_POINT ( 'NONE',  ( -17.92612601409339490, 146.8415343102147972, -2.296925525151568337 ) ) ;
#25003 = CARTESIAN_POINT ( 'NONE',  ( 4.100156219318407125, -15.52122063102406813, 2.251114749721512709 ) ) ;
#25004 = CARTESIAN_POINT ( 'NONE',  ( -4.145496126637243428, 118.2391368896328459, -0.3994797739803510606 ) ) ;
#25005 = EDGE_CURVE ( 'NONE', #21058, #37417, #30154, .T. ) ;
#25006 = EDGE_CURVE ( 'NONE', #11474, #1265, #11778, .T. ) ;
#25007 = CARTESIAN_POINT ( 'NONE',  ( -58.87911280034276018, -0.2081424763510641984, -0.2451831517279998984 ) ) ;
#25008 = CARTESIAN_POINT ( 'NONE',  ( 6.059261036834389103, 56.51500000000000057, 4.381499999999999950 ) ) ;
#25009 = CARTESIAN_POINT ( 'NONE',  ( 10.86423259349699677, 154.4230204216147513, 2.019759596344636865 ) ) ;
#25010 = FACE_OUTER_BOUND ( 'NONE', #38638, .T. ) ;
#25011 = CARTESIAN_POINT ( 'NONE',  ( 5.007560425261973869, -3.380029175189206203, 6.774419414089246416 ) ) ;
#25012 = CARTESIAN_POINT ( 'NONE',  ( 2.801574634701638367, 120.9854572005495044, 0.1568784928360138498 ) ) ;
#25013 = CARTESIAN_POINT ( 'NONE',  ( 14.73199999999999754, 61.59499999999999886, -5.016499999999999737 ) ) ;
#25014 = CARTESIAN_POINT ( 'NONE',  ( -42.80040666669066241, 21.79149265709745009, -2.067570201390457552 ) ) ;
#25015 = DIRECTION ( 'NONE',  ( -1.000000000000000000, 1.011795553208986377E-16, 0.000000000000000000 ) ) ;
#25016 = CARTESIAN_POINT ( 'NONE',  ( -6.057513928997650510, 83.56599999999998829, -1.904999999999999805 ) ) ;
#25017 = DIRECTION ( 'NONE',  ( -5.188838149069471174E-16, 1.699382548006136313E-16, 1.000000000000000000 ) ) ;
#25018 = CARTESIAN_POINT ( 'NONE',  ( -5.305748947172302721, 88.73331249999999670, -5.247078976224250013 ) ) ;
#25019 = CARTESIAN_POINT ( 'NONE',  ( -50.45326722236683281, 19.63324548489221044, 2.269669894115894593 ) ) ;
#25020 = CARTESIAN_POINT ( 'NONE',  ( -22.65966732694894503, 150.6414900647796173, -0.2998287813802532065 ) ) ;
#25021 = ORIENTED_EDGE ( 'NONE', *, *, #5067, .F. ) ;
#25022 = CARTESIAN_POINT ( 'NONE',  ( -51.10637696787394191, 21.44594517334857287, -0.3731469903906515784 ) ) ;
#25023 = CARTESIAN_POINT ( 'NONE',  ( 5.987228303333891333, 121.4272104811933275, -0.001111587135667825967 ) ) ;
#25024 = CARTESIAN_POINT ( 'NONE',  ( 16.87828382557106721, 17.14499999999999957, 0.000000000000000000 ) ) ;
#25025 = ORIENTED_EDGE ( 'NONE', *, *, #33097, .T. ) ;
#25026 = CARTESIAN_POINT ( 'NONE',  ( 3.398732499897371362, 115.7029691176617234, -1.510499792607192582 ) ) ;
#25027 = CARTESIAN_POINT ( 'NONE',  ( -5.911602206139031424, 121.5031286879076902, -0.2921876764073586541 ) ) ;
#25028 = CARTESIAN_POINT ( 'NONE',  ( 5.341062828015524566, -12.45213391371734168, 1.712110018432928982 ) ) ;
#25029 = CARTESIAN_POINT ( 'NONE',  ( -14.13727225732684012, 121.3807765770047666, 0.9276936697596736003 ) ) ;
#25030 = CARTESIAN_POINT ( 'NONE',  ( 5.385891243465063205, 78.92849802251100755, -5.190125708699709683 ) ) ;
#25031 = CARTESIAN_POINT ( 'NONE',  ( 15.88955207386058532, 121.0219768425927214, 0.4226783167178085332 ) ) ;
#25032 = CARTESIAN_POINT ( 'NONE',  ( 15.20596983381132183, 143.4108790439744610, 0.3714088703294859406 ) ) ;
#25033 = DIRECTION ( 'NONE',  ( -0.000000000000000000, -0.000000000000000000, -1.000000000000000000 ) ) ;
#25034 = CARTESIAN_POINT ( 'NONE',  ( 0.8991110484329473129, 28.35728145135693268, -0.3789830077994447155 ) ) ;
#25035 = EDGE_CURVE ( 'NONE', #40156, #4929, #19927, .T. ) ;
#25036 = CARTESIAN_POINT ( 'NONE',  ( -20.69515314362144665, 152.5608647341385335, -0.4887519660486649431 ) ) ;
#25037 = CARTESIAN_POINT ( 'NONE',  ( -41.05189575270520663, 23.09451173561983239, -1.523999999999987365 ) ) ;
#25038 = DIRECTION ( 'NONE',  ( 5.188838149069472160E-16, -1.699382548006136559E-16, -1.000000000000000000 ) ) ;
#25039 = VERTEX_POINT ( 'NONE', #5303 ) ;
#25040 = CARTESIAN_POINT ( 'NONE',  ( 4.178911134271665162, 118.4233117688550152, 1.013387016679737851 ) ) ;
#25041 = LINE ( 'NONE', #8864, #19757 ) ;
#25042 = CARTESIAN_POINT ( 'NONE',  ( 15.75167367066965340, 155.0373533369262589, 1.797107981590890580 ) ) ;
#25043 = CARTESIAN_POINT ( 'NONE',  ( 20.31268976784551228, 148.7458375694471044, -1.664162616495830083 ) ) ;
#25044 = CARTESIAN_POINT ( 'NONE',  ( 2.357476308904321360, 24.96372521773390929, -8.086248583043326832 ) ) ;
#25045 = CARTESIAN_POINT ( 'NONE',  ( -4.872874520552260336, 117.5843641943970681, -0.8145397704027564911 ) ) ;
#25046 = CARTESIAN_POINT ( 'NONE',  ( 4.929911170358315609, 117.6593520789608363, -0.7659856277397926183 ) ) ;
#25047 = CARTESIAN_POINT ( 'NONE',  ( 7.613751273744796322, 124.2930771091975117, 0.1610855651276039968 ) ) ;
#25048 = CARTESIAN_POINT ( 'NONE',  ( -15.77879114986273734, 146.5725700477668170, -0.1868612039608985864 ) ) ;
#25049 = CARTESIAN_POINT ( 'NONE',  ( -4.177977944338337579, 119.2415290214368042, -0.9917981586689073037 ) ) ;
#25050 = CARTESIAN_POINT ( 'NONE',  ( 4.813411144541747788, -15.18245576741394842, 4.205718551895911261 ) ) ;
#25051 =( BOUNDED_SURFACE ( )  B_SPLINE_SURFACE ( 3, 1, ( 
 ( #10419, #40254 ),
 ( #7449, #23390 ),
 ( #11048, #648 ),
 ( #23607, #1483 ),
 ( #7240, #17638 ),
 ( #33853, #36839 ),
 ( #39614, #3842 ),
 ( #30640, #16807 ),
 ( #4681, #36422 ),
 ( #20200, #26395 ),
 ( #23173, #17431 ),
 ( #10203, #7867 ),
 ( #17014, #7659 ),
 ( #20406, #14233 ),
 ( #24033, #33227 ),
 ( #13826, #7029 ) ),
 .UNSPECIFIED., .T., .F., .T. ) 
 B_SPLINE_SURFACE_WITH_KNOTS ( ( 4, 1, 1, 1, 1, 1, 2, 1, 1, 1, 1, 1, 4 ),
 ( 2, 2 ),
 ( 0.000000000000000000, 0.02374999999999993783, 0.1365624999999999478, 0.2493749999999999578, 0.3621874999999999956, 0.4749999999999999778, 0.5000000000000000000, 0.5250000000000000222, 0.6378125000000000044, 0.7506249999999999867, 0.8634374999999999689, 0.9762499999999999512, 1.000000000000000000 ),
 ( 0.000000000000000000, 1.000000000000000000 ),
 .UNSPECIFIED. ) 
 GEOMETRIC_REPRESENTATION_ITEM ( )  RATIONAL_B_SPLINE_SURFACE ( (
 ( 1.000000000000000000, 1.000000000000000000),
 ( 1.000000000000000222, 1.000000000000000000),
 ( 0.8208939328743548591, 1.000000000000000000),
 ( 0.5876145654044752087, 1.000000000000000000),
 ( 0.4813067448364888867, 1.000000000000000000),
 ( 0.5852845309810671415, 1.000000000000000000),
 ( 0.8180077452667815496, 1.000000000000000000),
 ( 0.9982788296041308351, 1.000000000000000000),
 ( 0.9982788296041308351, 1.000000000000000000),
 ( 0.8180077452667815496, 1.000000000000000000),
 ( 0.5852845309810672525, 1.000000000000000000),
 ( 0.4813067448364889422, 1.000000000000000000),
 ( 0.5876145654044749866, 1.000000000000000000),
 ( 0.8208939328743545261, 1.000000000000000000),
 ( 1.000000000000000000, 1.000000000000000000),
 ( 1.000000000000000000, 1.000000000000000000) ) ) 
 REPRESENTATION_ITEM ( '' )  SURFACE ( )  );
#25052 = CARTESIAN_POINT ( 'NONE',  ( 4.799946221452094264, 115.6909491485453145, 1.474290515423493764 ) ) ;
#25053 = EDGE_CURVE ( 'NONE', #22768, #6508, #32193, .T. ) ;
#25054 = CARTESIAN_POINT ( 'NONE',  ( -0.6792886333135017551, 118.1651005710540687, -0.8882677707207756734 ) ) ;
#25055 = ORIENTED_EDGE ( 'NONE', *, *, #15894, .T. ) ;
#25056 = CARTESIAN_POINT ( 'NONE',  ( 13.63191106101874617, 125.8243951943327517, 1.964466803988918153 ) ) ;
#25057 = CARTESIAN_POINT ( 'NONE',  ( -3.174366308152012373, 82.64346620154573486, -0.06343139340882730792 ) ) ;
#25058 = VECTOR ( 'NONE', #13501, 1000.000000000000000 ) ;
#25059 = DIRECTION ( 'NONE',  ( -0.9998004120163608288, 0.000000000000000000, -0.01997839162482747608 ) ) ;
#25060 = CARTESIAN_POINT ( 'NONE',  ( -1.613589725761693794, 119.1892773189224783, 0.6629358561546617734 ) ) ;
#25061 = CARTESIAN_POINT ( 'NONE',  ( -6.277010209292351206, 0.1250379130781943404, 5.629075605414042727 ) ) ;
#25062 = CARTESIAN_POINT ( 'NONE',  ( 0.6075365842365665348, 120.7136710450757988, 0.2388278564565363415 ) ) ;
#25063 = FACE_OUTER_BOUND ( 'NONE', #30449, .T. ) ;
#25064 = ADVANCED_FACE ( 'NONE', ( #24651 ), #9748, .F. ) ;
#25065 = CARTESIAN_POINT ( 'NONE',  ( 0.9832365512848652012, 116.8374933757159795, -0.2893350595372072842 ) ) ;
#25066 = DIRECTION ( 'NONE',  ( -0.8745520943968310146, 0.4849315768086426837, -5.361993529360588735E-16 ) ) ;
#25067 = CIRCLE ( 'NONE', #23686, 0.7620000000000000107 ) ;
#25068 = CARTESIAN_POINT ( 'NONE',  ( -58.05759491991644694, 0.3796087429759146814, 0.7800566416505788636 ) ) ;
#25069 = CARTESIAN_POINT ( 'NONE',  ( -8.797017425024156623, 117.6856564229855024, -0.2139691015837985044 ) ) ;
#25070 = CARTESIAN_POINT ( 'NONE',  ( -18.83202234259777086, 80.34319284215894186, -1.270000000000002904 ) ) ;
#25071 = DIRECTION ( 'NONE',  ( -0.8745520943968243532, 0.4849315768086547296, -5.361993529360573944E-16 ) ) ;
#25072 = CARTESIAN_POINT ( 'NONE',  ( -5.772319165918015749, 116.9338547871927858, -0.1153446742911716644 ) ) ;
#25073 = ORIENTED_EDGE ( 'NONE', *, *, #39751, .T. ) ;
#25074 = CARTESIAN_POINT ( 'NONE',  ( -52.76912830878634253, 12.08540908813377612, 4.334427935445234858 ) ) ;
#25075 = CARTESIAN_POINT ( 'NONE',  ( -6.333746706779065150, 120.0360757590860743, -1.205236591762536280 ) ) ;
#25076 = DIRECTION ( 'NONE',  ( 0.9998004120163610509, 5.205824365704083805E-17, 0.01997839162482749689 ) ) ;
#25077 = CARTESIAN_POINT ( 'NONE',  ( -7.089475284344026740, 121.8675249661327626, -0.6210822171188465912 ) ) ;
#25078 = CARTESIAN_POINT ( 'NONE',  ( 5.008579095262371439, 117.3966161975143052, -0.7759206765000108419 ) ) ;
#25079 = CARTESIAN_POINT ( 'NONE',  ( -37.66124916107632714, 74.02712188174415076, -1.270000000000011786 ) ) ;
#25080 = EDGE_LOOP ( 'NONE', ( #9344, #16215, #2522, #9337, #23030, #36986 ) ) ;
#25081 = CARTESIAN_POINT ( 'NONE',  ( 0.6590154617207463206, 19.50938314818779062, -4.574821423538240950 ) ) ;
#25082 = CARTESIAN_POINT ( 'NONE',  ( -33.42971872652992005, 49.93539301574497102, 1.269999999999994023 ) ) ;
#25083 = FACE_OUTER_BOUND ( 'NONE', #2804, .T. ) ;
#25084 = CARTESIAN_POINT ( 'NONE',  ( 6.262914499211069241, 78.85772796343783853, -4.069400916056300055 ) ) ;
#25085 = CARTESIAN_POINT ( 'NONE',  ( -23.49500000000000455, 71.11999999999999034, -1.904999999999999583 ) ) ;
#25086 = CARTESIAN_POINT ( 'NONE',  ( 7.796227911047320269, 122.5475566638853877, 0.4040998892956136346 ) ) ;
#25087 = EDGE_CURVE ( 'NONE', #22433, #3009, #28784, .T. ) ;
#25088 = CIRCLE ( 'NONE', #16232, 0.5080000000000002292 ) ;
#25089 = CARTESIAN_POINT ( 'NONE',  ( 4.353980591602404360, 23.44215234368072487, -1.583070106892425111 ) ) ;
#25090 = CARTESIAN_POINT ( 'NONE',  ( 20.52999062792637019, 132.2049894596293313, 1.489094535601873215 ) ) ;
#25091 = CARTESIAN_POINT ( 'NONE',  ( 4.211467216454458651, 104.6144662015457527, -2.363859967688341168 ) ) ;
#25093 = CARTESIAN_POINT ( 'NONE',  ( 12.17409717887508513, 120.5818589831333441, -1.028275848330292730 ) ) ;
#25092 = CARTESIAN_POINT ( 'NONE',  ( 2.232013814210268343, -15.18320146713449148, 5.067049754691558050 ) ) ;
#25094 = CARTESIAN_POINT ( 'NONE',  ( -17.94049195465775881, 148.7876888829155746, 1.661648619591604481 ) ) ;
#25095 = CIRCLE ( 'NONE', #16912, 0.2539999999999992819 ) ;
#25096 = CARTESIAN_POINT ( 'NONE',  ( -3.199182136055901626, 19.34408232073488065, 3.339653329369344004 ) ) ;
#25097 = CARTESIAN_POINT ( 'NONE',  ( -15.61264994714022869, 121.4606353739761744, -1.010464550865948441 ) ) ;
#25098 = EDGE_CURVE ( 'NONE', #28177, #1859, #2288, .T. ) ;
#25099 = CARTESIAN_POINT ( 'NONE',  ( -0.9160044981361634697, -1.370538221358817310, 0.3309596765904046500 ) ) ;
#25100 = ORIENTED_EDGE ( 'NONE', *, *, #7471, .T. ) ;
#25101 = CARTESIAN_POINT ( 'NONE',  ( -57.22211421646275653, 1.778355698664441098, -1.009576694067165286E-14 ) ) ;
#25102 = CARTESIAN_POINT ( 'NONE',  ( -9.286476516978044771, 123.9149913687586064, 0.2326040378870057601 ) ) ;
#25103 = CARTESIAN_POINT ( 'NONE',  ( 4.204793715662772158, -14.23101105591234550, 4.663061278791505337 ) ) ;
#25104 = CARTESIAN_POINT ( 'NONE',  ( 6.537359847799108614, 121.1369950346570192, -0.6189803324213466462 ) ) ;
#25105 = ORIENTED_EDGE ( 'NONE', *, *, #26636, .F. ) ;
#25106 = CARTESIAN_POINT ( 'NONE',  ( 2.812738770403601318, 115.7033313022755436, 1.680254796076790180 ) ) ;
#25107 = VERTEX_POINT ( 'NONE', #5506 ) ;
#25108 = CARTESIAN_POINT ( 'NONE',  ( -4.674760407624344971, 117.8378351759783556, -1.036698452010090810 ) ) ;
#25109 = CARTESIAN_POINT ( 'NONE',  ( 13.59242215834131962, 150.2357272821285221, 0.2218801189746054114 ) ) ;
#25110 = EDGE_CURVE ( 'NONE', #17903, #39565, #6024, .T. ) ;
#25111 = EDGE_LOOP ( 'NONE', ( #11690, #30990, #3303 ) ) ;
#25112 = CARTESIAN_POINT ( 'NONE',  ( 15.71367270535921712, 153.2725199748809928, 2.344280857665636209 ) ) ;
#25113 = DIRECTION ( 'NONE',  ( -0.8745520943968269068, 0.4849315768086501222, -8.537024980200721238E-16 ) ) ;
#25114 = CARTESIAN_POINT ( 'NONE',  ( 5.348924234570989533, 56.51499999999999346, 4.492130288940735738 ) ) ;
#25115 = CARTESIAN_POINT ( 'NONE',  ( 0.003550340867665223877, 156.3099534201614631, -0.1776735749810080256 ) ) ;
#25116 = CARTESIAN_POINT ( 'NONE',  ( 16.81673201796756700, 155.2524275687165982, 0.03818847721825018027 ) ) ;
#25117 = VECTOR ( 'NONE', #5504, 1000.000000000000114 ) ;
#25118 = AXIS2_PLACEMENT_3D ( 'NONE', #26821, #23815, #20612 ) ;
#25119 = DIRECTION ( 'NONE',  ( -0.01731298258488772612, 0.9998501190848634312, -1.788962107505314851E-16 ) ) ;
#25120 = CARTESIAN_POINT ( 'NONE',  ( -46.95274714683655759, 25.03842815569886326, 1.954508796226629208 ) ) ;
#25121 = DIRECTION ( 'NONE',  ( 0.9469626219732555361, 0.3213437296502561491, 8.537024980200885913E-16 ) ) ;
#25122 = CARTESIAN_POINT ( 'NONE',  ( 1.836962934898605404, -15.06515874082747786, 5.710661141901725024 ) ) ;
#25123 = CARTESIAN_POINT ( 'NONE',  ( -47.16890147375937659, 22.20336809214646578, 4.187060126831876339 ) ) ;
#25124 = CARTESIAN_POINT ( 'NONE',  ( -24.10666987309389597, 82.16896248603319464, -1.524000000000006239 ) ) ;
#25125 = CARTESIAN_POINT ( 'NONE',  ( -4.696693711212855504, 117.9632058761038564, 0.7093352692556416095 ) ) ;
#25126 = EDGE_CURVE ( 'NONE', #13983, #29032, #30901, .T. ) ;
#25127 = ORIENTED_EDGE ( 'NONE', *, *, #26050, .T. ) ;
#25128 = ORIENTED_EDGE ( 'NONE', *, *, #31380, .T. ) ;
#25129 = DIRECTION ( 'NONE',  ( -5.188838149069472160E-16, 1.699382548006136559E-16, 1.000000000000000000 ) ) ;
#25130 = CARTESIAN_POINT ( 'NONE',  ( -3.087959230053988868, 118.2558998309379064, -0.8917549213772042460 ) ) ;
#25131 = CARTESIAN_POINT ( 'NONE',  ( -5.925882289753597654, 120.8604418758245487, -0.3792092984231498209 ) ) ;
#25132 = CARTESIAN_POINT ( 'NONE',  ( 4.796130219922325466, 117.5429647511544431, 1.162721217937990659 ) ) ;
#25133 = FACE_OUTER_BOUND ( 'NONE', #17690, .T. ) ;
#25134 = CARTESIAN_POINT ( 'NONE',  ( -0.3885115210726761137, 119.2343925067223722, 0.8110907263698887704 ) ) ;
#25135 = CARTESIAN_POINT ( 'NONE',  ( 4.611808778022512989, -11.57686662695173929, 0.3579861242195471194 ) ) ;
#25136 = CARTESIAN_POINT ( 'NONE',  ( -58.50860430493788300, 0.7049166599848583070, 0.9756837515128382599 ) ) ;
#25137 = DIRECTION ( 'NONE',  ( -0.9998004120163608288, 0.000000000000000000, -0.01997839162482749342 ) ) ;
#25138 = CARTESIAN_POINT ( 'NONE',  ( 2.584330390446285985, -14.72226154538576459, 5.166463236119047231 ) ) ;
#25139 = CARTESIAN_POINT ( 'NONE',  ( 5.380575101947356664, 117.2069880336854197, -0.6820287515226022279 ) ) ;
#25140 = CARTESIAN_POINT ( 'NONE',  ( -10.21894633145453035, 123.0849000269954701, -1.386333990434162722 ) ) ;
#25141 = CARTESIAN_POINT ( 'NONE',  ( -5.348924234571056147, 56.51499999999999346, 4.492130288940740179 ) ) ;
#25142 = CARTESIAN_POINT ( 'NONE',  ( -0.2616981356411249848, 38.12352966651759090, 1.602708108658221553 ) ) ;
#25143 = CARTESIAN_POINT ( 'NONE',  ( -0.6753594273997497455, 115.7031289524320243, 1.734270338090476260 ) ) ;
#25144 = CARTESIAN_POINT ( 'NONE',  ( 0.3994026957563919789, 5.465888722076803319, 4.619092260001838923 ) ) ;
#25146 = ORIENTED_EDGE ( 'NONE', *, *, #6109, .T. ) ;
#25145 = CARTESIAN_POINT ( 'NONE',  ( 21.25299977426486464, 132.4531229209162575, 0.9669248719381913215 ) ) ;
#25147 = CARTESIAN_POINT ( 'NONE',  ( 1.273769851498584904, 105.1233871752103113, -5.190496487146082139 ) ) ;
#25148 = CARTESIAN_POINT ( 'NONE',  ( 3.048550003781630213, -15.65190959513015834, 4.520219006486421165 ) ) ;
#25149 = B_SPLINE_CURVE_WITH_KNOTS ( 'NONE', 3,
 ( #21803, #38238, #41009, #28000, #24806, #37386, #15214, #8625, #21587, #24586, #34617, #28216, #41223, #9054, #37591, #38019, #12242, #5030, #8840, #22019, #34830, #35048, #2465, #18620, #31626, #1624, #14580, #6909, #16260, #16049, #25650, #38657, #29263, #22429, #36094, #9465, #16475, #29052, #35458, #3514, #15633, #19038, #9264, #22637, #29479, #13073, #23062, #26064, #32044, #2881, #41649, #9876, #39283, #32467, #35673 ),
 .UNSPECIFIED., .F., .F.,
 ( 4, 2, 2, 2, 2, 1, 2, 2, 2, 2, 2, 1, 2, 2, 2, 2, 2, 1, 1, 2, 2, 2, 2, 2, 1, 2, 2, 2, 2, 4 ),
 ( 0.000000000000000000, 0.03125000000001328104, 0.06250000000002656209, 0.09375000000003984313, 0.1093750000000492661, 0.1171875000000572181, 0.1210937500000612149, 0.1250000000000652256, 0.1875000000000549283, 0.2187500000000527078, 0.2343750000000545952, 0.2421875000000584532, 0.2460937500000603129, 0.2500000000000621725, 0.3749999999999173994, 0.4374999999998416267, 0.4687499999998037126, 0.4843749999997847278, 0.4921874999997781774, 0.4960937499997777889, 0.4999999999997774003, 0.6249999999998002709, 0.6874999999998119282, 0.7187499999998145928, 0.7343749999998159250, 0.7421874999998194777, 0.7499999999998230304, 0.8749999999999115152, 0.9374999999999558131, 1.000000000000000000 ),
 .UNSPECIFIED. ) ;
#25150 = CARTESIAN_POINT ( 'NONE',  ( -12.53898343483658273, 122.9501582372872406, 1.331292802868025538 ) ) ;
#25151 = CARTESIAN_POINT ( 'NONE',  ( 0.4517697234110209514, 20.42248995698831493, 0.8659212905253524939 ) ) ;
#25152 = ADVANCED_FACE ( 'NONE', ( #6543 ), #3144, .F. ) ;
#25153 = CARTESIAN_POINT ( 'NONE',  ( 0.7153056356866435150, 7.414959551268969662, 0.6636563042211964802 ) ) ;
#25154 = VERTEX_POINT ( 'NONE', #42129 ) ;
#25155 = EDGE_CURVE ( 'NONE', #5382, #24401, #31506, .T. ) ;
#25156 = VERTEX_POINT ( 'NONE', #22281 ) ;
#25157 = CARTESIAN_POINT ( 'NONE',  ( -41.05189575270519242, 23.09451173561982174, 0.2116666666666617014 ) ) ;
#25158 = CARTESIAN_POINT ( 'NONE',  ( 1.155851712377341745, 107.4826764677166864, 4.671650131992445054 ) ) ;
#25159 =( NAMED_UNIT ( * ) PLANE_ANGLE_UNIT ( ) SI_UNIT ( $, .RADIAN. ) );
#25160 = CARTESIAN_POINT ( 'NONE',  ( -16.53085885483085704, 146.5532241433796230, 0.9478179252731555593 ) ) ;
#25161 = CARTESIAN_POINT ( 'NONE',  ( -12.69999999999999574, 11.53894877578617262, 0.000000000000000000 ) ) ;
#25162 = AXIS2_PLACEMENT_3D ( 'NONE', #33382, #26777, #29965 ) ;
#25163 = CARTESIAN_POINT ( 'NONE',  ( 3.853068500771395399, -13.31557002055877525, 3.124774401994960815 ) ) ;
#25164 = CARTESIAN_POINT ( 'NONE',  ( 11.41761608106091685, 123.3954635094115702, -1.178011644471332220 ) ) ;
#25165 = APPLICATION_CONTEXT ( 'automotive_design' ) ;
#25166 = CARTESIAN_POINT ( 'NONE',  ( -20.31017440411242347, 148.4497675966422889, -2.477828910454907163 ) ) ;
#25167 = DIRECTION ( 'NONE',  ( 0.000000000000000000, 0.000000000000000000, 1.000000000000000000 ) ) ;
#25168 = CARTESIAN_POINT ( 'NONE',  ( 8.795780368329440435, 117.6859443280086026, 0.2729219573496977080 ) ) ;
#25169 = CARTESIAN_POINT ( 'NONE',  ( -6.446885413170102552, 29.42808026494702389, 0.2842954123359195950 ) ) ;
#25170 = CARTESIAN_POINT ( 'NONE',  ( 2.954508604761920676, 156.0884104482065595, -0.2429312420959231777 ) ) ;
#25171 = ORIENTED_EDGE ( 'NONE', *, *, #7929, .F. ) ;
#25172 = CARTESIAN_POINT ( 'NONE',  ( -1.809052985942710023, 106.7492432543851777, -4.947880635703119090 ) ) ;
#25173 = CARTESIAN_POINT ( 'NONE',  ( 10.28897677580358128, 56.51500000000000057, 4.381499999999999950 ) ) ;
#25174 = DIRECTION ( 'NONE',  ( 0.1715592850456333363, -0.1224830539174543431, 0.9775302108976914317 ) ) ;
#25175 = CARTESIAN_POINT ( 'NONE',  ( -58.44960050528106876, -0.4277149010491103076, 0.3217025345704653261 ) ) ;
#25176 = CARTESIAN_POINT ( 'NONE',  ( 4.581790953832888924, -15.30257397518579232, -0.5115867857466148694 ) ) ;
#25177 = CARTESIAN_POINT ( 'NONE',  ( 15.56955422694807112, 149.1167355181319181, 1.737459915651670350 ) ) ;
#25178 = PLANE ( 'NONE',  #41680 ) ;
#25179 = CARTESIAN_POINT ( 'NONE',  ( 22.75657594704711784, 137.3797884758947703, 0.4311216471409409778 ) ) ;
#25180 = CARTESIAN_POINT ( 'NONE',  ( -5.249845242698206960, 116.4925209815607730, 0.8804580864248583438 ) ) ;
#25181 = CARTESIAN_POINT ( 'NONE',  ( -0.2084201458593382406, 5.265951782950084592, 4.622859108429906883 ) ) ;
#25182 = CARTESIAN_POINT ( 'NONE',  ( 9.104209967887914701, 153.9432936505793066, 0.1819237819739444872 ) ) ;
#25183 = AXIS2_PLACEMENT_3D ( 'NONE', #36871, #7687, #20646 ) ;
#25184 = CARTESIAN_POINT ( 'NONE',  ( 8.407117359195193984, -5.923529430292941989, 0.7350785369227282873 ) ) ;
#25185 = CARTESIAN_POINT ( 'NONE',  ( -8.773404058708813125, 117.7735243877689726, -0.4939657326346613697 ) ) ;
#25186 = CARTESIAN_POINT ( 'NONE',  ( -0.8061429914042389511, 121.2007779179981384, -0.4207382890248004825 ) ) ;
#25187 = DIRECTION ( 'NONE',  ( -0.8745520943968240202, 0.4849315768086551737, -5.361993529360572958E-16 ) ) ;
#25188 = CARTESIAN_POINT ( 'NONE',  ( 4.496586626007489151, 27.28078351817337222, -1.068494511273165193 ) ) ;
#25189 = CARTESIAN_POINT ( 'NONE',  ( 2.751661733825109923, 117.9394479625293997, 1.329244536658263698 ) ) ;
#25190 = FACE_OUTER_BOUND ( 'NONE', #18625, .T. ) ;
#25191 = CARTESIAN_POINT ( 'NONE',  ( 0.7705677718991392755, 119.3684187487962305, -0.7342037314787065450 ) ) ;
#25192 = CARTESIAN_POINT ( 'NONE',  ( -18.31971715989132221, 125.1624627582897915, 0.2149060778942797345 ) ) ;
#25193 = ORIENTED_EDGE ( 'NONE', *, *, #29820, .F. ) ;
#25194 = CARTESIAN_POINT ( 'NONE',  ( -9.665786669610962889, 56.51499999999998636, 0.1866227975165156705 ) ) ;
#25195 = ORIENTED_EDGE ( 'NONE', *, *, #34773, .T. ) ;
#25196 = CARTESIAN_POINT ( 'NONE',  ( -8.438477507926631205, 69.62414081991882142, 1.270000000000003126 ) ) ;
#25197 = CARTESIAN_POINT ( 'NONE',  ( -9.463739348024544640, 124.7787758165406444, -0.09662325335671638482 ) ) ;
#25198 = CARTESIAN_POINT ( 'NONE',  ( 5.457633994894312224, -14.92472868577397804, 3.194711634204877804 ) ) ;
#25199 = CARTESIAN_POINT ( 'NONE',  ( -20.48420673234498679, 149.1468970683199586, 1.615293151967227780 ) ) ;
#25200 = AXIS2_PLACEMENT_3D ( 'NONE', #15074, #23131, #35319 ) ;
#25201 = CARTESIAN_POINT ( 'NONE',  ( 19.78757913416905723, 132.0165317526581816, -1.053352019815566365 ) ) ;
#25202 = CARTESIAN_POINT ( 'NONE',  ( -4.420329592304260480, 21.65838872207745425, -1.398650104627336743 ) ) ;
#25203 = CARTESIAN_POINT ( 'NONE',  ( -4.764559463232044934, 116.8420656028321218, -0.3170442335454676797 ) ) ;
#25204 = CARTESIAN_POINT ( 'NONE',  ( -57.59359650234090822, 1.936081701823850088, -1.738013837494228220 ) ) ;
#25205 = ORIENTED_EDGE ( 'NONE', *, *, #32717, .F. ) ;
#25206 = LINE ( 'NONE', #29234, #15886 ) ;
#25207 = B_SPLINE_SURFACE_WITH_KNOTS ( 'NONE', 3, 3, ( 
 ( #3361, #13145, #16328, #32319, #388, #3148, #29334, #32969, #6978, #175, #26137, #22495, #32749, #19314, #3582, #13571, #35522, #25711, #10154, #10371, #16111, #13355, #26560, #36162, #26344, #23342, #36380, #38717, #9527, #5050, #23766, #17796, #13778, #40204, #34220, #30377, #23980, #10580, #30592, #7608, #11205, #11001, #37199, #39995, #17589, #4429, #39785 ),
 ( #17387, #1227, #26775, #24189, #37000, #33380, #1432, #18006, #7819, #27603, #14186, #33596, #23558, #33805, #14597, #27189, #20781, #803, #36579, #8221, #37402, #20569, #30793, #13980, #4633, #30175, #20357, #14391, #4215, #1016, #20991, #8020, #26985, #10786, #7395, #36791, #17176, #34014, #24398, #1644, #40612, #27399, #40409, #4842, #11411, #21194, #18210 ),
 ( #38257, #22039, #34635, #34424, #25252, #2485, #5462, #5256, #11837, #28019, #28656, #18850, #31430, #2272, #37819, #9074, #38466, #41241, #35067, #31855, #2054, #41029, #24824, #15236, #25470, #31211, #41668, #8438, #14809, #8647, #2694, #21607, #31002, #18640, #15019, #18422, #25036, #28235, #28450, #5889, #5682, #9284, #12046, #38038, #8858, #21822, #15652 ),
 ( #22244, #41456, #12476, #34850, #31645, #15447, #35270, #12260, #6094, #1845, #27811, #40819, #11620, #24607, #37612, #21396, #32487, #3108, #19685, #28869, #32278, #13308, #16069, #32701, #16704, #10111, #22659, #3537, #26513, #10324, #38677, #42091, #25670, #25874, #29502, #22447, #29072, #26295, #19057, #35476, #12886, #38880, #9692, #3315, #29709, #16496, #342 ),
 ( #39303, #41881, #13525, #29286, #32916, #2901, #39519, #23293, #15863, #23082, #32063, #16281, #130, #35692, #9483, #13095, #36331, #12680, #26087, #6300, #36116, #19271, #6501, #6930, #19901, #19479, #3746, #551, #39094, #9896, #22869, #35907, #6716, #10737, #10534, #1382, #20734, #23719, #23503, #30129, #4165, #4795, #37151, #7560, #20520, #13937, #14340 ),
 ( #40363, #7973, #20309, #17128, #968, #33550, #1596, #36530, #17746, #26727, #33128, #26933, #20942, #39945, #7147, #36951, #7350, #36737, #1175, #4381, #4584, #27350, #23934, #27561, #17543, #17339, #11158, #30329, #7771, #14138, #3958, #40153, #10945, #27140, #33758, #16919, #30544, #24143, #39735, #33967, #40568, #30746, #14553, #11366, #24352, #20104, #29919 ),
 ( #758, #13733, #33335, #3209, #32379, #14970, #25203, #8387, #37772, #24557, #14762, #11995, #27763, #37561, #15396, #31598, #21351, #34376, #5001, #18164, #34173, #28401, #19373, #12213, #38207, #5209, #18372, #8177, #31379, #29175, #31167, #24989, #11571, #8813, #34588, #2223, #41406, #2008, #24774, #9024, #15183, #41191, #27972, #37989, #16170, #40982, #21987 ),
 ( #21, #5417, #35020, #5841, #11784, #8597, #21560, #28187, #12987, #21772, #37358, #40773, #21144, #34798, #17959, #5631, #30959, #18589, #2435, #1799, #20007, #26405, #23401, #20210, #658, #4273, #16603, #6818, #26192, #4065, #13626, #3421, #33446, #36432, #26834, #39410, #39196, #29819, #30023, #3638, #10004, #13416, #10638, #33024, #22976, #863, #17236 ),
 ( #36006, #26617, #35797, #19788, #22764, #16817, #39624, #29611, #10213, #9798, #7251, #36218, #16388, #10430, #30232, #7039, #23617, #446, #23183, #38988, #33237, #39841, #3853, #17025, #1071, #6610, #25980, #20418, #13836, #36638, #32807, #7460, #13210, #29393, #19580, #233, #32588, #34284, #8285, #14243, #1285, #23831, #37059, #10845, #5113, #37677, #31068 ),
 ( #37259, #27043, #8078, #5319, #27250, #1704, #30439, #27663, #11265, #21051, #18065, #20840, #1495, #1906, #34077, #17858, #11059, #30859, #21457, #40266, #14870, #7669, #24251, #24044, #7877, #24456, #34487, #33864, #4904, #18271, #40881, #27872, #4694, #20627, #14659, #11682, #24668, #8500, #31273, #14039, #33657, #36851, #40674, #40052, #4482, #11467, #17442 ),
 ( #17649, #30651, #37460, #21254, #14451, #27461, #40474, #28917, #37884, #8707, #35324, #12528, #21671, #5740, #6150, #19326, #19117, #6355, #25097, #32123, #15079, #41514, #35536, #31703, #25308, #11898, #31917, #8916, #25519, #12321, #38519, #41303, #18906, #18693, #9336, #2954, #2545, #5524, #22299, #15709, #15506, #18481, #38101, #12107, #41932, #15917, #28507 ),
 ( #31486, #21882, #12733, #22507, #34908, #38312, #2116, #25722, #38730, #2331, #34694, #9132, #9537, #28079, #41090, #24887, #15291, #28296, #22093, #5947, #35120, #2753, #28713, #41723, #26148, #10383, #29126, #25931, #29563, #39578, #12940, #10590, #16765, #16974, #38938, #9750, #23353, #608, #22718, #35958, #36390, #7408, #7206, #36590, #13156, #20164, #3159 ),
 ( #13366, #42146, #19960, #39150, #13582, #399, #26570, #29345, #6990, #6772, #35746, #23134, #36173, #19738, #32760, #16123, #33189, #26355, #6558, #32978, #23568, #39361, #29973, #3593, #22927, #19533, #3803, #4017, #16555, #10166, #32330, #32540, #39796, #26786, #9954, #814, #3373, #29772, #16339, #186, #13789, #10798, #7620, #40624, #14609, #20580, #33607 ),
 ( #17187, #11422, #1857, #37414, #8233, #30389, #1442, #33392, #14402, #11630, #4439, #8031, #36801, #34027, #4643, #17600, #23991, #26996, #33816, #40831, #1027, #27410, #4227, #24408, #30186, #23780, #21206, #4852, #20791, #34232, #5062, #30604, #18017, #40421, #27614, #31014, #37011, #17397, #14820, #17808, #7829, #1240, #14196, #27201, #27822, #24617, #11216 ),
 ( #37625, #20370, #24200, #13991, #40007, #40214, #11012, #37211, #21002, #30805, #1655, #6105, #28029, #34434, #15245, #38475, #18431, #8449, #38266, #24835, #38048, #2495, #8868, #5899, #2704, #25261, #28880, #41250, #31439, #8657, #28665, #9083, #41039, #15873, #18860, #9293, #21830, #21617, #12272, #12485, #28246, #34644, #34859, #35280, #15458, #5472, #31656 ),
 ( #41677, #2281, #22049, #18220, #12056, #15661, #25045, #35077, #19068, #25480, #5691, #31864, #41892, #12690, #11849, #18649, #15029, #28459, #22255, #37830, #41465, #32074, #21406, #2910, #25680, #5268, #31221, #2065, #36342, #36127, #23093, #10122, #26306, #6942, #6309, #33138, #6728, #10335, #22458, #3968, #16929, #35487, #29719, #38687, #767, #19281, #29929 ),
 ( #26524, #9703, #39105, #25884, #16078, #13320, #29082, #38891, #16716, #32928, #22670, #35703, #32289, #19489, #3118, #561, #20116, #13536, #39530, #6514, #19695, #9493, #32712, #13744, #32498, #39315, #12896, #19912, #35918, #3547, #23304, #3327, #26099, #7157, #16507, #353, #16293, #3758, #42102, #29297, #141, #13107, #29514, #9908, #22880, #37160, #5008 ),
 ( #23729, #10955, #21152, #980, #24360, #4175, #10544, #33559, #14561, #36748, #26737, #14348, #13945, #14147, #20743, #27150, #24151, #20950, #1392, #17969, #17349, #7569, #26943, #4802, #27359, #17137, #34182, #7981, #27567, #40162, #39954, #30553, #30753, #4393, #10748, #23942, #11373, #33768, #20530, #7782, #33974, #30337, #17753, #1184, #40371, #36540, #36959 ),
 ( #11167, #37365, #1604, #4593, #40576, #30967, #1808, #30139, #17552, #33345, #8184, #39746, #23513, #7359, #20318, #14769, #31175, #40989, #34596, #24783, #28195, #12434, #12221, #41415, #35029, #8606, #5849, #11580, #8396, #12005, #21997, #37569, #35229, #25212, #41627, #21358, #34384, #18804, #38216, #5218, #18381, #31815, #32022, #2653, #19016, #37781, #15611 ),
 ( #27771, #28409, #37997, #24565, #2444, #21568, #9032, #24997, #28616, #11792, #31606, #31389, #18172, #5640, #18598, #2232, #15192, #40782, #25427, #8821, #2016, #15405, #6056, #21781, #38428, #41201, #5425, #14980, #9242, #22200, #34807, #27981, #7101, #28828, #10277, #39472, #22614, #32868, #16027, #3273, #32237, #22407, #19640, #35433, #3069, #23038, #39260 ),
 ( #12638, #25828, #41842, #36069, #26469, #19854, #3700, #12843, #26039, #15820, #39048, #36281, #29027, #32654, #19227, #16448, #82, #9854, #6885, #9647, #32442, #16660, #22824, #6674, #42046, #3490, #23247, #38838, #29667, #38635, #13048, #35648, #6462, #13266, #20062, #19436, #35861, #2860, #508, #13481, #16234, #9440, #29454, #25625, #6257, #29238, #293 ),
 ( #26250, #10066, #27097, #33504, #30498, #36694, #39688, #4334, #11322, #13689, #40108, #16876, #24104, #29877, #23459, #37112, #4539, #17298, #7932, #11116, #30288, #17705, #1129, #40323, #20901, #7516, #36486, #27309, #17500, #20478, #7307, #13896, #30084, #30705, #33922, #14098, #10901, #39897, #4753, #40530, #23892, #1554, #14510, #4123, #923, #26888, #36909 ),
 ( #7726, #27523, #24311, #37316, #8133, #33083, #26680, #10489, #20693, #3914, #715, #33717, #20266, #10694, #33295, #17084, #23674, #1341, #14297, #1760, #41577, #5590, #5798, #14720, #27722, #12169, #31549, #40731, #24734, #25166, #38378, #38165, #25373, #1967, #8979, #34976, #12386, #21106, #34755, #2181, #30922, #8773, #27931, #2394, #18333, #15353, #18125 ),
 ( #17917, #11956, #24948, #37736, #21520, #4957, #28359, #31336, #11531, #21733, #34131, #15139, #18754, #8560, #11746, #24512, #37948, #31764, #34553, #5378, #37520, #8344, #28569, #15565, #40939, #21946, #34342, #28143, #21313, #5171, #18545, #31130, #14931, #41366, #41150, #2606, #3221, #12996, #6209, #25990, #16614, #38581, #13221, #2811, #19385, #25576, #32186 ),
 ( #19180, #32389, #29621, #36015, #39207, #9392, #15772, #16182, #10016, #6829, #32818, #19798, #26203, #28777, #31974, #38999, #456, #22988, #9809, #29403, #3020, #243, #6005, #41789, #6414, #16397, #12587, #13429, #35807, #3648, #22355, #35380, #26416, #19589, #15976, #12789, #9191, #22147, #35179, #18967, #28973, #41993, #25779, #38787, #9597, #22776, #29185 ),
 ( #22567, #32599, #32, #3432, #35596, #6622, #873, #36227, #30241, #1081, #13845, #39851, #23193, #7679, #7469, #29828, #27054, #31226, #20429, #24622, #26843, #30032, #10224, #14050, #11637, #10647, #23628, #2070, #7049, #5275, #34440, #17034, #27827, #10439, #36647, #26626, #16826, #40061, #667, #39634, #17451, #33668, #23411, #36441, #20016, #20219, #33034 ),
 ( #14824, #40835, #7259, #33456, #3862, #4284, #15035, #33245, #10854, #13635, #23841, #17248, #36863, #30450, #4074, #20638, #4492, #1862, #37630, #8455, #21413, #18225, #39420, #41255, #41682, #25686, #19073, #31660, #12489, #35493, #19287, #5477, #8872, #34649, #34864, #38479, #31443, #38053, #22260, #28035, #2286, #12062, #5695, #21835, #41469, #38691, #25484 ),
 ( #11854, #6314, #22464, #18655, #15877, #25049, #28464, #15249, #18437, #2709, #28250, #2499, #6110, #35284, #15463, #12277, #37836, #25267, #24841, #32079, #9498, #2916, #28884, #38271, #9087, #41044, #22053, #32293, #35082, #15665, #5903, #9298, #18865, #31870, #41896, #28671, #12694, #3122, #8663, #21623, #13115, #32934, #23520, #3333, #20122, #9710, #26314 ),
 ( #26531, #36548, #26106, #39322, #7367, #773, #3975, #16302, #22675, #10128, #16936, #13750, #39755, #26745, #33147, #35710, #38898, #19919, #20325, #29935, #3764, #36349, #9916, #7163, #12901, #6519, #13326, #23313, #19494, #33352, #568, #10552, #32505, #29304, #16082, #39536, #148, #19702, #29087, #42107, #25890, #39111, #22886, #35924, #6734, #32721, #3555 ),
 ( #23100, #16514, #36133, #29520, #360, #16723, #6951, #29726, #13542, #10342, #24364, #10962, #33774, #34188, #40377, #7987, #1193, #20957, #11586, #33566, #8188, #39962, #14354, #20536, #27156, #14566, #24569, #14153, #27366, #37575, #30972, #5014, #4399, #10754, #11172, #17973, #1812, #27775, #14775, #21157, #23736, #26950, #33979, #8402, #40786, #4808, #37370 ),
 ( #986, #36756, #1398, #11377, #7575, #21362, #30759, #4181, #17356, #30344, #17145, #27572, #40170, #7788, #30147, #13952, #23949, #36967, #20750, #4601, #17558, #30559, #24157, #17759, #37166, #1609, #40580, #41207, #2657, #31610, #28620, #31393, #9037, #38003, #31179, #25217, #38220, #8825, #34811, #18177, #15615, #2449, #24788, #22002, #25631, #15409, #19020 ),
 ( #35034, #6060, #21785, #5646, #38641, #2020, #41847, #28834, #12009, #22204, #5429, #18604, #21574, #11798, #5854, #37785, #34600, #12439, #41631, #18385, #2238, #14984, #15197, #27986, #25432, #8610, #28200, #25002, #32027, #35235, #28414, #41419, #12226, #38432, #12644, #18810, #9248, #2865, #31819, #15826, #9446, #34389, #5223, #40994, #29673, #29033, #35439 ),
 ( #35655, #22412, #300, #38844, #26045, #19646, #39055, #10072, #36075, #29461, #23254, #29244, #32448, #22621, #6892, #13272, #12849, #36288, #39266, #16666, #9860, #6468, #16455, #32876, #16241, #19443, #22831, #515, #32661, #3280, #6680, #23044, #89, #3707, #13054, #26257, #3075, #35867, #19860, #3496, #13488, #26475, #39479, #10283, #6263, #19234, #32244 ),
 ( #9653, #16034, #42054, #25835, #28337, #12566, #18311, #34734, #2372, #38144, #41346, #31741, #15956, #15748, #2791, #31952, #5983, #28753, #28120, #12769, #28547, #32162, #2157, #25759, #38766, #15117, #9371, #31313, #2585, #15545, #21924, #24927, #41555, #9577, #41129, #25351, #11935, #22335, #37925, #8748, #35358, #41766, #18731, #6188, #38558, #12363, #2996 ),
 ( #19157, #34954, #21710, #25553, #28952, #5777, #5565, #41970, #22546, #18522, #31528, #15330, #12148, #25140, #35575, #8957, #38354, #9171, #22127, #35157, #18946, #434, #39830, #35784, #36206, #22752, #19995, #3627, #13404, #26606, #13196, #35993, #36421, #26394, #10201, #3408, #23172, #13825, #6598, #10418, #9, #16592, #19567, #29381, #16806, #26823, #16376 ),
 ( #33226, #7239, #32576, #12975, #29600, #20199, #4052, #30012, #17013, #23389, #25968, #29163, #7028, #10625, #851, #33013, #39613, #221, #23606, #3196, #38976, #39399, #13616, #9784, #6393, #3841, #19363, #26180, #39183, #32368, #29808, #9992, #22964, #16159, #6807, #19776, #32796, #647, #11453, #8272, #27860, #40868, #8064, #17637, #4262, #24237, #1274 ),
 ( #34272, #27650, #40253, #21039, #1894, #11669, #14026, #17430, #1061, #14231, #4891, #40041, #4472, #30845, #36627, #10834, #20615, #27239, #30428, #7865, #5100, #34064, #17846, #1692, #37247, #14647, #17225, #31055, #4680, #21242, #20405, #14856, #7448, #33435, #40661, #30221, #27032, #23818, #36838, #11047, #24444, #7658, #37048, #33645, #24032, #11253, #20827 ),
 ( #37448, #33852, #30639, #1482, #14438, #27447, #18052, #40463, #32156, #22960, #35569, #6593, #6387, #39180, #13190, #19357, #19772, #32363, #215, #26175, #38761, #38553, #29376, #19561, #9572, #9366, #15951, #2989, #32792, #35989, #3191, #16153, #41965, #9987, #429, #29158, #6803, #3622, #6183, #28948, #12764, #4, #29596, #22330, #16587, #12561, #18941 ),
 ( #25754, #35152, #22747, #35354, #22542, #12970, #25963, #32571, #13400, #9780, #26388, #38970, #35778, #19152, #39395, #3403, #25550, #10197, #16371, #5977, #31948, #2786, #15743, #28747, #41760, #36417, #10620, #7860, #30217, #7235, #4258, #4468, #13820, #14227, #20195, #23812, #33009, #33220, #17425, #4048, #36834, #20821, #27234, #26818, #7653, #30633, #14433 ),
 ( #29803, #30008, #33641, #26603, #17008, #30423, #23168, #39609, #847, #39826, #23602, #36623, #33847, #20610, #1270, #40249, #7443, #17221, #1477, #4675, #11042, #23384, #16801, #1057, #24026, #17633, #27442, #40457, #37042, #643, #3837, #27028, #36202, #7023, #40036, #19991, #20401, #13612, #10413, #33430, #14021, #10831, #34057, #31684, #37865, #38083, #4887 ),
 ( #21651, #17841, #14850, #2313, #28488, #28278, #15489, #34267, #41284, #25077, #2527, #11247, #24870, #34469, #21035, #41072, #18048, #34676, #8484, #5505, #8266, #28061, #27855, #8060, #2097, #15062, #40862, #11664, #37242, #18464, #21440, #1688, #11881, #24232, #5302, #8897, #24650, #1888, #30840, #8689, #21865, #37660, #18250, #14642, #27643, #18677, #5722 ),
 ( #31256, #40656, #11449, #31469, #24439, #37442, #15273, #12089, #21237, #5095, #31049, #34891, #38294, #32524, #22909, #169, #29109, #9114, #35306, #12301, #35516, #32742, #28696, #42127, #15689, #12923, #38711, #6337, #19516, #6134, #28901, #29325, #19308, #3142, #38502, #16105, #6754, #41704, #3355, #35103, #9521, #12512, #22280, #9732, #19723, #22076, #25502 ),
 ( #25914, #39132, #16322, #2937, #38922, #3575, #16536, #18889, #19097, #5927, #32106, #22700, #2734, #9318, #35730, #41496, #15900, #41916, #12716, #25706, #22488, #9938, #6541, #13139, #26131, #35942, #25290, #31897, #32312, #39778, #1219, #13347, #23973, #7812, #26337, #20560, #29547, #13771, #26768, #33170, #36154, #795, #20774, #10148, #36572, #39343, #32961 ),
 ( #29955, #1009, #10572, #33589, #7598, #23551, #14178, #7388, #36782, #4422, #3998, #3787, #23759, #13973, #16956, #16747, #10364, #26553, #27182, #17380, #20349, #33373, #36372, #30370, #36991, #4205, #40196, #10991, #591, #39559, #23335, #17169, #33798, #29752, #4626, #6971, #23118, #7188, #381, #20147, #19942, #30168, #13563, #26977, #39987, #10778, #15011 ),
 ( #38030, #8212, #40603, #17786, #37811, #5247, #37190, #25027, #28010, #18414, #30995, #30785, #21388, #21599, #37395, #1635, #5042, #2263, #24596, #14589, #40811, #41019, #21184, #8636, #27594, #18202, #17997, #4834, #8012, #34414, #20983, #11403, #34627, #11828, #24390, #34213, #27390, #1836, #14381, #5454, #41233, #31421, #31203, #40401, #14800, #30585, #11612 ),
 ( #2046, #34004, #24816, #27803, #37603, #15226, #8430, #28227, #12036, #8850, #21814, #34840, #17581, #1424, #11195, #24181, #41447, #15854, #22030, #28648, #16061, #26078, #2686, #28860, #39086, #32478, #35684, #5880, #12252, #41873, #6493, #3307, #29277, #16273, #9684, #25245, #28441, #9475, #9888, #22650, #22439, #25866, #41659, #38872, #2477, #38248, #2892 ),
 ( #9065, #13086, #3100, #19471, #19049, #18842, #35468, #122, #25461, #31846, #35262, #22861, #12672, #15643, #25661, #29063, #38458, #5674, #12467, #6291, #15438, #9276, #42083, #22234, #19262, #18631, #31636, #6086, #32270, #35059, #32054, #38668, #12877, #334, #542, #4157, #39295, #3738, #30120, #35898, #10102, #19892, #13516, #16696, #7139, #33540, #33327 ),
 ( #23495, #7341, #3527, #30323, #3949, #7552, #14131, #32693, #26924, #6709, #20096, #33120, #39510, #13300, #16910, #27133, #16487, #750, #19677, #23074, #32907, #23710, #36321, #20300, #29911, #39937, #13929, #13724, #20512, #26718, #960, #10729, #10315, #36108, #36729, #17119, #23284, #6922, #29701, #26505, #4372, #17332, #39726, #10525, #36522, #1167, #40146 ),
 ( #10939, #29493, #26287, #20936, #8171, #18367, #40356, #21555, #1376, #7764, #30741, #11779, #33961, #23928, #11566, #11151, #11361, #17953, #24346, #21345, #18159, #40768, #2218, #14547, #4790, #24138, #2003, #24551, #14334, #31374, #34371, #24769, #37353, #37146, #27757, #27967, #1590, #7968, #21139, #8591, #30954, #17741, #4995, #5204, #27556, #14965, #40563 ),
 ( #34168, #31162, #1794, #37556, #34583, #40976, #14757, #8381, #15177, #28181, #27344, #37767, #30537, #5412, #41186, #36943, #20728, #33752, #4578, #17536, #38202, #31802, #21982, #25972, #10206, #9996, #39188, #26184, #225, #22968, #21766, #7032, #22756, #26398, #37983, #19999, #35998, #9788, #6811, #9019, #29385, #15599, #8808, #3412, #16380, #29166, #12979 ),
 ( #35789, #2429, #13200, #3846, #6601, #39403, #13, #2639, #24984, #19780, #23176, #38980, #19572, #16810, #34793, #33017, #29811, #32580, #439, #25197, #32800, #41401, #31592, #3631, #15390, #12208, #16595, #29604, #35015, #5835, #5626, #18789, #18584, #13408, #36210, #11989, #28396, #10422, #36631, #13619, #36842, #34068, #30016, #30432, #17017, #14236, #40045 ),
 ( #30225, #30643, #7662, #4476, #39834, #17434, #8068, #856, #4684, #36425, #10838, #13829, #23610, #11051, #21043, #10630, #23823, #4895, #27452, #1486, #26827, #7244, #20620, #14443, #40467, #24243, #11257, #17641, #20203, #23393, #1278, #17850, #37251, #27242, #20832, #7453, #33856, #39617, #33230, #33650, #7870, #4057, #651, #40258, #26610, #20409, #33439 ) ),
 .UNSPECIFIED., .F., .F., .F.,
 ( 4, 1, 1, 1, 1, 1, 1, 1, 1, 1, 1, 1, 1, 1, 1, 1, 1, 1, 1, 1, 1, 1, 1, 1, 1, 1, 1, 1, 1, 1, 1, 1, 1, 1, 1, 1, 1, 1, 1, 1, 1, 1, 1, 1, 1, 1, 3, 4 ),
 ( 4, 1, 1, 1, 1, 1, 1, 1, 1, 1, 1, 1, 2, 1, 1, 1, 2, 1, 1, 1, 1, 1, 2, 1, 1, 1, 1, 1, 1, 1, 2, 1, 1, 1, 1, 1, 1, 1, 1, 1, 4 ),
 ( 0.000000000000000000, 0.007812500000000000000, 0.01562500000000000000, 0.02343750000000000000, 0.03125000000000000000, 0.04687500000000000000, 0.06250000000000000000, 0.07812500000000000000, 0.09375000000000000000, 0.1093750000000000000, 0.1250000000000000000, 0.1406250000000000000, 0.1562500000000000000, 0.1875000000000000000, 0.2187500000000000000, 0.2500000000000000000, 0.2812500000000000000, 0.3125000000000000000, 0.3281250000000000000, 0.3437500000000000000, 0.3750000000000000000, 0.4062500000000000000, 0.4375000000000000000, 0.4687500000000000000, 0.5000000000000000000, 0.5312500000000000000, 0.5625000000000000000, 0.5937500000000000000, 0.6250000000000000000, 0.6562500000000000000, 0.6718750000000000000, 0.6875000000000000000, 0.7187500000000000000, 0.7500000000000000000, 0.7812500000000000000, 0.8125000000000000000, 0.8437500000000000000, 0.8750000000000000000, 0.8906250000000000000, 0.9062500000000000000, 0.9218750000000000000, 0.9375000000000000000, 0.9531250000000000000, 0.9687500000000000000, 0.9765625000000000000, 0.9843750000000000000, 1.000000000000000000, 1.020397104956431988 ),
 ( 0.000000000000000000, 0.01539374999999999945, 0.03078749999999999890, 0.04618125000000002089, 0.06157499999999999779, 0.07696875000000003020, 0.09236250000000004179, 0.1077562499999999979, 0.1231499999999999956, 0.1431375000000000008, 0.1631250000000000200, 0.1831125000000000114, 0.2031000000000000028, 0.2063375000000000070, 0.2095750000000000113, 0.2128125000000000155, 0.2160500000000000198, 0.2667375000000000163, 0.3174250000000000682, 0.3681125000000000647, 0.4188000000000000611, 0.5201750000000000540, 0.6215500000000000469, 0.6266374999999999584, 0.6317250000000000920, 0.6368124999999997815, 0.6418999999999999151, 0.6469874999999999376, 0.6520749999999999602, 0.6571624999999999828, 0.6622500000000000053, 0.7044687500000000879, 0.7466875000000001705, 0.7889062500000000311, 0.8010555555555555207, 0.8311249999999998916, 0.8733437499999998632, 0.9155625000000000568, 0.9403166666666666895, 0.9577812500000000284, 1.000000000000000000 ),
 .UNSPECIFIED. ) ;
#25208 = CARTESIAN_POINT ( 'NONE',  ( -17.11529127082752666, 148.4623951536435698, 1.463161431351220676 ) ) ;
#25209 = CARTESIAN_POINT ( 'NONE',  ( -51.06239344698444427, 14.35285235637163659, -4.522483476426243598 ) ) ;
#25210 = CARTESIAN_POINT ( 'NONE',  ( 1.009415275228580322, 157.6350123088122359, -1.589207162029931952 ) ) ;
#25211 = AXIS2_PLACEMENT_3D ( 'NONE', #14059, #1304, #885 ) ;
#25212 = CARTESIAN_POINT ( 'NONE',  ( -20.70190595857163274, 149.9184980045912425, -2.291194810033231111 ) ) ;
#25213 = B_SPLINE_CURVE_WITH_KNOTS ( 'NONE', 3,
 ( #26446, #12819, #3891, #22801 ),
 .UNSPECIFIED., .F., .F.,
 ( 4, 4 ),
 ( 0.000000000000000000, 0.5643836377221552736 ),
 .UNSPECIFIED. ) ;
#25214 = CARTESIAN_POINT ( 'NONE',  ( -56.71132732703541990, 3.319205314284062958, -2.191228219141365230 ) ) ;
#25215 = CARTESIAN_POINT ( 'NONE',  ( 10.01767202841737792, 124.1433363813624311, -0.6017494237236774568 ) ) ;
#25216 = ORIENTED_EDGE ( 'NONE', *, *, #27204, .T. ) ;
#25217 = CARTESIAN_POINT ( 'NONE',  ( -16.91058881216885368, 149.6223975874448229, -2.301385465272872910 ) ) ;
#25218 = CARTESIAN_POINT ( 'NONE',  ( 1.842426711869078471, -15.45708672024491470, 5.391926158250404555 ) ) ;
#25219 = CARTESIAN_POINT ( 'NONE',  ( -4.159407845105936197, 118.2392947828752199, -0.3847720730525907018 ) ) ;
#25220 = CARTESIAN_POINT ( 'NONE',  ( -57.78858274104275949, 1.044662872677112997, -1.355440516197766732 ) ) ;
#25221 = CARTESIAN_POINT ( 'NONE',  ( -4.747830334022490106, 117.7228629901014614, 0.9149653662667899257 ) ) ;
#25222 = CARTESIAN_POINT ( 'NONE',  ( 10.89299388415055070, 123.1276765127550021, 1.556224048961160955 ) ) ;
#25223 = CARTESIAN_POINT ( 'NONE',  ( -5.525052883313952279, 65.71034362490503611, -1.269999999999993801 ) ) ;
#25224 = CIRCLE ( 'NONE', #23155, 1.905000000000000471 ) ;
#25225 = CARTESIAN_POINT ( 'NONE',  ( -6.572471397769512613, 1.803772144246908127, -5.323917895317753946 ) ) ;
#25226 = CARTESIAN_POINT ( 'NONE',  ( 9.301463764468513418, 124.2035065715909496, 0.4191708393134264687 ) ) ;
#25227 = LINE ( 'NONE', #13498, #16087 ) ;
#25229 = ORIENTED_EDGE ( 'NONE', *, *, #32944, .F. ) ;
#25228 = CARTESIAN_POINT ( 'NONE',  ( -41.90039389258884484, 22.27519970079744382, -1.481527307957015926 ) ) ;
#25230 = DIRECTION ( 'NONE',  ( 5.188838149069472160E-16, -1.699382548006136559E-16, -1.000000000000000000 ) ) ;
#25231 = CIRCLE ( 'NONE', #30671, 0.2540000000000052771 ) ;
#25232 = CARTESIAN_POINT ( 'NONE',  ( -57.95878807693440393, 1.295030275130740094, 1.504629864475967915 ) ) ;
#25233 = CARTESIAN_POINT ( 'NONE',  ( -56.50625740582004397, 4.231662007982201601, 2.501568669484166563 ) ) ;
#25234 = CARTESIAN_POINT ( 'NONE',  ( 1.364512232122848889, 118.7629491485454025, 1.251959052674563866 ) ) ;
#25235 = CARTESIAN_POINT ( 'NONE',  ( -5.177913976931283635, 53.58606249999999704, -5.372100000000000541 ) ) ;
#25236 = CARTESIAN_POINT ( 'NONE',  ( -49.25189787529244967, 18.82624764011888630, 4.709232814563275582 ) ) ;
#25237 = B_SPLINE_CURVE_WITH_KNOTS ( 'NONE', 3,
 ( #20475, #19852, #10899, #29874, #27095, #32866 ),
 .UNSPECIFIED., .F., .F.,
 ( 4, 2, 4 ),
 ( 0.000000000000000000, 0.5000000000000000000, 1.000000000000000000 ),
 .UNSPECIFIED. ) ;
#25238 = CARTESIAN_POINT ( 'NONE',  ( -23.32536756748188012, 149.0517038676186417, -0.2354165988066208859 ) ) ;
#25239 = ORIENTED_EDGE ( 'NONE', *, *, #10766, .F. ) ;
#25240 = CARTESIAN_POINT ( 'NONE',  ( -50.06058399760020450, 19.37794936593257589, -3.106418048087412842 ) ) ;
#25241 = CARTESIAN_POINT ( 'NONE',  ( -6.958142857130818371, 121.9433530685592046, -0.2545489040402749703 ) ) ;
#25242 = CARTESIAN_POINT ( 'NONE',  ( 4.801338745653756845, 117.3993836138989906, -1.016148446936214977 ) ) ;
#25243 = ORIENTED_EDGE ( 'NONE', *, *, #36259, .T. ) ;
#25244 = CARTESIAN_POINT ( 'NONE',  ( 2.432624640667874427, 115.7029433324280916, -1.605953286633470700 ) ) ;
#25245 = CARTESIAN_POINT ( 'NONE',  ( -14.68908181661163148, 148.8396455022467535, -0.5202010721049650233 ) ) ;
#25246 = CARTESIAN_POINT ( 'NONE',  ( 3.566861488287894844, -14.88765406650577283, 5.398167181214303945 ) ) ;
#25247 = CARTESIAN_POINT ( 'NONE',  ( -21.30706188252199595, 149.4807732621110006, 1.383641861344255153 ) ) ;
#25248 = DIRECTION ( 'NONE',  ( -0.7770581983690896255, 0.6294287539883960392, 1.268759650262045389E-15 ) ) ;
#25249 = CARTESIAN_POINT ( 'NONE',  ( 10.79372094067536736, 157.9251727141802633, 0.3940533352873709094 ) ) ;
#25250 = CARTESIAN_POINT ( 'NONE',  ( 8.708480741344933662, 123.6715853908191605, 0.2610670616659550025 ) ) ;
#25251 = CARTESIAN_POINT ( 'NONE',  ( -0.8615061033338488050, 12.60145565637890286, -0.4637196408544374537 ) ) ;
#25252 = CARTESIAN_POINT ( 'NONE',  ( -2.743358099589880972, 116.5337465564440578, -0.09497135926289690389 ) ) ;
#25253 = DIRECTION ( 'NONE',  ( -0.8745520943968247973, 0.4849315768086537304, -5.361993529360573944E-16 ) ) ;
#25254 = CARTESIAN_POINT ( 'NONE',  ( -6.657354853833413522, 117.1094500233132152, -0.1330297985976032216 ) ) ;
#25255 = ORIENTED_EDGE ( 'NONE', *, *, #23212, .T. ) ;
#25256 = CARTESIAN_POINT ( 'NONE',  ( 5.574731289855488825, 117.5669237741502542, 0.9295890844387997287 ) ) ;
#25257 = CARTESIAN_POINT ( 'NONE',  ( -2.587970193024280441, -12.16632112844677494, -3.833404006186521773 ) ) ;
#25258 = CARTESIAN_POINT ( 'NONE',  ( 21.23477820244536218, 149.4807732621110006, 2.233729070194449662 ) ) ;
#25259 = CARTESIAN_POINT ( 'NONE',  ( 1.172281656590494325, 158.5855360310326319, -1.517099175104413611 ) ) ;
#25260 = CARTESIAN_POINT ( 'NONE',  ( 3.683590692373001296, 21.29142263786511080, 7.571256661570916258 ) ) ;
#25261 = CARTESIAN_POINT ( 'NONE',  ( -22.31562366552510213, 146.3189071340513294, -1.902122558187540058 ) ) ;
#25262 = CARTESIAN_POINT ( 'NONE',  ( 4.819985158455081020, 117.7659792149047888, -0.8434561934874992284 ) ) ;
#25263 = CIRCLE ( 'NONE', #6899, 0.2540000000000000591 ) ;
#25264 = B_SPLINE_CURVE_WITH_KNOTS ( 'NONE', 3,
 ( #4056, #1277, #16594, #26826, #17433, #39402, #14030, #26397, #14235, #39833, #6810, #33438, #27241, #19998, #33229, #13828, #23822, #10421, #4265, #3630, #30015, #35997, #20202, #855, #10629, #23609, #36630, #10205, #23392, #17228, #438, #7661, #13407, #33016, #36209, #3845, #36424, #1063, #27035, #16809, #19779, #40044, #36841, #20619, #7243, #29810, #13618, #26609, #33649, #9995, #4475, #22967, #32799, #11256, #18260, #34685 ),
 .UNSPECIFIED., .F., .F.,
 ( 4, 2, 2, 2, 2, 1, 2, 2, 2, 2, 2, 2, 1, 2, 2, 2, 2, 2, 1, 1, 2, 2, 2, 2, 1, 1, 2, 2, 2, 2, 4 ),
 ( 0.000000000000000000, 0.06250000000003663736, 0.1250000000000732747, 0.1875000000001099121, 0.2187500000001282863, 0.2343750000001399991, 0.2421875000001458555, 0.2500000000001517120, 0.3750000000002494671, 0.4375000000002982614, 0.4687500000003190226, 0.4843750000003258505, 0.4921875000003256284, 0.4960937500003254064, 0.5000000000003251843, 0.6250000000001366685, 0.6875000000000456302, 0.7187500000000000000, 0.7343749999999770184, 0.7421874999999621414, 0.7460937499999581446, 0.7499999999999542588, 0.8124999999999031886, 0.8437499999998805400, 0.8593749999998692157, 0.8671874999998636646, 0.8710937499998608891, 0.8749999999998582245, 0.9374999999999291678, 0.9687499999999645839, 1.000000000000000000 ),
 .UNSPECIFIED. ) ;
#25265 = CARTESIAN_POINT ( 'NONE',  ( 6.114402651314309267, 119.5149100643186983, 0.5171552335003601897 ) ) ;
#25266 = CARTESIAN_POINT ( 'NONE',  ( -15.77201034003361890, 145.9134097338176730, -0.1865891569459577071 ) ) ;
#25267 = CARTESIAN_POINT ( 'NONE',  ( -12.16261443152851562, 122.9664497093790629, -1.797897170200384753 ) ) ;
#25268 = CARTESIAN_POINT ( 'NONE',  ( 2.285161673027230389, -15.58026522864758334, 5.856586201423784388 ) ) ;
#25269 = CARTESIAN_POINT ( 'NONE',  ( -2.032601633563780229E-14, 30.83083951148100255, -1.904999999999999805 ) ) ;
#25270 = CARTESIAN_POINT ( 'NONE',  ( -2.756659151272291552, 117.3993815979357578, -1.414639205003844991 ) ) ;
#25271 = ORIENTED_EDGE ( 'NONE', *, *, #17876, .T. ) ;
#25272 = CARTESIAN_POINT ( 'NONE',  ( 17.07725563869803054, 135.3907879583883869, 2.389267674572352895 ) ) ;
#25273 = AXIS2_PLACEMENT_3D ( 'NONE', #30526, #30732, #20502 ) ;
#25274 = CARTESIAN_POINT ( 'NONE',  ( 0.01793833495430298061, 118.1627382089642566, -0.8977079103094813828 ) ) ;
#25275 = CARTESIAN_POINT ( 'NONE',  ( -0.1450076288961997528, 106.1446358501009826, 5.226538226828138178 ) ) ;
#25276 = CARTESIAN_POINT ( 'NONE',  ( -6.970347610136101046, -0.07026165769430378627, 4.770677917868129114 ) ) ;
#25277 = CARTESIAN_POINT ( 'NONE',  ( 6.480921187770015912, 121.5572409441427482, 0.5803991303062127072 ) ) ;
#25278 = CARTESIAN_POINT ( 'NONE',  ( 0.005431400947610381079, 116.8580640273661118, -0.2718095133625907933 ) ) ;
#25279 = CARTESIAN_POINT ( 'NONE',  ( 5.860205464924936436, 57.15000000000087255, -5.019550311879306115 ) ) ;
#25280 = CIRCLE ( 'NONE', #27323, 6.349999999999999645 ) ;
#25281 = CARTESIAN_POINT ( 'NONE',  ( -58.34772544449950971, -0.2453081154814788778, 0.1850187449336859469 ) ) ;
#25282 = DIRECTION ( 'NONE',  ( -0.9998004120163609398, 0.000000000000000000, -0.01997839162482749689 ) ) ;
#25283 = AXIS2_PLACEMENT_3D ( 'NONE', #22849, #35889, #6912 ) ;
#25284 = AXIS2_PLACEMENT_3D ( 'NONE', #395, #38725, #19112 ) ;
#25285 = CARTESIAN_POINT ( 'NONE',  ( -5.941750549330245157, 56.51500000000488200, 5.016499812855502505 ) ) ;
#25286 = CARTESIAN_POINT ( 'NONE',  ( -23.11127252101368867, 149.9001116002701224, -0.4618182267416073850 ) ) ;
#25287 = ORIENTED_EDGE ( 'NONE', *, *, #34464, .T. ) ;
#25288 = CARTESIAN_POINT ( 'NONE',  ( 8.270623378294651218, 120.3814744154732068, -1.107964214892792398 ) ) ;
#25289 = CARTESIAN_POINT ( 'NONE',  ( -17.14499999999999957, 71.11999999999999034, -5.016499999999999737 ) ) ;
#25290 = CARTESIAN_POINT ( 'NONE',  ( -15.86281397719570307, 145.7686330500600036, -0.9137093302325696165 ) ) ;
#25291 = CARTESIAN_POINT ( 'NONE',  ( -28.94717034978515713, 63.96727089252595988, 1.523999999999992916 ) ) ;
#25292 = CARTESIAN_POINT ( 'NONE',  ( 22.83504831576691529, 150.4065277667444036, 0.4818782557684029300 ) ) ;
#25293 = EDGE_CURVE ( 'NONE', #39680, #32786, #26836, .T. ) ;
#25294 = ORIENTED_EDGE ( 'NONE', *, *, #7649, .F. ) ;
#25295 = CARTESIAN_POINT ( 'NONE',  ( -3.453265078539333288, 21.00871511114837276, -3.102408547967784092 ) ) ;
#25296 = CARTESIAN_POINT ( 'NONE',  ( -29.24370919332844210, 62.65993627038479019, 1.523999999999994470 ) ) ;
#25297 = CARTESIAN_POINT ( 'NONE',  ( -7.784012322544769269, 122.6313477034873074, -0.1555430911242075831 ) ) ;
#25298 = CARTESIAN_POINT ( 'NONE',  ( -41.34781391884743584, 22.78346824045823737, 1.529410470707965208 ) ) ;
#25299 = CARTESIAN_POINT ( 'NONE',  ( -3.682264917456323339, 78.32546620154573702, -0.07358041635423968885 ) ) ;
#25300 = CARTESIAN_POINT ( 'NONE',  ( -6.992289727212193107, 121.9234231950531040, 0.03108638981060581064 ) ) ;
#25301 = CARTESIAN_POINT ( 'NONE',  ( -1.512449008193210931, 25.81601926892489018, -4.382106060783010903 ) ) ;
#25302 = CARTESIAN_POINT ( 'NONE',  ( -0.01289612358334866170, 159.5048567107479585, 0.6453747585945883714 ) ) ;
#25303 = CARTESIAN_POINT ( 'NONE',  ( 4.546605812636178356, 104.6144662015457101, -1.650915952755167782 ) ) ;
#25305 = CARTESIAN_POINT ( 'NONE',  ( 19.98084523315760208, 136.1824594150436383, -1.423751267309647517 ) ) ;
#25304 = DIRECTION ( 'NONE',  ( -0.8138664877804109299, 0.5810519254489895369, 0.000000000000000000 ) ) ;
#25306 = CARTESIAN_POINT ( 'NONE',  ( -11.23500844718025782, 122.9575399027323073, 1.191779604289733507 ) ) ;
#25307 = CARTESIAN_POINT ( 'NONE',  ( 0.1402366131884419942, -14.11417690215759713, -0.9622292808001302600 ) ) ;
#25308 = CARTESIAN_POINT ( 'NONE',  ( -22.78320035282278866, 142.4248215231809240, -1.435786487410106282 ) ) ;
#25309 = CARTESIAN_POINT ( 'NONE',  ( -0.8250140797137134330, 8.550980984719981137, 0.5181985368706800710 ) ) ;
#25310 = VERTEX_POINT ( 'NONE', #35307 ) ;
#25311 = EDGE_CURVE ( 'NONE', #26988, #20298, #14470, .T. ) ;
#25312 = CARTESIAN_POINT ( 'NONE',  ( -54.22787649382025421, 6.886497292746610377, -9.139123573059997208E-15 ) ) ;
#25313 = CARTESIAN_POINT ( 'NONE',  ( -10.62256650593141138, 126.1357510980948575, 0.2607537273017401791 ) ) ;
#25314 = CARTESIAN_POINT ( 'NONE',  ( 5.906500239725072987, -12.19293670846725774, 0.5532178544325924152 ) ) ;
#25315 = CARTESIAN_POINT ( 'NONE',  ( 14.77909737591000905, 150.5114039713088516, -1.257293140667800957 ) ) ;
#25316 = CARTESIAN_POINT ( 'NONE',  ( 0.3620310593072569860, 115.7033445315342561, 1.764050944526450726 ) ) ;
#25317 = AXIS2_PLACEMENT_3D ( 'NONE', #26230, #3251, #19830 ) ;
#25318 = CARTESIAN_POINT ( 'NONE',  ( -4.845260018671773139, 117.7536946542396521, -0.9519537261478631107 ) ) ;
#25319 = CARTESIAN_POINT ( 'NONE',  ( 14.17939111974011546, 138.8817910697950140, 0.2325274008182655339 ) ) ;
#25320 = ORIENTED_EDGE ( 'NONE', *, *, #36240, .T. ) ;
#25321 = EDGE_CURVE ( 'NONE', #21896, #3203, #251, .T. ) ;
#25322 = CARTESIAN_POINT ( 'NONE',  ( 20.08651816730950657, 147.5185649274072830, 2.508444087122727595 ) ) ;
#25323 = CARTESIAN_POINT ( 'NONE',  ( 11.83539255247743149, 152.0195595274622349, 0.2364993098673506822 ) ) ;
#25324 = CARTESIAN_POINT ( 'NONE',  ( -6.096105168583893358E-14, 97.88346620154572975, 1.046006720343116589E-16 ) ) ;
#25325 = ADVANCED_FACE ( 'NONE', ( #22490 ), #41720, .T. ) ;
#25326 = CARTESIAN_POINT ( 'NONE',  ( -3.682264917456324671, 104.6144662015457243, -0.07358041635423968885 ) ) ;
#25327 = TOROIDAL_SURFACE ( 'NONE', #34884, 3.683000000000000718, 0.5080000000000000071 ) ;
#25328 = CARTESIAN_POINT ( 'NONE',  ( 20.63094779205695417, 152.5829384802601396, -0.02634999427677312683 ) ) ;
#25329 = EDGE_CURVE ( 'NONE', #25936, #31634, #41636, .T. ) ;
#25330 = DIRECTION ( 'NONE',  ( 4.017660918040594346E-17, -1.000000000000000000, -2.376309959284832031E-19 ) ) ;
#25331 = CARTESIAN_POINT ( 'NONE',  ( -46.87366875892457330, 25.48678770706554175, 1.642247700512937669 ) ) ;
#25332 = DIRECTION ( 'NONE',  ( -0.3213437296502708040, 0.9469626219732506511, -9.578090222180217247E-17 ) ) ;
#25333 = EDGE_CURVE ( 'NONE', #41136, #19839, #31898, .T. ) ;
#25334 = CARTESIAN_POINT ( 'NONE',  ( 1.665918867370522083, -15.28033259084871176, 5.729025533920835578 ) ) ;
#25335 = CARTESIAN_POINT ( 'NONE',  ( -46.82679756180435504, 21.08486709759267086, 4.907624977305271585 ) ) ;
#25336 = DIRECTION ( 'NONE',  ( 0.9998004120163609398, 4.016384292689130894E-17, 0.01997839162482749689 ) ) ;
#25337 = B_SPLINE_CURVE_WITH_KNOTS ( 'NONE', 3,
 ( #6107, #144, #23095, #19070, #22882, #32077, #38689 ),
 .UNSPECIFIED., .F., .F.,
 ( 4, 1, 1, 1, 4 ),
 ( 0.6462721360804335458, 0.7047636632187934680, 0.8031757754791957193, 0.9015878877395978597, 1.000000000000000000 ),
 .UNSPECIFIED. ) ;
#25338 = CARTESIAN_POINT ( 'NONE',  ( -4.577798419110891359, 118.0358839641028084, 0.6746410181898425673 ) ) ;
#25339 = ORIENTED_EDGE ( 'NONE', *, *, #18294, .F. ) ;
#25340 = DIRECTION ( 'NONE',  ( -5.188838149069472160E-16, 1.699382548006136559E-16, 1.000000000000000000 ) ) ;
#25341 = CARTESIAN_POINT ( 'NONE',  ( 5.892261121993457529, 118.9652010781061620, -1.019900290652594688 ) ) ;
#25342 = CARTESIAN_POINT ( 'NONE',  ( -4.672526732406542926, 120.2198808273567892, -0.4623614190293560688 ) ) ;
#25343 = CARTESIAN_POINT ( 'NONE',  ( 4.624176940134817393, 117.9598222893437054, 0.9309007159876104831 ) ) ;
#25344 = DIRECTION ( 'NONE',  ( -5.206863593109713661E-17, 1.000000000000000000, -1.077750396879097183E-30 ) ) ;
#25345 = CARTESIAN_POINT ( 'NONE',  ( -0.3809694336149819782, 120.1716774721349168, 0.6201936767135832751 ) ) ;
#25346 = AXIS2_PLACEMENT_3D ( 'NONE', #19891, #22860, #23494 ) ;
#25347 = CARTESIAN_POINT ( 'NONE',  ( -4.476207883417873568, -7.053342675672244155, -1.178223045331058705 ) ) ;
#25348 = DIRECTION ( 'NONE',  ( -5.188838149069471174E-16, 1.699382548006136313E-16, 1.000000000000000000 ) ) ;
#25349 = CARTESIAN_POINT ( 'NONE',  ( 17.14499999999999957, 71.11999999999999034, 5.016499999999999737 ) ) ;
#25350 = CARTESIAN_POINT ( 'NONE',  ( 0.1065646865914872399, 105.8844662015456777, -5.332932678536313809 ) ) ;
#25351 = CARTESIAN_POINT ( 'NONE',  ( -16.32868586224187624, 149.3997711511537148, -2.122341471705226912 ) ) ;
#25352 = CARTESIAN_POINT ( 'NONE',  ( -6.068057099051500813, 121.4371919376452524, -0.1208108290503153576 ) ) ;
#25353 = CARTESIAN_POINT ( 'NONE',  ( -5.712646857600669037, 30.64406086319245404, 3.136461800983552983 ) ) ;
#25354 = DIRECTION ( 'NONE',  ( -1.000000000000000000, 0.000000000000000000, 0.000000000000000000 ) ) ;
#25355 = CARTESIAN_POINT ( 'NONE',  ( 4.573446973487649281, 17.56025517495590904, -0.6989348988664985107 ) ) ;
#25357 = ORIENTED_EDGE ( 'NONE', *, *, #38817, .T. ) ;
#25356 = CARTESIAN_POINT ( 'NONE',  ( 1.385657586283472797, 159.5796833544862352, 0.3718886678235075460 ) ) ;
#25358 = CARTESIAN_POINT ( 'NONE',  ( 2.260647411234051773, 105.1243225396854797, -4.832372919530040001 ) ) ;
#25359 = CARTESIAN_POINT ( 'NONE',  ( 3.525547644170144324, -15.07001638954266731, 1.996499786560847367 ) ) ;
#25360 = CARTESIAN_POINT ( 'NONE',  ( -1.064682733364023193, 157.9544661020348997, 1.608744340525368077 ) ) ;
#25361 = CARTESIAN_POINT ( 'NONE',  ( -0.7860673829865619799, 16.32342451650498916, -0.5763570944834206511 ) ) ;
#25362 = TOROIDAL_SURFACE ( 'NONE', #39661, 0.3809999999999999498, 0.2540000000000000036 ) ;
#25363 = CARTESIAN_POINT ( 'NONE',  ( -0.9756160567605162148, 3.744600508531710226, -0.009113680661486545098 ) ) ;
#25364 = VERTEX_POINT ( 'NONE', #12925 ) ;
#25365 = ORIENTED_EDGE ( 'NONE', *, *, #41005, .F. ) ;
#25366 = FACE_OUTER_BOUND ( 'NONE', #29370, .T. ) ;
#25367 = CARTESIAN_POINT ( 'NONE',  ( 6.804471202056719292, 123.7298400107579255, 0.1732695889264301847 ) ) ;
#25368 =( NAMED_UNIT ( * ) PLANE_ANGLE_UNIT ( ) SI_UNIT ( $, .RADIAN. ) );
#25369 = CARTESIAN_POINT ( 'NONE',  ( -9.105332701317941257, 123.1184971541203055, 0.5608273726695749417 ) ) ;
#25370 = CARTESIAN_POINT ( 'NONE',  ( -15.70103477329412911, 145.5797129992483292, -0.3137440411564564879 ) ) ;
#25371 = CARTESIAN_POINT ( 'NONE',  ( 3.292060170515798578, -12.34027101600769427, 0.7492661515550719242 ) ) ;
#25372 = CARTESIAN_POINT ( 'NONE',  ( 17.40456409200965382, 148.7932787949812905, -1.578286399122462713 ) ) ;
#25373 = CARTESIAN_POINT ( 'NONE',  ( -19.98568676637960095, 149.3093937917295762, -2.465107550769984446 ) ) ;
#25374 = DIRECTION ( 'NONE',  ( -0.000000000000000000, -0.000000000000000000, -1.000000000000000000 ) ) ;
#25375 = CARTESIAN_POINT ( 'NONE',  ( 8.547710372622628228, 118.8041091126597593, 1.212475388694229217 ) ) ;
#25376 = DIRECTION ( 'NONE',  ( -0.2290273297124504059, 0.9734199927291325993, 0.000000000000000000 ) ) ;
#25377 = CARTESIAN_POINT ( 'NONE',  ( 12.13843755257572354, 130.5412724693565849, -0.1686832038582289639 ) ) ;
#25378 = EDGE_CURVE ( 'NONE', #29332, #32282, #14533, .T. ) ;
#25379 = EDGE_LOOP ( 'NONE', ( #26860, #3692 ) ) ;
#25380 = CARTESIAN_POINT ( 'NONE',  ( 0.1066493941971741466, 105.7853621660184871, -5.332931186019222558 ) ) ;
#25381 = CARTESIAN_POINT ( 'NONE',  ( -25.80936006922821591, 73.72935646344811289, -1.270000000000005791 ) ) ;
#25382 = EDGE_CURVE ( 'NONE', #38342, #2334, #37999, .T. ) ;
#25383 = MECHANICAL_DESIGN_GEOMETRIC_PRESENTATION_REPRESENTATION (  '', ( #11115 ), #38309 ) ;
#25384 = CARTESIAN_POINT ( 'NONE',  ( 4.986734588179421834, 117.3993830463062835, 0.9017165445866112128 ) ) ;
#25385 = AXIS2_PLACEMENT_3D ( 'NONE', #21093, #27087, #14086 ) ;
#25386 = CARTESIAN_POINT ( 'NONE',  ( -13.70915846191426013, 16.90875728684043366, 5.016499999999999737 ) ) ;
#25387 = CARTESIAN_POINT ( 'NONE',  ( 7.043328640077428204, 23.89357186360551566, -4.653114003055315528 ) ) ;
#25388 = CARTESIAN_POINT ( 'NONE',  ( 7.189601074672208547, 121.4526873951801633, 0.9441605179235380563 ) ) ;
#25389 = DIRECTION ( 'NONE',  ( 0.9998004120163609398, 5.205824365704083189E-17, 0.01997839162482749689 ) ) ;
#25390 = CARTESIAN_POINT ( 'NONE',  ( 22.66420477949313650, 150.6410255081855212, 0.3761569768119879531 ) ) ;
#25391 = ADVANCED_FACE ( 'NONE', ( #38503 ), #33521, .T. ) ;
#25392 = CARTESIAN_POINT ( 'NONE',  ( -5.282628607152124012, 116.7267603939287426, 0.8077565746219078635 ) ) ;
#25393 = AXIS2_PLACEMENT_3D ( 'NONE', #24425, #40850, #5290 ) ;
#25394 = EDGE_CURVE ( 'NONE', #41701, #26282, #15204, .T. ) ;
#25395 = CARTESIAN_POINT ( 'NONE',  ( 2.294499597581835193, -9.852027417895397932, -4.012603411698490774 ) ) ;
#25396 = CARTESIAN_POINT ( 'NONE',  ( 7.044606587285096033, 122.0729346620515088, 0.1407680048458705979 ) ) ;
#25397 = CARTESIAN_POINT ( 'NONE',  ( 13.99112315924537420, 122.1591959312462592, 1.692395687056787557 ) ) ;
#25398 = CARTESIAN_POINT ( 'NONE',  ( -8.048466033148526932, -0.5260294302935444311, 2.538140512261041426 ) ) ;
#25399 = CARTESIAN_POINT ( 'NONE',  ( 8.727022611403114638, 118.0966510066766375, -0.5008853566498474574 ) ) ;
#25400 = CARTESIAN_POINT ( 'NONE',  ( -0.3568539549766963637, 120.5507043431651510, -0.5637235919965007946 ) ) ;
#25401 = CARTESIAN_POINT ( 'NONE',  ( -5.586884702347496123, 100.6774662015457409, -0.1116392523995361624 ) ) ;
#25402 = EDGE_CURVE ( 'NONE', #37685, #4530, #39518, .T. ) ;
#25403 = CARTESIAN_POINT ( 'NONE',  ( -30.20416046766210272, 71.17241488000101413, -1.270000000000007345 ) ) ;
#25404 = CARTESIAN_POINT ( 'NONE',  ( -5.875566536072981627, -5.528788512802195854, 6.048791003748659634 ) ) ;
#25405 = CARTESIAN_POINT ( 'NONE',  ( 2.553797193193295012, 117.3993834737731845, 1.425018694576543510 ) ) ;
#25406 = LINE ( 'NONE', #12198, #31425 ) ;
#25407 = CARTESIAN_POINT ( 'NONE',  ( 3.150244473240279675, -14.07033042043420146, 1.813758411523331393 ) ) ;
#25408 = CARTESIAN_POINT ( 'NONE',  ( 0.7355314204967891012, 116.0160817474902331, -1.626749668116675096 ) ) ;
#25409 = CARTESIAN_POINT ( 'NONE',  ( -6.917230302149087962, 117.3903047926647787, 0.3126493885886561519 ) ) ;
#25410 = ORIENTED_EDGE ( 'NONE', *, *, #22899, .T. ) ;
#25411 = DIRECTION ( 'NONE',  ( -0.9816537812491089587, -0.1906721105965065444, -4.769617732184475162E-16 ) ) ;
#25412 = VERTEX_POINT ( 'NONE', #30171 ) ;
#25413 = DIRECTION ( 'NONE',  ( -0.8745520943968243532, 0.4849315768086547296, -6.829619984160642269E-16 ) ) ;
#25414 = CONICAL_SURFACE ( 'NONE', #11632, 1.905000000000007354, 0.7853981633974428389 ) ;
#25415 = CARTESIAN_POINT ( 'NONE',  ( 2.845652327410156612, -15.51977306057959716, 5.689769116265302351 ) ) ;
#25416 = CARTESIAN_POINT ( 'NONE',  ( -20.75082247216797171, 147.7542213611591535, 1.617965925928342097 ) ) ;
#25417 = CARTESIAN_POINT ( 'NONE',  ( 5.352805660278670885, 158.9031408473208273, -0.9771030980504659125 ) ) ;
#25418 = CARTESIAN_POINT ( 'NONE',  ( -0.2480930319908794535, 10.21371511114847053, -4.635561276548324727 ) ) ;
#25419 = CARTESIAN_POINT ( 'NONE',  ( -58.40556995236380544, 0.1837532267470638192, -0.8520485832066984067 ) ) ;
#25420 = CONICAL_SURFACE ( 'NONE', #22643, 13.46199999999999619, 0.7853981633974497223 ) ;
#25421 = ORIENTED_EDGE ( 'NONE', *, *, #13992, .F. ) ;
#25422 = CARTESIAN_POINT ( 'NONE',  ( -0.0006472084743731488631, 124.6436471961814476, 0.03238895860161147139 ) ) ;
#25423 = DIRECTION ( 'NONE',  ( 5.188838149069472160E-16, -1.699382548006136559E-16, -1.000000000000000000 ) ) ;
#25424 = CARTESIAN_POINT ( 'NONE',  ( -11.42483690514971251, 124.5424752485109963, 1.054873134768184118 ) ) ;
#25425 = DIRECTION ( 'NONE',  ( -0.8745520943968225769, 0.4849315768086578382, -5.691349986800571545E-16 ) ) ;
#25426 = CARTESIAN_POINT ( 'NONE',  ( 13.18164045127527473, 153.9517556018257096, -1.734949727869875780 ) ) ;
#25427 = CARTESIAN_POINT ( 'NONE',  ( -13.99112315924550387, 122.1591959312462592, -1.692395687056787557 ) ) ;
#25428 = CARTESIAN_POINT ( 'NONE',  ( -50.29507671575587580, 15.72791930032350827, -4.796563717952114558 ) ) ;
#25429 = CIRCLE ( 'NONE', #16561, 0.2540000000000000036 ) ;
#25430 = CARTESIAN_POINT ( 'NONE',  ( 15.65625195688299520, 148.1291547725267037, -0.6483782694814674841 ) ) ;
#25431 = ORIENTED_EDGE ( 'NONE', *, *, #31589, .T. ) ;
#25432 = CARTESIAN_POINT ( 'NONE',  ( -16.90821003499447528, 140.1729163700083518, -2.280195664865559468 ) ) ;
#25433 = CARTESIAN_POINT ( 'NONE',  ( 3.506097670019660217, -15.11506922876175452, 2.387495833752258267 ) ) ;
#25434 = CIRCLE ( 'NONE', #35657, 0.7620000000000030083 ) ;
#25435 = CARTESIAN_POINT ( 'NONE',  ( -4.226413698654440054, 118.2242417877410077, -0.4878142890945914023 ) ) ;
#25436 = CARTESIAN_POINT ( 'NONE',  ( -5.861642722916909243, 64.54502714855203749, 1.524000000000005572 ) ) ;
#25437 = CARTESIAN_POINT ( 'NONE',  ( -4.794585119801084261, 117.6364790366381214, 0.9472855824390624679 ) ) ;
#25438 = CARTESIAN_POINT ( 'NONE',  ( 10.97746297113248204, 123.2082810311540300, 1.564610664257709116 ) ) ;
#25439 = DIRECTION ( 'NONE',  ( -5.188838149069471174E-16, 1.699382548006136313E-16, 1.000000000000000000 ) ) ;
#25440 = VECTOR ( 'NONE', #15441, 1000.000000000000114 ) ;
#25441 = EDGE_CURVE ( 'NONE', #38260, #29270, #34911, .T. ) ;
#25442 = CARTESIAN_POINT ( 'NONE',  ( 4.537321141924904211, 26.63107350737006840, 0.8823464973398146283 ) ) ;
#25443 = CARTESIAN_POINT ( 'NONE',  ( 0.6320571215039689772, 120.9405031987692212, 0.1040377489725132221 ) ) ;
#25444 = CARTESIAN_POINT ( 'NONE',  ( 3.682264917456193221, 71.97546620154574271, 0.07358041635424013294 ) ) ;
#25445 = EDGE_CURVE ( 'NONE', #4283, #29150, #24061, .T. ) ;
#25446 = CARTESIAN_POINT ( 'NONE',  ( -47.44699234454015624, 15.94620872345377904, -0.4021177788561511313 ) ) ;
#25447 = CARTESIAN_POINT ( 'NONE',  ( -0.3675782062531062766, 118.1588899765148000, 0.8952817763280002117 ) ) ;
#25448 = CARTESIAN_POINT ( 'NONE',  ( -57.66338803320029882, 2.692357263605615891, 1.869785753600835987 ) ) ;
#25449 = CARTESIAN_POINT ( 'NONE',  ( -53.62923018145963283, 9.955465683803918608, 3.869326235999875241 ) ) ;
#25450 = CARTESIAN_POINT ( 'NONE',  ( -29.63955751525485383, 69.20430988267358430, -1.524000000000006905 ) ) ;
#25451 = AXIS2_PLACEMENT_3D ( 'NONE', #27066, #17047, #4716 ) ;
#25452 = CARTESIAN_POINT ( 'NONE',  ( -5.475330206976867231, 53.58606249999999704, -5.107412922131463695 ) ) ;
#25453 = CARTESIAN_POINT ( 'NONE',  ( -53.65397596840620764, 15.31786685697163897, 0.6615342354323947571 ) ) ;
#25454 = CARTESIAN_POINT ( 'NONE',  ( -22.59814275696104957, 137.2245694613254443, -0.1355511068837782773 ) ) ;
#25455 = ORIENTED_EDGE ( 'NONE', *, *, #37587, .T. ) ;
#25456 = CARTESIAN_POINT ( 'NONE',  ( -50.64083584635693569, 22.17031203569813513, -1.070075483901071409E-14 ) ) ;
#25457 = CARTESIAN_POINT ( 'NONE',  ( 6.923717762196975656, 121.8542084741468727, -0.1949843968422386720 ) ) ;
#25458 = CARTESIAN_POINT ( 'NONE',  ( 4.976602257458158540, 117.4065341493209331, -0.8843054372351270009 ) ) ;
#25459 = ORIENTED_EDGE ( 'NONE', *, *, #25098, .F. ) ;
#25460 = CARTESIAN_POINT ( 'NONE',  ( 1.821088186378801099, 115.7029441851158680, -1.652984706171152673 ) ) ;
#25462 = AXIS2_PLACEMENT_3D ( 'NONE', #39370, #20375, #37017 ) ;
#25461 = CARTESIAN_POINT ( 'NONE',  ( -6.494557633019148568, 121.7745328324513139, -0.2023806202038006818 ) ) ;
#25463 = CARTESIAN_POINT ( 'NONE',  ( 4.383797612528895549, -14.46967269938057044, 4.720428574551663203 ) ) ;
#25464 = CARTESIAN_POINT ( 'NONE',  ( -18.02024205669876622, 128.5942011134444272, 1.207605415130186710 ) ) ;
#25465 = CARTESIAN_POINT ( 'NONE',  ( 5.767947771861689610, 78.89823565723094134, -5.032924692340810857 ) ) ;
#25466 = CARTESIAN_POINT ( 'NONE',  ( 22.49140923449501273, 150.7830971219523519, 0.7772193431698347643 ) ) ;
#25467 = CARTESIAN_POINT ( 'NONE',  ( 1.628970766729582964, 120.9961522207271969, 0.09962698007392074839 ) ) ;
#25468 = DIRECTION ( 'NONE',  ( 2.664535259100375303E-15, 0.000000000000000000, 1.000000000000000000 ) ) ;
#25469 = CARTESIAN_POINT ( 'NONE',  ( 0.9752960398044887569, 8.493769703755262412, 0.04006526980912952091 ) ) ;
#25470 = CARTESIAN_POINT ( 'NONE',  ( -23.40402153822892828, 142.8142681763856388, -0.5431523703306524453 ) ) ;
#25471 = FACE_OUTER_BOUND ( 'NONE', #26664, .T. ) ;
#25472 = DIRECTION ( 'NONE',  ( -9.627370216492862708E-17, -1.000000000000000000, 0.000000000000000000 ) ) ;
#25473 = ORIENTED_EDGE ( 'NONE', *, *, #4045, .T. ) ;
#25474 = CARTESIAN_POINT ( 'NONE',  ( -2.409930537596374212, 116.5911498892034786, 0.3318507686391455880 ) ) ;
#25475 = CARTESIAN_POINT ( 'NONE',  ( -58.35793580214877352, -0.2667336269367078794, -0.1357860315391856976 ) ) ;
#25476 = CARTESIAN_POINT ( 'NONE',  ( 13.69970117413521393, 155.7522398296385404, 1.951476099255863739 ) ) ;
#25477 = CARTESIAN_POINT ( 'NONE',  ( 1.222221009663079672, 118.4063602595805946, -0.6323148984906140635 ) ) ;
#25478 = CIRCLE ( 'NONE', #15899, 14.73199999999999577 ) ;
#25479 = CARTESIAN_POINT ( 'NONE',  ( 8.395564333921381461, 13.51935342844394583, -0.6424836208785561498 ) ) ;
#25480 = CARTESIAN_POINT ( 'NONE',  ( -7.998778050759740132, 118.2752802814886053, -1.041156008592528437 ) ) ;
#25481 = CARTESIAN_POINT ( 'NONE',  ( 4.711505574849351063, 117.9616044365023271, -0.6920222299632273755 ) ) ;
#25482 = CARTESIAN_POINT ( 'NONE',  ( -0.1065646865916381608, 105.8844662015456777, 5.332932678536313809 ) ) ;
#25483 = CARTESIAN_POINT ( 'NONE',  ( -4.580760836099313948, 121.1907927009877000, -0.02326454623414934281 ) ) ;
#25484 = CARTESIAN_POINT ( 'NONE',  ( 0.03245814172805025488, 157.7902383798253538, -1.624338139048501439 ) ) ;
#25485 = CARTESIAN_POINT ( 'NONE',  ( 5.890162669548780094, -14.87046963210582362, 1.285284309844398898 ) ) ;
#25486 = CARTESIAN_POINT ( 'NONE',  ( -17.14499999999999957, 71.11999999999999034, 5.714999999999999858 ) ) ;
#25487 = CARTESIAN_POINT ( 'NONE',  ( -0.7769838098421247841, 118.1651004966810774, -0.8853101393953053400 ) ) ;
#25488 = VERTEX_POINT ( 'NONE', #36157 ) ;
#25489 = CARTESIAN_POINT ( 'NONE',  ( 15.10275521329001336, 128.5586215118215705, 2.151272397954999249 ) ) ;
#25490 = DIRECTION ( 'NONE',  ( 0.000000000000000000, 0.000000000000000000, -1.000000000000000000 ) ) ;
#25491 = CARTESIAN_POINT ( 'NONE',  ( 5.217040494953375962, 115.7029491485453008, 1.134277920141861129 ) ) ;
#25492 = CARTESIAN_POINT ( 'NONE',  ( -4.368052411777271438, 123.4689364668338385, -0.008193521294099921984 ) ) ;
#25493 = CARTESIAN_POINT ( 'NONE',  ( 5.670988759832523485, -4.508684804710943794, -6.293633234193930726 ) ) ;
#25494 = CARTESIAN_POINT ( 'NONE',  ( 16.04872481256637684, 146.6973543426590254, 1.173426683271129090 ) ) ;
#25495 = CARTESIAN_POINT ( 'NONE',  ( 23.00823290520135345, 149.2143936249396461, -0.3942700086401350057 ) ) ;
#25496 = CARTESIAN_POINT ( 'NONE',  ( 4.662336540953832653, 117.9271336397564909, 0.9606932247104178479 ) ) ;
#25497 = PLANE ( 'NONE',  #27653 ) ;
#25498 = CARTESIAN_POINT ( 'NONE',  ( -18.63504953328976299, 154.1157618415863624, -0.3723726386282264489 ) ) ;
#25499 = ORIENTED_EDGE ( 'NONE', *, *, #35780, .F. ) ;
#25500 = CARTESIAN_POINT ( 'NONE',  ( 6.335329328642134605, 119.9360031486299789, -0.9656527664637336583 ) ) ;
#25501 = CARTESIAN_POINT ( 'NONE',  ( -58.37116772670351850, -0.2940390518722524327, -2.603646672650065119E-13 ) ) ;
#25502 = CARTESIAN_POINT ( 'NONE',  ( 0.008148072696521003327, 156.3406798448389168, -0.4077628766201953359 ) ) ;
#25503 = CARTESIAN_POINT ( 'NONE',  ( 13.85159022459154166, 60.48513866567135722, 5.016500000000000625 ) ) ;
#25504 = CARTESIAN_POINT ( 'NONE',  ( 15.95982161465177285, 121.0385544001969436, 0.3359599701671937000 ) ) ;
#25505 = VERTEX_POINT ( 'NONE', #39562 ) ;
#25506 = CARTESIAN_POINT ( 'NONE',  ( 1.111903444298625754, 15.29877551736591812, 4.515507465039587665 ) ) ;
#25507 = CARTESIAN_POINT ( 'NONE',  ( -30.53944104333574217, 56.31939948593669243, 1.269999999999994023 ) ) ;
#25508 = CARTESIAN_POINT ( 'NONE',  ( -20.69909148798450360, 152.5508394022677692, -0.4136171090298760844 ) ) ;
#25509 = CARTESIAN_POINT ( 'NONE',  ( 17.14499999999999957, 71.11999999999999034, 1.904999999999989146 ) ) ;
#25510 = CARTESIAN_POINT ( 'NONE',  ( 1.406077420118782567E-15, 14.60500000000000220, 0.000000000000000000 ) ) ;
#25511 = CARTESIAN_POINT ( 'NONE',  ( 7.924296910773485081, 121.8627509869352679, 1.022570594433494851 ) ) ;
#25512 = CARTESIAN_POINT ( 'NONE',  ( 0.02375515148176195884, 10.92298121479113426, 4.626086752085273979 ) ) ;
#25513 = CARTESIAN_POINT ( 'NONE',  ( 9.505306604063411768, 118.4542681464805298, 0.9615324788044604665 ) ) ;
#25514 = DIRECTION ( 'NONE',  ( -5.188838149069472160E-16, 1.699382548006136559E-16, 1.000000000000000000 ) ) ;
#25516 = CARTESIAN_POINT ( 'NONE',  ( 9.140851504705331365, 119.2843051134756536, -0.9831809102843881432 ) ) ;
#25515 = CARTESIAN_POINT ( 'NONE',  ( 5.224239234539634680, 57.14999999999999147, 5.327449267724802873 ) ) ;
#25517 = CARTESIAN_POINT ( 'NONE',  ( -16.46509630982090400, 135.1966315799913900, 1.639354953089778633 ) ) ;
#25518 = CARTESIAN_POINT ( 'NONE',  ( 0.7325351754718939512, 15.47086736126800766, -4.571311019245588803 ) ) ;
#25519 = CARTESIAN_POINT ( 'NONE',  ( -22.87667167544120517, 149.1739538623130272, -1.428090254611251275 ) ) ;
#25520 = ORIENTED_EDGE ( 'NONE', *, *, #24067, .F. ) ;
#25521 = CARTESIAN_POINT ( 'NONE',  ( -15.93731397951220252, 146.3070982487133165, 0.2768821801232404511 ) ) ;
#25522 = EDGE_CURVE ( 'NONE', #11267, #37307, #38377, .T. ) ;
#25523 = CARTESIAN_POINT ( 'NONE',  ( 5.669917404453804544, -14.04548127125972101, 2.990483579271598469 ) ) ;
#25524 = DIRECTION ( 'NONE',  ( -5.188838149069472160E-16, 1.699382548006136559E-16, 1.000000000000000000 ) ) ;
#25525 = CARTESIAN_POINT ( 'NONE',  ( -4.564150745914989038, 118.0173319454175669, -0.8780539647668005321 ) ) ;
#25526 = CARTESIAN_POINT ( 'NONE',  ( 15.52759540040485753, 147.5317938866932366, 0.2591190040802687222 ) ) ;
#25528 = ORIENTED_EDGE ( 'NONE', *, *, #30623, .T. ) ;
#25527 = CIRCLE ( 'NONE', #35071, 0.5080000000000000071 ) ;
#25529 = CARTESIAN_POINT ( 'NONE',  ( 16.05419991788299328, 128.5601350900737998, 2.191829208737125612 ) ) ;
#25530 = DIRECTION ( 'NONE',  ( 1.000000000000000000, -9.466894658874049451E-17, 0.000000000000000000 ) ) ;
#25531 = CARTESIAN_POINT ( 'NONE',  ( 5.078986093043054595, 75.27746620154573520, 0.1014902294541237815 ) ) ;
#25532 = CARTESIAN_POINT ( 'NONE',  ( -1.008409768533949036, 116.9791385580615781, 0.3449706568517266758 ) ) ;
#25533 = ADVANCED_FACE ( 'NONE', ( #23762 ), #1427, .F. ) ;
#25534 = CARTESIAN_POINT ( 'NONE',  ( 4.924011148325399212, 117.4782075418523135, -0.9295710142836602907 ) ) ;
#25535 = CARTESIAN_POINT ( 'NONE',  ( 23.30518390908419946, 149.0397177335360652, 0.1341373440727925415 ) ) ;
#25536 = DIRECTION ( 'NONE',  ( -0.01997839162482737546, -1.040247600000940825E-18, 0.9998004120163610509 ) ) ;
#25537 = CARTESIAN_POINT ( 'NONE',  ( 5.341067892174450549, 115.6909491485453145, -0.2000027940544922000 ) ) ;
#25538 = CARTESIAN_POINT ( 'NONE',  ( -8.816700480405424756, 73.94613776634058411, -1.269999999999996909 ) ) ;
#25539 = CARTESIAN_POINT ( 'NONE',  ( -4.974001918027356695, 117.3966124608058266, -0.9751453930575103568 ) ) ;
#25540 = CARTESIAN_POINT ( 'NONE',  ( -46.52557095416602806, 23.25943309041075224, 3.047882326417268750 ) ) ;
#25541 = CARTESIAN_POINT ( 'NONE',  ( -58.68165211130394709, -0.3140782993471775142, 0.3080062417138906827 ) ) ;
#25542 = CARTESIAN_POINT ( 'NONE',  ( -4.590661430219167727, 118.0729565861886812, 0.5857098603017855121 ) ) ;
#25543 = ORIENTED_EDGE ( 'NONE', *, *, #30098, .F. ) ;
#25544 = ORIENTED_EDGE ( 'NONE', *, *, #15680, .T. ) ;
#25545 = CARTESIAN_POINT ( 'NONE',  ( -0.6576497334167915598, 118.7629491485454025, -1.273914634100742127 ) ) ;
#25546 = CARTESIAN_POINT ( 'NONE',  ( 5.935441270543534209, 119.0670427498981212, -1.024523171172543767 ) ) ;
#25547 = CARTESIAN_POINT ( 'NONE',  ( -4.970930975556761666, 121.2162878128435892, -0.3527489803516244971 ) ) ;
#25548 = CARTESIAN_POINT ( 'NONE',  ( 4.604483500233246929, 118.0232679518424135, 0.8447168980634072177 ) ) ;
#25549 = DIRECTION ( 'NONE',  ( -0.8745520943968139171, 0.4849315768086732703, -5.271987356194193006E-16 ) ) ;
#25550 = CARTESIAN_POINT ( 'NONE',  ( -9.846098633339826378, 123.9483309312939099, -0.9889573185143103462 ) ) ;
#25551 = DIRECTION ( 'NONE',  ( -1.000000000000000000, 5.463695987328526437E-16, -6.146657985744592735E-16 ) ) ;
#25552 = CARTESIAN_POINT ( 'NONE',  ( 0.3628555246834703207, 105.8844662015457629, -5.327769491516690437 ) ) ;
#25553 = CARTESIAN_POINT ( 'NONE',  ( -2.540463897194821463, 119.9929590031203901, -0.6352340916430189166 ) ) ;
#25554 = DIRECTION ( 'NONE',  ( -0.5064479475276348897, 0.8622111466057285067, -0.01012003527073128926 ) ) ;
#25555 = CARTESIAN_POINT ( 'NONE',  ( -18.01920641645600796, 83.84822824455466161, -1.270000000000003348 ) ) ;
#25556 = TOROIDAL_SURFACE ( 'NONE', #26220, 3.683000000000000718, 0.5080000000000000071 ) ;
#25557 = CARTESIAN_POINT ( 'NONE',  ( -2.442087156279620253, 115.7029470234981687, 1.605172157923005383 ) ) ;
#25558 = CARTESIAN_POINT ( 'NONE',  ( -1.756104463947763428, 14.33678105357426702, 4.288642365192034234 ) ) ;
#25560 = VERTEX_POINT ( 'NONE', #13566 ) ;
#25559 = CARTESIAN_POINT ( 'NONE',  ( 13.21954506825620612, 156.9672759736256467, 0.8747755986887107982 ) ) ;
#25561 = CARTESIAN_POINT ( 'NONE',  ( -2.150341965413615331, 104.6144662015345972, -4.893691083646714901 ) ) ;
#25562 = CARTESIAN_POINT ( 'NONE',  ( 3.758269890760038034, -15.41186319813359162, 2.599103203065302292 ) ) ;
#25563 = CARTESIAN_POINT ( 'NONE',  ( -0.4903093677402899919, 118.8635629087341954, 0.5952627799645435758 ) ) ;
#25564 = CARTESIAN_POINT ( 'NONE',  ( -0.8770832347484921465, 27.56386522087566249, 0.4220112102557041500 ) ) ;
#25565 = CARTESIAN_POINT ( 'NONE',  ( 0.9769954323678800012, -0.8923827921977626199, -0.09387087892739469364 ) ) ;
#25566 = EDGE_CURVE ( 'NONE', #17215, #37322, #7747, .T. ) ;
#25567 = ORIENTED_EDGE ( 'NONE', *, *, #4338, .F. ) ;
#25568 = VERTEX_POINT ( 'NONE', #7602 ) ;
#25569 = CARTESIAN_POINT ( 'NONE',  ( -6.631541954483209765E-14, 98.39146620154573952, -1.863789202389766375E-18 ) ) ;
#25570 = CARTESIAN_POINT ( 'NONE',  ( 6.647360066587990168, 123.1390089711370166, 0.2039998645198906335 ) ) ;
#25571 = DIRECTION ( 'NONE',  ( 1.000000000000000000, 0.000000000000000000, 0.000000000000000000 ) ) ;
#25572 = CARTESIAN_POINT ( 'NONE',  ( -0.5989337510913105289, 120.4790399057546182, 0.3068722873270141038 ) ) ;
#25573 = CARTESIAN_POINT ( 'NONE',  ( -17.09258512000246455, 84.17916046765628835, 1.269999999999996243 ) ) ;
#25574 = CARTESIAN_POINT ( 'NONE',  ( 3.463597221183738917, -14.01103841792809845, 4.185469790819682068 ) ) ;
#25575 = CARTESIAN_POINT ( 'NONE',  ( 9.157854976475270803, 121.7740273863187923, -1.020316602444926612 ) ) ;
#25576 = CARTESIAN_POINT ( 'NONE',  ( -1.054772537320801673, 158.2739225783580537, -1.630455200628576851 ) ) ;
#25577 = DIRECTION ( 'NONE',  ( -0.9998004120163609398, -4.016384292689130894E-17, -0.01997839162482749689 ) ) ;
#25578 = CARTESIAN_POINT ( 'NONE',  ( 8.362803050136434990, 119.6845577230325688, 1.431069710389275995 ) ) ;
#25579 = CARTESIAN_POINT ( 'NONE',  ( -6.449616047178365896, 30.29533487405314318, -0.03228945779065251626 ) ) ;
#25580 = CARTESIAN_POINT ( 'NONE',  ( 13.63867282259125879, 150.2122286517991085, -0.04772847129159314000 ) ) ;
#25581 = EDGE_LOOP ( 'NONE', ( #21092, #38002, #19886, #540 ) ) ;
#25582 = LINE ( 'NONE', #39427, #4106 ) ;
#25583 = CARTESIAN_POINT ( 'NONE',  ( 2.866728174840395216, 37.98889525090484653, 1.397978221435859147 ) ) ;
#25584 = CARTESIAN_POINT ( 'NONE',  ( -13.85159022459154166, 16.59642619247577500, 5.016500000000000625 ) ) ;
#25585 = TOROIDAL_SURFACE ( 'NONE', #26255, 5.080000000000005400, 0.5080000000000000071 ) ;
#25586 = CARTESIAN_POINT ( 'NONE',  ( -5.002256584969458686, 16.77047026005132224, -6.819937116506380903 ) ) ;
#25587 = CARTESIAN_POINT ( 'NONE',  ( 9.932629385191864557, 123.7598584631124794, 1.097969866555963625 ) ) ;
#25588 = DIRECTION ( 'NONE',  ( 1.000000000000000000, 0.000000000000000000, 0.000000000000000000 ) ) ;
#25589 = CARTESIAN_POINT ( 'NONE',  ( 3.301441731159253656, 159.4676453237595410, 0.05120667577156024636 ) ) ;
#25590 = CARTESIAN_POINT ( 'NONE',  ( -5.069034061154344073, 114.3796182124986984, 1.753882200456532647 ) ) ;
#25591 = LINE ( 'NONE', #46, #40739 ) ;
#25592 = CARTESIAN_POINT ( 'NONE',  ( 14.67500508075654508, 148.8517222230099719, 0.2932415260845993576 ) ) ;
#25593 = EDGE_CURVE ( 'NONE', #14480, #28898, #13853, .T. ) ;
#25594 = CARTESIAN_POINT ( 'NONE',  ( 20.38236371569457361, 141.4490678312372722, 2.395676066357400824 ) ) ;
#25595 = CARTESIAN_POINT ( 'NONE',  ( 8.391225363336687337, -15.30560670943152957, -0.4339906691978474562 ) ) ;
#25596 = CARTESIAN_POINT ( 'NONE',  ( 8.745956712206110595, 117.9959567041441630, -0.4150867728463960016 ) ) ;
#25597 = CARTESIAN_POINT ( 'NONE',  ( -0.9302644990745694287, 122.9246775559910390, -0.2070653534288169895 ) ) ;
#25598 = DIRECTION ( 'NONE',  ( -6.353134868986659519E-16, 1.000000000000000000, 0.000000000000000000 ) ) ;
#25599 = FACE_OUTER_BOUND ( 'NONE', #23708, .T. ) ;
#25600 = CARTESIAN_POINT ( 'NONE',  ( 0.1094753925894137725, 104.6144662015478701, 5.344208972995505569 ) ) ;
#25601 = CARTESIAN_POINT ( 'NONE',  ( -3.685501180670149424, 30.72893705507438611, -2.802369389919810772 ) ) ;
#25602 = DIRECTION ( 'NONE',  ( 9.627370216492862708E-17, 1.000000000000000000, -0.000000000000000000 ) ) ;
#25603 = DIRECTION ( 'NONE',  ( 0.000000000000000000, 1.000000000000000000, 0.000000000000000000 ) ) ;
#25604 = CARTESIAN_POINT ( 'NONE',  ( 1.979733141779612016, -15.19599036556555660, 5.309005240801834447 ) ) ;
#25605 = CARTESIAN_POINT ( 'NONE',  ( 2.294838902200146080, 118.2243428780609662, -0.8383363118275910519 ) ) ;
#25606 = CARTESIAN_POINT ( 'NONE',  ( -4.829765040637250095, 117.0737178285515654, 0.3500672345979856659 ) ) ;
#25607 = VERTEX_POINT ( 'NONE', #26556 ) ;
#25608 = ADVANCED_FACE ( 'NONE', ( #39990 ), #20563, .T. ) ;
#25609 = CARTESIAN_POINT ( 'NONE',  ( 5.305748947172191698, 88.73331249999999670, 5.247078976224250013 ) ) ;
#25610 = EDGE_LOOP ( 'NONE', ( #192, #8062, #28239, #34136, #27229 ) ) ;
#25611 = DIRECTION ( 'NONE',  ( 5.188838149069472160E-16, -1.699382548006136559E-16, -1.000000000000000000 ) ) ;
#25612 = CARTESIAN_POINT ( 'NONE',  ( 4.157678856868515460, -15.71065181052187754, 4.128466586810772831 ) ) ;
#25613 = CARTESIAN_POINT ( 'NONE',  ( -8.948346978250222961, 119.7003323559047061, 1.088312767383050828 ) ) ;
#25614 = CARTESIAN_POINT ( 'NONE',  ( 10.16518949684062534, 157.7687470436769388, -1.006875576665116734 ) ) ;
#25615 = CARTESIAN_POINT ( 'NONE',  ( 1.961646697876492373, -0.1315482170498871728, -4.191205975169975950 ) ) ;
#25616 = CARTESIAN_POINT ( 'NONE',  ( -53.81263303816225374, 9.606026272359288853, -3.797673599996276739 ) ) ;
#25617 = EDGE_LOOP ( 'NONE', ( #31540, #16431, #42151, #30072 ) ) ;
#25618 = CARTESIAN_POINT ( 'NONE',  ( -58.54486130996896520, -0.6084878433709398626, -0.2286541811367976129 ) ) ;
#25619 = TOROIDAL_SURFACE ( 'NONE', #13371, 3.683000000000000718, 0.5080000000000000071 ) ;
#25620 = CARTESIAN_POINT ( 'NONE',  ( -0.006734421714333356339, 121.9236798544229003, 0.3370180007450782056 ) ) ;
#25621 = CARTESIAN_POINT ( 'NONE',  ( -5.874057931648946962, 120.5744318282211651, 0.7168624585904721513 ) ) ;
#25622 = DIRECTION ( 'NONE',  ( 5.188838149069472160E-16, -1.699382548006136559E-16, -1.000000000000000000 ) ) ;
#25623 = ADVANCED_FACE ( 'NONE', ( #17383 ), #1222, .T. ) ;
#25624 = CARTESIAN_POINT ( 'NONE',  ( 11.47069961394310411, 122.2847249198043471, -1.269327653809199763 ) ) ;
#25625 = CARTESIAN_POINT ( 'NONE',  ( -4.785842063580277639, 158.3075559295907055, -1.719165798332182860 ) ) ;
#25626 = CARTESIAN_POINT ( 'NONE',  ( -57.55343345497419705, 2.880119995625998630, -1.988856187846590018 ) ) ;
#25627 = EDGE_CURVE ( 'NONE', #18019, #7919, #36304, .T. ) ;
#25628 = EDGE_LOOP ( 'NONE', ( #19764, #28453, #34983, #20009 ) ) ;
#25629 = CARTESIAN_POINT ( 'NONE',  ( 5.892782515047439773, 121.3091694753028520, -0.3064017138515002237 ) ) ;
#25630 = ORIENTED_EDGE ( 'NONE', *, *, #21163, .T. ) ;
#25631 = CARTESIAN_POINT ( 'NONE',  ( -2.103759425340729461, 157.1282018749678002, -1.585319646506186508 ) ) ;
#25632 = CARTESIAN_POINT ( 'NONE',  ( 3.394867371861720606, -15.19666007832035071, 3.108802900814295000 ) ) ;
#25633 = DIRECTION ( 'NONE',  ( 4.017660918040594346E-17, -1.000000000000000000, -2.376309959284834438E-19 ) ) ;
#25634 = TOROIDAL_SURFACE ( 'NONE', #12039, 0.7620000000000000107, 0.2540000000000000036 ) ;
#25635 = CARTESIAN_POINT ( 'NONE',  ( -41.05189575270517821, 23.09451173561986792, -5.652993304041789371E-15 ) ) ;
#25636 = EDGE_CURVE ( 'NONE', #5073, #19034, #19289, .T. ) ;
#25637 = CARTESIAN_POINT ( 'NONE',  ( -4.900629823555088471, 117.6430597497268451, 0.8581014524456938020 ) ) ;
#25638 = CARTESIAN_POINT ( 'NONE',  ( 17.26689864452585965, 148.5513402141484391, 2.222558794446809927 ) ) ;
#25639 = FACE_BOUND ( 'NONE', #17385, .T. ) ;
#25640 = CIRCLE ( 'NONE', #20856, 5.080000000000006288 ) ;
#25641 = CARTESIAN_POINT ( 'NONE',  ( -3.957843245660688680, 22.95775517496322848, 2.395914033147342970 ) ) ;
#25642 = CARTESIAN_POINT ( 'NONE',  ( 12.03016689884984736, 130.4833683797432684, 0.5359549021282031811 ) ) ;
#25643 = DIRECTION ( 'NONE',  ( 1.000000000000000000, 6.353134868986659519E-16, 0.000000000000000000 ) ) ;
#25644 = TOROIDAL_SURFACE ( 'NONE', #13393, 3.683000000000000718, 0.5080000000000000071 ) ;
#25646 = VERTEX_POINT ( 'NONE', #4837 ) ;
#25645 = CARTESIAN_POINT ( 'NONE',  ( -49.01239152747368166, 15.29178156536908872, -1.600675721865278289 ) ) ;
#25647 = CARTESIAN_POINT ( 'NONE',  ( -0.5679911634757053296, 118.1588899970992372, 0.8844275911688039837 ) ) ;
#25648 = CARTESIAN_POINT ( 'NONE',  ( -6.616924617768071466E-14, 97.37546620154573418, 7.965525879364083286E-30 ) ) ;
#25649 = CARTESIAN_POINT ( 'NONE',  ( -49.54009375067479937, 17.01946532844685223, 5.019578552719032416 ) ) ;
#25650 = CARTESIAN_POINT ( 'NONE',  ( -8.212032660176594945, 120.4197669723354380, -1.432790658092274683 ) ) ;
#25651 = CARTESIAN_POINT ( 'NONE',  ( -6.059261036834474368, 53.58606249999999704, -5.016499999999999737 ) ) ;
#25652 = CARTESIAN_POINT ( 'NONE',  ( -54.22526503003591358, 12.24891082007571086, 1.741649939400648606 ) ) ;
#25653 = ADVANCED_FACE ( 'NONE', ( #21188 ), #24393, .T. ) ;
#25654 = CARTESIAN_POINT ( 'NONE',  ( -8.030623918766140790, 158.6806155330135084, 0.07574440115180955391 ) ) ;
#25655 = ORIENTED_EDGE ( 'NONE', *, *, #40501, .F. ) ;
#25656 = CARTESIAN_POINT ( 'NONE',  ( -55.34794038087419210, 7.786537553440359360, -3.264576684945873275 ) ) ;
#25657 = CARTESIAN_POINT ( 'NONE',  ( 7.824763724456980540, 122.4691624671024499, -0.2194572792259929794 ) ) ;
#25658 = CARTESIAN_POINT ( 'NONE',  ( 5.008434261519718156, 117.3975399490705342, -0.7758999597088642730 ) ) ;
#25659 = ORIENTED_EDGE ( 'NONE', *, *, #39143, .F. ) ;
#25660 = CARTESIAN_POINT ( 'NONE',  ( 2.876251655540356111, 115.7032362331918307, -1.566559221233196686 ) ) ;
#25661 = CARTESIAN_POINT ( 'NONE',  ( -8.997762725188083621, 123.9218113011205986, -0.2640260769295984522 ) ) ;
#25662 = CARTESIAN_POINT ( 'NONE',  ( 5.593658044048013700, -13.59245692957503060, 2.833247147397068399 ) ) ;
#25663 = CARTESIAN_POINT ( 'NONE',  ( -21.51828093163823041, 145.9698620541949765, 1.394984360948490432 ) ) ;
#25664 = CARTESIAN_POINT ( 'NONE',  ( 5.800481910058622681, 78.89561208401062231, -5.028344476440722133 ) ) ;
#25665 = CARTESIAN_POINT ( 'NONE',  ( 21.88244685892433239, 151.4414241944827495, 0.6640443303913107220 ) ) ;
#25666 = VECTOR ( 'NONE', #20521, 1000.000000000000000 ) ;
#25667 = CARTESIAN_POINT ( 'NONE',  ( 8.867535967563629384, 123.8953242916030462, 0.2653767370228412026 ) ) ;
#25668 = DIRECTION ( 'NONE',  ( -0.000000000000000000, -1.000000000000000000, -0.000000000000000000 ) ) ;
#25669 = CARTESIAN_POINT ( 'NONE',  ( 0.1867991717342751268, 10.66319190514178139, -0.9583599856553294272 ) ) ;
#25670 = CARTESIAN_POINT ( 'NONE',  ( -22.82515744214359898, 150.4067493646842593, -0.6093393687072345966 ) ) ;
#25671 = DIRECTION ( 'NONE',  ( -0.9511648638205115747, -0.3086833358529540439, -8.537024980200888871E-16 ) ) ;
#25672 = DIRECTION ( 'NONE',  ( 5.188838149069472160E-16, -1.699382548006136559E-16, -1.000000000000000000 ) ) ;
#25673 = VERTEX_POINT ( 'NONE', #15230 ) ;
#25674 = CARTESIAN_POINT ( 'NONE',  ( 8.541884356874501094, 118.8312421787186111, 1.225717238265990883 ) ) ;
#25675 = ORIENTED_EDGE ( 'NONE', *, *, #20890, .F. ) ;
#25676 = CARTESIAN_POINT ( 'NONE',  ( -58.36413812860618577, -0.2797192912122439812, -0.09355837775955268276 ) ) ;
#25677 = CARTESIAN_POINT ( 'NONE',  ( 13.91935487398206739, 155.8415165211600595, 1.849969996916311921 ) ) ;
#25678 = CARTESIAN_POINT ( 'NONE',  ( 20.15738656758741598, 148.0303212619860744, -1.701566911850818986 ) ) ;
#25679 = CARTESIAN_POINT ( 'NONE',  ( 7.912908961612729719, 12.87109176889305928, 2.878135455392844655 ) ) ;
#25680 = CARTESIAN_POINT ( 'NONE',  ( -21.74891716461465663, 141.9756885651356413, -2.029123422127836029 ) ) ;
#25681 = CARTESIAN_POINT ( 'NONE',  ( 4.751009958040408598, 117.9441986225446470, -0.6307358576018021745 ) ) ;
#25682 = EDGE_CURVE ( 'NONE', #33118, #24559, #1638, .T. ) ;
#25683 = CARTESIAN_POINT ( 'NONE',  ( 5.947819151547380834, 118.9610140496397719, 0.5876226394569610267 ) ) ;
#25684 = AXIS2_PLACEMENT_3D ( 'NONE', #36896, #20883, #7290 ) ;
#25685 = CARTESIAN_POINT ( 'NONE',  ( -3.751144962740160960, 121.0949217282140182, -0.04819499160668135052 ) ) ;
#25686 = CARTESIAN_POINT ( 'NONE',  ( -18.97908907040220683, 145.0145856610025987, -2.515253529532921473 ) ) ;
#25687 = CARTESIAN_POINT ( 'NONE',  ( 5.309364964326869440, -15.28511724905957969, 2.738662543889408774 ) ) ;
#25688 = CARTESIAN_POINT ( 'NONE',  ( -17.14500000000466784, 71.11999999999886768, -1.524000000000000909 ) ) ;
#25689 = CARTESIAN_POINT ( 'NONE',  ( -45.45367893016184979, 22.54667639846615046, -3.012003376585093317 ) ) ;
#25690 = VERTEX_POINT ( 'NONE', #18205 ) ;
#25691 = CARTESIAN_POINT ( 'NONE',  ( 7.475014592328083296, 120.3045338523282197, 1.338105361635808732 ) ) ;
#25692 =( LENGTH_UNIT ( ) NAMED_UNIT ( * ) SI_UNIT ( .MILLI., .METRE. ) );
#25693 = CARTESIAN_POINT ( 'NONE',  ( -17.14499999999999957, 71.11999999999999034, 1.904999999999989146 ) ) ;
#25694 = CIRCLE ( 'NONE', #29778, 3.683000000000001162 ) ;
#25695 = CARTESIAN_POINT ( 'NONE',  ( -4.469499996960022870, 123.9529229959338608, -0.04273414237147016986 ) ) ;
#25696 = CARTESIAN_POINT ( 'NONE',  ( 7.100331465950064036, 27.70181474634058461, -4.559502152892632942 ) ) ;
#25697 = CARTESIAN_POINT ( 'NONE',  ( 8.043896744443927105, 154.6119571123129788, 0.8805139685443127417 ) ) ;
#25698 = CARTESIAN_POINT ( 'NONE',  ( 13.02773564672682127, 156.9259531928012734, -0.6619068571425152925 ) ) ;
#25699 = DIRECTION ( 'NONE',  ( 0.000000000000000000, 0.000000000000000000, -1.000000000000000000 ) ) ;
#25700 = DIRECTION ( 'NONE',  ( -4.017660918040594346E-17, 1.000000000000000000, 2.376309959284834438E-19 ) ) ;
#25701 = PRODUCT_DEFINITION_CONTEXT ( 'detailed design', #42030, 'design' ) ;
#25702 = CARTESIAN_POINT ( 'NONE',  ( -18.84845417996787020, 125.3331924886369961, -0.3579177782036729871 ) ) ;
#25703 = VERTEX_POINT ( 'NONE', #24819 ) ;
#25704 = CARTESIAN_POINT ( 'NONE',  ( 4.791256430390820498, 119.8698651693515416, -0.7146009144274133584 ) ) ;
#25705 = CARTESIAN_POINT ( 'NONE',  ( 5.379065264290444404, -14.65747380975624381, 3.538013181455927914 ) ) ;
#25706 = CARTESIAN_POINT ( 'NONE',  ( -9.927929498514854956, 124.8826105625126530, -0.6426615136408515561 ) ) ;
#25707 = CARTESIAN_POINT ( 'NONE',  ( -30.29872984418086901, 56.23795811436772851, 1.523999999999994248 ) ) ;
#25708 = CARTESIAN_POINT ( 'NONE',  ( 0.2932902739209606313, 116.4254261620736344, 0.01852769337193122673 ) ) ;
#25709 = VERTEX_POINT ( 'NONE', #18000 ) ;
#25710 = CARTESIAN_POINT ( 'NONE',  ( -4.627450822138572839, 2.892058097378844117, -0.1328416527703782657 ) ) ;
#25711 = CARTESIAN_POINT ( 'NONE',  ( -16.18905205736058051, 121.2598130428683447, -0.3234957879086920451 ) ) ;
#25712 = LINE ( 'NONE', #9528, #29637 ) ;
#25713 = DIRECTION ( 'NONE',  ( 5.188838149069472160E-16, -1.699382548006136559E-16, -1.000000000000000000 ) ) ;
#25714 = DIRECTION ( 'NONE',  ( -4.017660918040594346E-17, 1.000000000000000000, 2.376309959284834438E-19 ) ) ;
#25715 = CARTESIAN_POINT ( 'NONE',  ( 6.098048384433346847, 121.2450635489416015, 0.6169096678833930758 ) ) ;
#25716 = CARTESIAN_POINT ( 'NONE',  ( -3.833338661037195561, 9.423677021345861604, 2.587938769098377279 ) ) ;
#25717 = CARTESIAN_POINT ( 'NONE',  ( 0.3477286622123275106, 117.0882377308211773, 0.3718801884458514673 ) ) ;
#25718 = CARTESIAN_POINT ( 'NONE',  ( -4.556757383386185190, 31.49269130883712720, -0.6906699653381264126 ) ) ;
#25720 = CARTESIAN_POINT ( 'NONE',  ( 2.840063763404204522, 158.7847427699215928, -1.391859091975727436 ) ) ;
#25719 = CARTESIAN_POINT ( 'NONE',  ( -6.059261036834082681, 78.87450423423038615, 5.016499999999999737 ) ) ;
#25721 = CARTESIAN_POINT ( 'NONE',  ( -4.556395268149300293, 8.773967715207941609, 0.7749943352582737699 ) ) ;
#25722 = CARTESIAN_POINT ( 'NONE',  ( -5.832486214875789443, 117.3024554866451865, -0.6456718139904970011 ) ) ;
#25723 = AXIS2_PLACEMENT_3D ( 'NONE', #19794, #36011, #38783 ) ;
#25724 = ORIENTED_EDGE ( 'NONE', *, *, #36656, .F. ) ;
#25725 = CARTESIAN_POINT ( 'NONE',  ( -0.008148072696648066618, 156.3406798448389168, 0.4077628766201955579 ) ) ;
#25726 = CARTESIAN_POINT ( 'NONE',  ( 3.968318174290614397, -14.81366206205479763, 5.151173006574525814 ) ) ;
#25727 = DIRECTION ( 'NONE',  ( 6.353134868986659519E-16, -1.000000000000000000, -0.000000000000000000 ) ) ;
#25728 = CARTESIAN_POINT ( 'NONE',  ( -4.625471757156744523, 117.9841676167708044, -0.8981547367807174442 ) ) ;
#25729 = CARTESIAN_POINT ( 'NONE',  ( 8.981069108608807028, 123.9698733229553937, 0.1794631345465901584 ) ) ;
#25730 = ORIENTED_EDGE ( 'NONE', *, *, #25005, .T. ) ;
#25731 = CARTESIAN_POINT ( 'NONE',  ( 19.83855703208262966, 148.9191654756151024, 2.494779984669014183 ) ) ;
#25732 = CARTESIAN_POINT ( 'NONE',  ( -7.917360960270791281, 70.00264313970245666, -1.269999999999995799 ) ) ;
#25733 = CARTESIAN_POINT ( 'NONE',  ( 19.68500000000000227, 71.11999999999999034, 5.016499999999999737 ) ) ;
#25734 = CARTESIAN_POINT ( 'NONE',  ( -22.87957784423544894, 146.5373477140321938, 0.6332847025415453412 ) ) ;
#25735 = CARTESIAN_POINT ( 'NONE',  ( 4.803906986837436222, 117.5395264250762750, -0.9847398809678364895 ) ) ;
#25736 = CARTESIAN_POINT ( 'NONE',  ( 21.78567168733521697, 151.4242408681541008, -0.1492089687398848730 ) ) ;
#25737 = CARTESIAN_POINT ( 'NONE',  ( 12.21488373879589417, 55.24500000000000455, -5.016499999999999737 ) ) ;
#25738 = CARTESIAN_POINT ( 'NONE',  ( -6.057513928997659391, 86.35999999999998522, -1.904999999999999805 ) ) ;
#25739 = CARTESIAN_POINT ( 'NONE',  ( 5.177913976931196594, 78.94499979771845233, 5.372100000000001430 ) ) ;
#25740 = DIRECTION ( 'NONE',  ( 1.011795553208986377E-16, 1.000000000000000000, -0.000000000000000000 ) ) ;
#25741 = CARTESIAN_POINT ( 'NONE',  ( -44.96292901393739783, 21.56701576681934540, 3.486870777078499017 ) ) ;
#25742 = DIRECTION ( 'NONE',  ( -5.206863593109713661E-17, 1.000000000000000000, -1.077750396879097183E-30 ) ) ;
#25743 = CARTESIAN_POINT ( 'NONE',  ( -4.563054629617739444, 118.0738312922104427, 0.6152185306409869714 ) ) ;
#25744 = CARTESIAN_POINT ( 'NONE',  ( -58.36439606173801309, -0.2818266832427390733, -0.2195612235341928287 ) ) ;
#25745 = EDGE_LOOP ( 'NONE', ( #22535, #1915, #3706, #11314 ) ) ;
#25746 = VERTEX_POINT ( 'NONE', #34418 ) ;
#25747 = CARTESIAN_POINT ( 'NONE',  ( 5.078986093043054595, 75.78546620154573077, 0.1014902294541237815 ) ) ;
#25748 = AXIS2_PLACEMENT_3D ( 'NONE', #17125, #19682, #4378 ) ;
#25749 = CARTESIAN_POINT ( 'NONE',  ( -5.940513678270559872, 119.1894665386702599, -1.265456493235758373 ) ) ;
#25750 = CARTESIAN_POINT ( 'NONE',  ( -5.310592030460785651, 116.9519127983885340, -0.9557578278138695316 ) ) ;
#25751 = CARTESIAN_POINT ( 'NONE',  ( 4.688515861213570446, 117.9735081910210255, 0.8265790947846195502 ) ) ;
#25752 = CIRCLE ( 'NONE', #13518, 0.2539999999999942859 ) ;
#25753 = DIRECTION ( 'NONE',  ( -5.188838149069471174E-16, 1.699382548006136313E-16, 1.000000000000000000 ) ) ;
#25754 = CARTESIAN_POINT ( 'NONE',  ( 0.006077178772629055273, 120.4695998130595598, -0.3041268764237431421 ) ) ;
#25755 = DIRECTION ( 'NONE',  ( 0.8745520943968251304, -0.4849315768086535638, -5.653143757709532409E-15 ) ) ;
#25756 = CARTESIAN_POINT ( 'NONE',  ( -6.059261036834475256, 56.81853847168529370, 4.948064083792229617 ) ) ;
#25757 = LINE ( 'NONE', #33372, #12436 ) ;
#25758 = CARTESIAN_POINT ( 'NONE',  ( 5.480007210012603380, 117.5214873295501405, -0.6081561229113361389 ) ) ;
#25759 = CARTESIAN_POINT ( 'NONE',  ( -15.36238541928155676, 134.8939017613128328, -2.058614936883395252 ) ) ;
#25760 = CARTESIAN_POINT ( 'NONE',  ( 17.31377588638417819, 122.7721875394316555, 0.3459704467065362055 ) ) ;
#25761 = CARTESIAN_POINT ( 'NONE',  ( -0.01133159106151501033, 159.5297144918048673, 0.5670791535570577357 ) ) ;
#25762 = CARTESIAN_POINT ( 'NONE',  ( -12.21488373879589240, 17.14500000000000313, -4.381499999999999950 ) ) ;
#25763 = CARTESIAN_POINT ( 'NONE',  ( -4.157303687089163979, 2.242350289152962528, -2.029258473605290103 ) ) ;
#25765 = ORIENTED_EDGE ( 'NONE', *, *, #13703, .F. ) ;
#25764 = CARTESIAN_POINT ( 'NONE',  ( 22.76704383476076643, 150.0845277111093310, 1.179919005961814316 ) ) ;
#25766 = LINE ( 'NONE', #19369, #19929 ) ;
#25767 = CARTESIAN_POINT ( 'NONE',  ( 3.462569250300066681, -15.15729918637651075, 2.757833548007345037 ) ) ;
#25768 = CARTESIAN_POINT ( 'NONE',  ( -12.38900849369197488, 122.4057692182592092, 1.312116060471626433 ) ) ;
#25769 = CARTESIAN_POINT ( 'NONE',  ( 0.4369565669422456611, 1.205365006982008547, 0.8739355888918843851 ) ) ;
#25770 = CARTESIAN_POINT ( 'NONE',  ( 0.8726510978149698561, 7.843753604616166442, 0.4398688123008435147 ) ) ;
#25771 = ORIENTED_EDGE ( 'NONE', *, *, #17307, .T. ) ;
#25772 = ORIENTED_EDGE ( 'NONE', *, *, #35802, .T. ) ;
#25773 = DIRECTION ( 'NONE',  ( 0.8138664877804110409, -0.5810519254489896479, 5.002558946445370251E-16 ) ) ;
#25774 = CARTESIAN_POINT ( 'NONE',  ( 3.352959238113102813, 119.3320731715853782, 0.6187547705018834332 ) ) ;
#25775 = DIRECTION ( 'NONE',  ( 1.000000000000000000, 0.000000000000000000, 0.000000000000000000 ) ) ;
#25776 = CARTESIAN_POINT ( 'NONE',  ( -15.97699994813262236, 148.2453349897154737, 0.9478121846735144684 ) ) ;
#25777 = CARTESIAN_POINT ( 'NONE',  ( 3.873131646279637241, -11.92617534808754165, 0.9134907789774980857 ) ) ;
#25778 = CARTESIAN_POINT ( 'NONE',  ( 12.79346581414803907, 125.9836878220586556, -1.262672879670394099 ) ) ;
#25779 = CARTESIAN_POINT ( 'NONE',  ( -6.251746415250131861, 157.3995435888475072, -1.956906209352898385 ) ) ;
#25780 = CARTESIAN_POINT ( 'NONE',  ( -6.639407854763120941E-14, 101.6934662015457320, 3.307182826377456566E-30 ) ) ;
#25781 = CARTESIAN_POINT ( 'NONE',  ( 7.851011797225573297, 122.2448088404016744, 0.7696373360186058443 ) ) ;
#25782 = CARTESIAN_POINT ( 'NONE',  ( -0.03167860221993856057, 39.02239338330883811, 0.4531538051958025060 ) ) ;
#25783 = CARTESIAN_POINT ( 'NONE',  ( 8.936721596564167314, 123.7033391712731145, -0.04711667938246239667 ) ) ;
#25784 = ORIENTED_EDGE ( 'NONE', *, *, #9101, .F. ) ;
#25785 = DIRECTION ( 'NONE',  ( -5.188838149069472160E-16, 1.699382548006136559E-16, 1.000000000000000000 ) ) ;
#25786 = AXIS2_PLACEMENT_3D ( 'NONE', #3997, #4202, #4623 ) ;
#25787 = AXIS2_PLACEMENT_3D ( 'NONE', #10673, #29854, #10883 ) ;
#25788 = CIRCLE ( 'NONE', #31915, 0.2539999999999989488 ) ;
#25789 = DIRECTION ( 'NONE',  ( -0.8745520943968252414, 0.4849315768086529532, -5.691349986800548865E-16 ) ) ;
#25790 = CARTESIAN_POINT ( 'NONE',  ( -4.582397001690157623, 27.87760190724945630, 0.5120981666136417143 ) ) ;
#25791 = CARTESIAN_POINT ( 'NONE',  ( 10.02582114772196320, 123.8737202207250618, 1.106617482833786026 ) ) ;
#25792 = CARTESIAN_POINT ( 'NONE',  ( 4.581716828367337513, -15.30239761468843973, -0.5121115983836379559 ) ) ;
#25793 = CARTESIAN_POINT ( 'NONE',  ( 6.900242392319256624, 117.1694300671557727, 0.09431812980450680894 ) ) ;
#25794 = CARTESIAN_POINT ( 'NONE',  ( -5.120189775498736218, 114.3381464724725447, 1.761508159713760957 ) ) ;
#25795 = CARTESIAN_POINT ( 'NONE',  ( -15.21260244842765808, 1.539204351005524363E-15, 0.000000000000000000 ) ) ;
#25796 = DIRECTION ( 'NONE',  ( -0.1906721105965138718, 0.9816537812491076265, -2.657572025465751014E-16 ) ) ;
#25797 = CARTESIAN_POINT ( 'NONE',  ( -4.432242455686237648, 32.76553509196318004, 1.287969469385144006 ) ) ;
#25798 = CARTESIAN_POINT ( 'NONE',  ( 16.06052414861342825, 125.3625853296581312, 1.884096674228965540 ) ) ;
#25799 = CARTESIAN_POINT ( 'NONE',  ( 0.7325351754718939512, 15.47086736126800766, -4.571311019245588803 ) ) ;
#25800 = CARTESIAN_POINT ( 'NONE',  ( 8.358864306157585133, 27.05150166619590379, -1.223686670289468870 ) ) ;
#25801 = CARTESIAN_POINT ( 'NONE',  ( 2.178318100214458042, 116.7197325431357626, -0.3987410329529229025 ) ) ;
#25802 = CARTESIAN_POINT ( 'NONE',  ( -1.569003042721709651, 118.7759820277219944, -0.8276293794157988382 ) ) ;
#25803 = CARTESIAN_POINT ( 'NONE',  ( 2.461950787117386241, 107.2461522219063852, -4.634887458941427951 ) ) ;
#25804 = CARTESIAN_POINT ( 'NONE',  ( 3.603301376113230869, 105.1231864822307074, 3.947254286302657622 ) ) ;
#25805 = CARTESIAN_POINT ( 'NONE',  ( -4.603678009535974169, 12.38766144714272066, -0.4343361176327051321 ) ) ;
#25806 = CARTESIAN_POINT ( 'NONE',  ( 4.691674582040246122, 118.1588881536613655, 0.6237239105626953828 ) ) ;
#25807 = CARTESIAN_POINT ( 'NONE',  ( -18.86374853661781970, 125.3403196291361610, -0.3769425889880998470 ) ) ;
#25808 = CARTESIAN_POINT ( 'NONE',  ( 3.074000544403499902, -13.70685301784095600, 1.494313880732895283 ) ) ;
#25809 = CARTESIAN_POINT ( 'NONE',  ( 1.209846520933339553, 108.5039085404744981, -4.223631676023018144 ) ) ;
#25810 = CARTESIAN_POINT ( 'NONE',  ( -8.172070396906034873, 117.7057695168643932, 0.3161122371724937041 ) ) ;
#25811 = CIRCLE ( 'NONE', #4771, 0.2540000000000057767 ) ;
#25812 = ORIENTED_EDGE ( 'NONE', *, *, #36768, .F. ) ;
#25813 = CARTESIAN_POINT ( 'NONE',  ( 5.475330206976777525, 88.73331249999999670, 5.107412922131463695 ) ) ;
#25814 = AXIS2_PLACEMENT_3D ( 'NONE', #16546, #39353, #19952 ) ;
#25815 = ORIENTED_EDGE ( 'NONE', *, *, #18492, .F. ) ;
#25816 = CARTESIAN_POINT ( 'NONE',  ( 4.081004676854354862, -15.57459693632588760, 4.681182614216856663 ) ) ;
#25817 = CARTESIAN_POINT ( 'NONE',  ( -10.41147150295396528, 120.1444133044471556, 1.103258690517171514 ) ) ;
#25818 = CARTESIAN_POINT ( 'NONE',  ( 5.877369116561975915, 117.9059190437751141, -0.7167914486236909299 ) ) ;
#25819 = CARTESIAN_POINT ( 'NONE',  ( 3.895047602890354010, -2.730319773039217690, 2.488009491782988469 ) ) ;
#25820 = EDGE_CURVE ( 'NONE', #19060, #26194, #29522, .T. ) ;
#25821 = CARTESIAN_POINT ( 'NONE',  ( -58.14663602181426683, 0.7450421216238902744, -1.200248684312827496 ) ) ;
#25822 = ORIENTED_EDGE ( 'NONE', *, *, #28749, .F. ) ;
#25823 = CARTESIAN_POINT ( 'NONE',  ( -58.10259267898851476, 0.2821446311931097295, -0.7168088428569907578 ) ) ;
#25824 = CARTESIAN_POINT ( 'NONE',  ( 0.3562792453294140183, 120.3637084677653633, 0.5982640298941754864 ) ) ;
#25825 = CARTESIAN_POINT ( 'NONE',  ( -8.085704850285766909, 121.5393406094847819, 0.8545391641419388673 ) ) ;
#25826 = DIRECTION ( 'NONE',  ( -0.9816537812491076265, -0.1906721105965138718, -4.769617732184456426E-16 ) ) ;
#25827 = CARTESIAN_POINT ( 'NONE',  ( 11.86655615995733903, 122.9427978038690270, -1.277170931065712445 ) ) ;
#25828 = CARTESIAN_POINT ( 'NONE',  ( -0.4079906055176309998, 117.9789173577105572, -0.5621165275234436542 ) ) ;
#25829 = CARTESIAN_POINT ( 'NONE',  ( -58.33777482027510786, 1.113448835244251756, -1.208045587469442017 ) ) ;
#25830 = ORIENTED_EDGE ( 'NONE', *, *, #9148, .F. ) ;
#25831 = CARTESIAN_POINT ( 'NONE',  ( 4.456149177844714870, 118.1611006391523802, -0.4359789887486856808 ) ) ;
#25832 = EDGE_CURVE ( 'NONE', #25646, #12982, #34007, .T. ) ;
#25833 = CARTESIAN_POINT ( 'NONE',  ( 16.08724493259836308, 146.0544122543811341, -0.5338004346038368597 ) ) ;
#25834 = ORIENTED_EDGE ( 'NONE', *, *, #7844, .T. ) ;
#25835 = CARTESIAN_POINT ( 'NONE',  ( -2.508893989683191883, 119.8406177399916714, -0.6723988897110714236 ) ) ;
#25836 = CARTESIAN_POINT ( 'NONE',  ( 3.518836906362542205, -15.09289160254213868, 2.194652486238897193 ) ) ;
#25837 = CARTESIAN_POINT ( 'NONE',  ( -3.292844983492351663, 105.1237654751116679, -4.198017798423213875 ) ) ;
#25838 = CARTESIAN_POINT ( 'NONE',  ( -46.67338572489354931, 16.85372243840488338, -7.793947694802422673E-15 ) ) ;
#25839 = TOROIDAL_SURFACE ( 'NONE', #31286, 5.080000000000005400, 0.5080000000000000071 ) ;
#25840 = CARTESIAN_POINT ( 'NONE',  ( -4.880401117214993256, 117.7311422177337477, 0.7973360288362750792 ) ) ;
#25841 = CARTESIAN_POINT ( 'NONE',  ( 0.8355136867051613514, 157.0053619834820324, 1.416332280276763056 ) ) ;
#25842 = DIRECTION ( 'NONE',  ( 0.8745520943968249084, -0.4849315768086533418, 5.271987356194193006E-16 ) ) ;
#25843 = CARTESIAN_POINT ( 'NONE',  ( -3.290491044589036740, 30.52917213649525507, -3.264312889705288878 ) ) ;
#25844 = CARTESIAN_POINT ( 'NONE',  ( 9.171413160121566932, 124.0935018032023436, 0.3437271393031031685 ) ) ;
#25845 = DIRECTION ( 'NONE',  ( -5.188838149069471174E-16, 1.699382548006136313E-16, 1.000000000000000000 ) ) ;
#25846 = EDGE_CURVE ( 'NONE', #21511, #32767, #8410, .T. ) ;
#25847 = EDGE_CURVE ( 'NONE', #6137, #4990, #37606, .T. ) ;
#25848 = CARTESIAN_POINT ( 'NONE',  ( -49.86808358410245745, 14.13890166617936472, -1.547476669397169546 ) ) ;
#25849 = CARTESIAN_POINT ( 'NONE',  ( -30.15642192025596202, 71.36377005712995469, 1.269999999999991580 ) ) ;
#25850 = CARTESIAN_POINT ( 'NONE',  ( -46.75046525359888960, 25.87185527623879366, -1.402209946078870173 ) ) ;
#25851 = CARTESIAN_POINT ( 'NONE',  ( -54.48477107295269661, 8.311058014251186066, 3.524008549750177188 ) ) ;
#25852 = LINE ( 'NONE', #32679, #3908 ) ;
#25853 = EDGE_CURVE ( 'NONE', #35981, #13983, #41070, .T. ) ;
#25854 = FACE_OUTER_BOUND ( 'NONE', #13203, .T. ) ;
#25855 = DIRECTION ( 'NONE',  ( 0.6559537821943227653, -0.7548010569845297058, 4.686333752532403923E-16 ) ) ;
#25856 = CARTESIAN_POINT ( 'NONE',  ( -56.90132276708389725, 4.901539372897764757, 1.453963793661417370 ) ) ;
#25857 = CARTESIAN_POINT ( 'NONE',  ( -57.97566020452313040, 1.918554019021911916, 1.632400077439698061 ) ) ;
#25858 = B_SPLINE_CURVE_WITH_KNOTS ( 'NONE', 3,
 ( #22081, #38089, #35108, #5933, #31903, #6760, #16544, #9738, #29554, #20154, #42133, #16754, #6344, #22916, #29115, #35736, #23125, #33177, #22707, #35948, #4006, #39139, #7196, #12930, #19522, #19950, #16963, #19728, #3794, #598, #25920, #6548, #32530, #9944, #29963, #38928 ),
 .UNSPECIFIED., .F., .F.,
 ( 4, 2, 2, 2, 2, 2, 2, 2, 2, 2, 2, 2, 2, 2, 2, 2, 2, 4 ),
 ( 0.0005651914853900366935, 0.001585058938068627417, 0.002604926390747218032, 0.003624793843425808647, 0.004644661296104399262, 0.005664528748782989877, 0.006684396201461581359, 0.007704263654140174576, 0.008724131106818766926, 0.009743998559497358408, 0.01076386601217595336, 0.01178373346485454658, 0.01280360091753313979, 0.01382346837021173648, 0.01484333582289032970, 0.01535326954922962457, 0.01586320327556892118, 0.01688307072824751093 ),
 .UNSPECIFIED. ) ;
#25859 = CARTESIAN_POINT ( 'NONE',  ( -8.206428610460363871, 117.5568930537867800, 0.09596530983984032093 ) ) ;
#25860 = ORIENTED_EDGE ( 'NONE', *, *, #17757, .F. ) ;
#25861 = CARTESIAN_POINT ( 'NONE',  ( -54.34407705511657127, 12.44913727002957415, -1.242021477015530451 ) ) ;
#25862 = CARTESIAN_POINT ( 'NONE',  ( 7.815145927280279459, 122.5100161380369883, -0.1573892018284728800 ) ) ;
#25863 = EDGE_LOOP ( 'NONE', ( #14285, #9695, #24590, #28812 ) ) ;
#25864 = CARTESIAN_POINT ( 'NONE',  ( 2.051540280110341286, 115.7029491863636252, -1.635878083004340233 ) ) ;
#25866 = CARTESIAN_POINT ( 'NONE',  ( -5.992274430539111130, 155.3621521873626534, -0.2980204051088302664 ) ) ;
#25865 = CIRCLE ( 'NONE', #31304, 0.3810000000000015041 ) ;
#25867 = CARTESIAN_POINT ( 'NONE',  ( 2.663994046441380270, -15.36521416583532051, 5.826768514169494040 ) ) ;
#25868 = CARTESIAN_POINT ( 'NONE',  ( -2.121647970409728856, 117.6567184779878232, 0.5798693372496744880 ) ) ;
#25869 = CARTESIAN_POINT ( 'NONE',  ( -5.041199056414468416, 117.2682846570353234, -0.6824308366424440830 ) ) ;
#25870 = CARTESIAN_POINT ( 'NONE',  ( 9.776364138556694172, 118.0142902678875885, 0.3953848830946986581 ) ) ;
#25871 = CARTESIAN_POINT ( 'NONE',  ( 4.628951617348011638, 121.2001895567974117, 0.1993854900221215809 ) ) ;
#25872 = DIRECTION ( 'NONE',  ( 0.000000000000000000, 0.000000000000000000, 1.000000000000000000 ) ) ;
#25873 = CARTESIAN_POINT ( 'NONE',  ( 0.1178611003048646577, 6.342877585758503578, 0.9680126135609015137 ) ) ;
#25874 = CARTESIAN_POINT ( 'NONE',  ( -22.65355654554115716, 150.6414900647796173, -0.6056372710714957863 ) ) ;
#25875 = CARTESIAN_POINT ( 'NONE',  ( -10.44685452804832160, 82.62549350906336088, 1.269999999999998908 ) ) ;
#25876 = DIRECTION ( 'NONE',  ( -0.8138664877804109299, -0.5810519254489895369, 0.000000000000000000 ) ) ;
#25877 = ORIENTED_EDGE ( 'NONE', *, *, #37318, .T. ) ;
#25878 = CARTESIAN_POINT ( 'NONE',  ( 5.544816079372258955, 117.3577646156732328, 0.8411452473849327927 ) ) ;
#25879 = VERTEX_POINT ( 'NONE', #31206 ) ;
#25880 = DIRECTION ( 'NONE',  ( -0.01997839162482761832, -1.040247600000950455E-18, 0.9998004120163610509 ) ) ;
#25881 = CARTESIAN_POINT ( 'NONE',  ( 2.121516847112188575, 117.7847241295267651, 0.6923378844829271017 ) ) ;
#25882 = CARTESIAN_POINT ( 'NONE',  ( 0.4701463269443866833, 118.5593716040226724, -0.5956656855050134203 ) ) ;
#25883 = CARTESIAN_POINT ( 'NONE',  ( -6.209159877377784298, 7.473591768893033560, -5.687189600455027971 ) ) ;
#25884 = CARTESIAN_POINT ( 'NONE',  ( -2.066728864739012295, 117.5043770775735510, -0.6257643424168403135 ) ) ;
#25885 = CARTESIAN_POINT ( 'NONE',  ( 4.629299653413243121, 117.9776611452159614, -0.7348692566910467461 ) ) ;
#25886 = AXIS2_PLACEMENT_3D ( 'NONE', #17151, #30151, #993 ) ;
#25887 = CARTESIAN_POINT ( 'NONE',  ( 5.298772840285820962, 116.6867539651165373, 1.022742042655826245 ) ) ;
#25888 = CARTESIAN_POINT ( 'NONE',  ( -0.001367086239821354828, 156.3041635968983485, 0.06841458569046227067 ) ) ;
#25889 = ORIENTED_EDGE ( 'NONE', *, *, #31107, .F. ) ;
#25890 = CARTESIAN_POINT ( 'NONE',  ( -9.942133252021321255, 155.4362223408194836, -2.105659105541914045 ) ) ;
#25891 = CARTESIAN_POINT ( 'NONE',  ( 5.680254533628135150, -15.02324869320220735, 2.089386157847644920 ) ) ;
#25892 = CARTESIAN_POINT ( 'NONE',  ( 1.172031118611134874E-15, 12.17394877578616885, 0.000000000000000000 ) ) ;
#25893 = CIRCLE ( 'NONE', #31338, 2.540000000000000480 ) ;
#25894 = CARTESIAN_POINT ( 'NONE',  ( -46.52557095416602806, 23.25943309041075224, -3.047882326417284293 ) ) ;
#25895 = EDGE_CURVE ( 'NONE', #16499, #17903, #4966, .T. ) ;
#25896 = ORIENTED_EDGE ( 'NONE', *, *, #15368, .T. ) ;
#25897 = B_SPLINE_SURFACE_WITH_KNOTS ( 'NONE', 3, 3, ( 
 ( #7917, #34324, #30272, #21090, #17283, #4735, #1325, #21296, #20882, #11100, #8326, #20461, #31112, #14909, #33907, #14701, #4320 ),
 ( #17688, #24088, #1114, #30687, #40919, #14082, #1537, #33490, #37500, #27084, #37298, #30482, #40092, #17900, #5152, #10888, #27505 ),
 ( #14283, #27292, #37099, #23875, #36895, #14492, #7713, #40513, #20676, #24293, #33700, #18107, #24496, #8116, #4522, #36680, #40714 ),
 ( #34114, #11509, #1949, #17485, #4941, #30903, #7502, #1742, #41132, #22337, #2159, #8540, #34956, #15547, #5779, #38357, #12365 ),
 ( #12150, #18733, #19159, #2374, #15958, #41972, #15119, #2793, #9172, #41557, #15750, #25353, #28122, #32163, #31744, #28955, #21500 ),
 ( #28755, #15333, #37927, #25142, #9373, #2587, #8750, #28549, #5985, #28339, #41768, #21712, #22129, #34533, #34736, #2998, #5359 ) ),
 .UNSPECIFIED., .F., .F., .F.,
 ( 4, 2, 4 ),
 ( 4, 1, 1, 1, 1, 1, 1, 1, 1, 1, 1, 1, 1, 1, 4 ),
 ( 0.000000000000000000, 0.4999999999999998890, 1.000000000000000000 ),
 ( 0.000000000000000000, 0.08300113939718137268, 0.1732806554784933895, 0.2717672377176819087, 0.3752096606209606167, 0.4787223716043260135, 0.5772295444745598747, 0.6668133826162351285, 0.7470991451079272982, 0.7815930070524458317, 0.8169452614683294644, 0.8547689062991584708, 0.8968063284581728745, 0.9447228702782888288, 1.000000000000000000 ),
 .UNSPECIFIED. ) ;
#25898 = CARTESIAN_POINT ( 'NONE',  ( 17.73882382519367695, 148.9562551477873740, 2.372964443305868087 ) ) ;
#25899 =( NAMED_UNIT ( * ) PLANE_ANGLE_UNIT ( ) SI_UNIT ( $, .RADIAN. ) );
#25900 = CIRCLE ( 'NONE', #12318, 5.080000000000006288 ) ;
#25901 = CARTESIAN_POINT ( 'NONE',  ( -8.723850037987372019, 68.58388863026053173, -1.269999999999996021 ) ) ;
#25902 = CARTESIAN_POINT ( 'NONE',  ( -5.854942301702540597, 124.9344662015456890, -0.1169956811762814242 ) ) ;
#25903 = CARTESIAN_POINT ( 'NONE',  ( -6.616342194955179501, 21.00577804425827111, -5.270772580892629122 ) ) ;
#25904 = CARTESIAN_POINT ( 'NONE',  ( 10.66982511085990204, 153.0728289088170300, 0.9866062039827817598 ) ) ;
#25905 = B_SPLINE_CURVE_WITH_KNOTS ( 'NONE', 3,
 ( #25635, #19650, #16459, #36080, #6895, #16244, #25838, #12443, #32453, #9449, #13060, #42057, #39061, #41850, #35442, #26260, #19023, #22625, #6268, #19238, #29038, #32248, #26049, #6064, #12648, #9863, #2660, #32031, #28837 ),
 .UNSPECIFIED., .F., .F.,
 ( 4, 1, 1, 1, 1, 1, 1, 2, 1, 1, 1, 1, 1, 1, 1, 1, 1, 1, 1, 1, 1, 1, 1, 1, 1, 4 ),
 ( 0.000000000000000000, 0.03307066603948304734, 0.06614133207896609468, 0.09921199811844919059, 0.1653533301974152714, 0.1984239962368983812, 0.2314946622763813522, 0.2645653283158643787, 0.3105299952961229071, 0.3564946622763812689, 0.4024593292566397418, 0.4484239962368982702, 0.5403533301974150493, 0.6322826641579321061, 0.7242119981184491628, 0.7701766650987074136, 0.8161413320789658865, 0.8850883325493537068, 0.8965794992944182695, 0.9080706660394826102, 0.9195618327845473949, 0.9310529995296121797, 0.9425441662746769644, 0.9540353330197415271, 0.9770176665098706525, 1.000000000000000000 ),
 .UNSPECIFIED. ) ;
#25906 = CARTESIAN_POINT ( 'NONE',  ( 10.46273137052124547, 157.8855781193960297, -0.6617911890761499771 ) ) ;
#25907 = DIRECTION ( 'NONE',  ( 0.000000000000000000, 1.000000000000000000, 0.000000000000000000 ) ) ;
#25908 = DIRECTION ( 'NONE',  ( 0.3256999990547864710, 0.9454731675810330582, 1.565722810161054351E-16 ) ) ;
#25909 = EDGE_CURVE ( 'NONE', #29922, #33599, #31884, .T. ) ;
#25910 = CARTESIAN_POINT ( 'NONE',  ( -23.29167281398218492, 149.3519930085110161, -0.4396919384238293094 ) ) ;
#25911 = ORIENTED_EDGE ( 'NONE', *, *, #35344, .T. ) ;
#25912 = CARTESIAN_POINT ( 'NONE',  ( 4.447838849061712452, 119.5324918327893755, -0.7507019530623586512 ) ) ;
#25913 = CARTESIAN_POINT ( 'NONE',  ( 23.34372044208193131, 149.0681261006343448, 0.4664630893998608641 ) ) ;
#25914 = CARTESIAN_POINT ( 'NONE',  ( 0.003756957834429965667, 120.7746249494737896, -0.1880135328902410030 ) ) ;
#25915 = CARTESIAN_POINT ( 'NONE',  ( 3.354142537596241702, -14.24820561377959649, 4.738596845331590757 ) ) ;
#25916 = CARTESIAN_POINT ( 'NONE',  ( -24.57769139521899149, 76.70147894597536720, 1.269999999999993578 ) ) ;
#25917 = CARTESIAN_POINT ( 'NONE',  ( 22.98446660148354681, 150.1594536303649932, 0.4849100737359565150 ) ) ;
#25918 = ORIENTED_EDGE ( 'NONE', *, *, #9662, .T. ) ;
#25919 = CARTESIAN_POINT ( 'NONE',  ( 0.7007450612751181529, 9.901275517365906609, -4.597291952374415125 ) ) ;
#25920 = CARTESIAN_POINT ( 'NONE',  ( 5.039110484533481760, 105.1218593930509826, 1.758957507424023570 ) ) ;
#25921 = CARTESIAN_POINT ( 'NONE',  ( -5.757472737270721730, 159.1136035536173097, -0.1150480073142621795 ) ) ;
#25922 = DIRECTION ( 'NONE',  ( 9.627370216492862708E-17, 1.000000000000000000, -0.000000000000000000 ) ) ;
#25923 = CARTESIAN_POINT ( 'NONE',  ( -8.046888644775119559, 121.4502209704282052, 0.8789830068023335441 ) ) ;
#25924 = CARTESIAN_POINT ( 'NONE',  ( 4.585212383536918956, 13.09695617864405470, 0.6580430208065696229 ) ) ;
#25925 = CARTESIAN_POINT ( 'NONE',  ( 15.23381565553107286, 121.5932973536894934, 1.241876992062232343 ) ) ;
#25926 = FACE_OUTER_BOUND ( 'NONE', #9183, .T. ) ;
#25928 = CARTESIAN_POINT ( 'NONE',  ( 12.96767020122738856, 121.2479969211051127, -1.095090382205327062 ) ) ;
#25927 = CARTESIAN_POINT ( 'NONE',  ( 3.056907941849938748, 108.4801157075169158, 4.214599240514290024 ) ) ;
#25929 = AXIS2_PLACEMENT_3D ( 'NONE', #22939, #622, #3602 ) ;
#25930 = CARTESIAN_POINT ( 'NONE',  ( -2.065029617914060367, 6.824861272777455135, -4.134893973632223663 ) ) ;
#25931 = CARTESIAN_POINT ( 'NONE',  ( -22.81419135200717818, 148.8343141121478652, -1.537101565576850515 ) ) ;
#25932 = EDGE_LOOP ( 'NONE', ( #28642, #6084 ) ) ;
#25933 = CARTESIAN_POINT ( 'NONE',  ( -2.986828117522290604, 156.0959049650892041, 0.3398701836618411853 ) ) ;
#25934 = CARTESIAN_POINT ( 'NONE',  ( 2.467627578834723057, -15.39586678991472546, 5.881674146221526733 ) ) ;
#25935 = CARTESIAN_POINT ( 'NONE',  ( 0.3140373394025232079, 115.7030944333331632, 1.764426444009986605 ) ) ;
#25936 = VERTEX_POINT ( 'NONE', #31849 ) ;
#25937 = CARTESIAN_POINT ( 'NONE',  ( 19.55492868859742472, 148.8045834396381508, 2.507096624874099344 ) ) ;
#25938 = DIRECTION ( 'NONE',  ( 0.1906721105965186736, -0.9816537812491066273, 0.000000000000000000 ) ) ;
#25939 = DIRECTION ( 'NONE',  ( 0.1565721916417968096, 0.9876665170007964401, 0.000000000000000000 ) ) ;
#25940 = AXIS2_PLACEMENT_3D ( 'NONE', #28737, #40903, #21908 ) ;
#25941 = AXIS2_PLACEMENT_3D ( 'NONE', #37652, #30831, #38074 ) ;
#25942 = CARTESIAN_POINT ( 'NONE',  ( -13.06303874853662528, 119.8917521002241955, 0.5243808535303264851 ) ) ;
#25943 = CARTESIAN_POINT ( 'NONE',  ( 3.811114225546782475, 116.8316721669309572, -0.2429903670874779542 ) ) ;
#25944 = EDGE_CURVE ( 'NONE', #39773, #20108, #39035, .T. ) ;
#25945 = FACE_OUTER_BOUND ( 'NONE', #27515, .T. ) ;
#25946 = APPLICATION_CONTEXT ( 'automotive_design' ) ;
#25947 = CIRCLE ( 'NONE', #15060, 3.175000000000001155 ) ;
#25948 = CARTESIAN_POINT ( 'NONE',  ( -46.77796495209232575, 25.80132671658136090, 1.441379436031522410 ) ) ;
#25949 = CARTESIAN_POINT ( 'NONE',  ( -47.29859047510723258, 25.70208046547991287, 0.1062880809757735939 ) ) ;
#25951 = ADVANCED_FACE ( 'NONE', ( #2689 ), #9478, .T. ) ;
#25950 = CARTESIAN_POINT ( 'NONE',  ( -4.862785380276537950, 117.4092208852611918, -1.165888418928414216 ) ) ;
#25952 = CARTESIAN_POINT ( 'NONE',  ( -47.20791569504335428, 21.28685671521062517, 4.803936552638831792 ) ) ;
#25953 = DIRECTION ( 'NONE',  ( -0.8745520943968235761, 0.4849315768086558398, -4.268512490100410909E-16 ) ) ;
#25954 = CARTESIAN_POINT ( 'NONE',  ( -4.668965673006310269, 118.0244993202197605, 0.5693437839270533152 ) ) ;
#25955 = CARTESIAN_POINT ( 'NONE',  ( -58.37241122568488549, -0.2962816677227891882, -1.035588846938697759E-14 ) ) ;
#25956 = ORIENTED_EDGE ( 'NONE', *, *, #14101, .T. ) ;
#25957 = ORIENTED_EDGE ( 'NONE', *, *, #36760, .T. ) ;
#25958 = DIRECTION ( 'NONE',  ( -0.000000000000000000, -0.000000000000000000, -1.000000000000000000 ) ) ;
#25959 = CARTESIAN_POINT ( 'NONE',  ( -3.637648525249608245, 118.8078150821789905, -0.9359800040424770540 ) ) ;
#25960 = CARTESIAN_POINT ( 'NONE',  ( -7.643874070029948342, 124.9344662015457317, -0.1527427953284560547 ) ) ;
#25961 = CARTESIAN_POINT ( 'NONE',  ( 4.807312038368031892, 117.8307531015728529, 0.8998899155070840816 ) ) ;
#25962 = DIRECTION ( 'NONE',  ( -1.000000000000000000, 0.000000000000000000, 0.000000000000000000 ) ) ;
#25963 = CARTESIAN_POINT ( 'NONE',  ( -5.176742542608756104, 120.9449653624321144, -0.6121131393098594442 ) ) ;
#25964 = CARTESIAN_POINT ( 'NONE',  ( -1.848033302852856385, 115.7026900523373456, -1.721337056304435675 ) ) ;
#25965 = CARTESIAN_POINT ( 'NONE',  ( -0.1701498899198997661, 105.9761672132488570, 5.294459536038139014 ) ) ;
#25966 = CARTESIAN_POINT ( 'NONE',  ( -8.473844426907701788, 67.77203500197072117, -1.523999999999995802 ) ) ;
#25967 = CARTESIAN_POINT ( 'NONE',  ( 5.205184729905183438, 115.4673366222922368, -1.303740999714490201 ) ) ;
#25968 = CARTESIAN_POINT ( 'NONE',  ( -7.970993357304875460, 121.6949282028273132, -1.099362369368161785 ) ) ;
#25969 = CARTESIAN_POINT ( 'NONE',  ( 22.76738278397251136, 137.3906169244638136, 0.4549464913834384561 ) ) ;
#25970 = CARTESIAN_POINT ( 'NONE',  ( -0.009747742627877935620, 156.3581291470199233, 0.4878169013068173743 ) ) ;
#25971 = CARTESIAN_POINT ( 'NONE',  ( -2.676945639826796786, 115.7033391084184899, 1.585126308171322496 ) ) ;
#25972 = CARTESIAN_POINT ( 'NONE',  ( -12.83038717616591029, 133.7433341693027842, -0.1947450472242223951 ) ) ;
#25973 = CARTESIAN_POINT ( 'NONE',  ( 1.104432469574216480, -9.427232690354344413, -4.492858291722996888 ) ) ;
#25975 = ORIENTED_EDGE ( 'NONE', *, *, #38073, .F. ) ;
#25974 = CARTESIAN_POINT ( 'NONE',  ( 15.60190333658766981, 121.2802728028965475, 0.9237637308081629861 ) ) ;
#25976 = DIRECTION ( 'NONE',  ( -0.8745520943968249084, 0.4849315768086533418, -5.311926654347176508E-16 ) ) ;
#25977 = CARTESIAN_POINT ( 'NONE',  ( 2.255636784185061749, -15.37476536804864580, 5.049411959999403621 ) ) ;
#25978 = CARTESIAN_POINT ( 'NONE',  ( -11.84733475906203104, 122.5845257805695923, 1.288679497020477127 ) ) ;
#25979 = CARTESIAN_POINT ( 'NONE',  ( 0.8080343152487895475, 3.801264818822497560, -0.5430376807499140979 ) ) ;
#25980 = CARTESIAN_POINT ( 'NONE',  ( -23.12143742665070434, 148.7607265879045144, -1.192451864686425500 ) ) ;
#25981 = AXIS2_PLACEMENT_3D ( 'NONE', #27548, #27336, #11142 ) ;
#25982 = CARTESIAN_POINT ( 'NONE',  ( 0.2615529312792121419, 0.9453775857588032627, -0.9394305312888860948 ) ) ;
#25983 = ORIENTED_EDGE ( 'NONE', *, *, #12591, .F. ) ;
#25984 = ORIENTED_EDGE ( 'NONE', *, *, #4529, .T. ) ;
#25985 = CARTESIAN_POINT ( 'NONE',  ( -46.67338572489354931, 16.85372243840488338, -6.574220250756231762E-15 ) ) ;
#25986 = CARTESIAN_POINT ( 'NONE',  ( 1.365700293149759492, 106.2535611835979239, 5.166841330979377034 ) ) ;
#25987 = CARTESIAN_POINT ( 'NONE',  ( -4.473055752542836494, 120.8671296916768227, 0.3242568198034687654 ) ) ;
#25988 = CARTESIAN_POINT ( 'NONE',  ( 1.960603841440088146, -15.05276691075377293, 5.730201639535507319 ) ) ;
#25989 = CARTESIAN_POINT ( 'NONE',  ( 6.615874392072679910, 120.4115791468657903, -0.8913422009562909087 ) ) ;
#25990 = CARTESIAN_POINT ( 'NONE',  ( -12.56843540011194094, 155.2353133052689032, -2.219430909113760730 ) ) ;
#25991 = DIRECTION ( 'NONE',  ( 0.4849315768086534528, 0.8745520943968250194, 1.030032898892974942E-16 ) ) ;
#25992 = CARTESIAN_POINT ( 'NONE',  ( 2.769760999665409340, -14.92388480464812872, 4.423285184949336646 ) ) ;
#25993 = CARTESIAN_POINT ( 'NONE',  ( 0.008457519121113112742, 39.20946620154573026, -0.4232488410869263418 ) ) ;
#25994 = CARTESIAN_POINT ( 'NONE',  ( 10.50161782422432921, 126.1106773019354819, -0.1489875947030158132 ) ) ;
#25995 = ORIENTED_EDGE ( 'NONE', *, *, #6887, .F. ) ;
#25996 = AXIS2_PLACEMENT_3D ( 'NONE', #4142, #24123, #946 ) ;
#25997 = CARTESIAN_POINT ( 'NONE',  ( -20.79116009376201646, 79.67004825550966984, 1.269999999999995133 ) ) ;
#25998 = CARTESIAN_POINT ( 'NONE',  ( -20.79116009376201646, 79.67004825550966984, 1.523999999999995358 ) ) ;
#25999 = CARTESIAN_POINT ( 'NONE',  ( -58.73303099470203392, -0.3138845496159919923, 0.2515151591903359574 ) ) ;
#26000 = DIRECTION ( 'NONE',  ( -0.1728608224830406603, -0.000000000000000000, -0.9849462604886047856 ) ) ;
#26001 = CARTESIAN_POINT ( 'NONE',  ( 16.23473294303248338, 121.3954344197762083, 0.2182100806314835051 ) ) ;
#26002 = CARTESIAN_POINT ( 'NONE',  ( -5.284833012248508766, 116.4655405006298849, 0.8823810258511327609 ) ) ;
#26003 = VECTOR ( 'NONE', #2583, 1000.000000000000000 ) ;
#26004 = DIRECTION ( 'NONE',  ( -9.627370216492862708E-17, -1.000000000000000000, 0.000000000000000000 ) ) ;
#26005 = DIRECTION ( 'NONE',  ( 0.9998004120163608288, 0.000000000000000000, 0.01997839162482760791 ) ) ;
#26006 = CARTESIAN_POINT ( 'NONE',  ( -3.742012044685256722, 31.40836143976739336, -0.4637063799314742329 ) ) ;
#26007 = EDGE_CURVE ( 'NONE', #7000, #28177, #15879, .T. ) ;
#26008 = CARTESIAN_POINT ( 'NONE',  ( 0.4079906055175022139, 117.9789173577105572, 0.5621165275234438763 ) ) ;
#26009 = CARTESIAN_POINT ( 'NONE',  ( -4.295268622494708310, 18.69437521248495671, 1.722957355393906598 ) ) ;
#26010 = CARTESIAN_POINT ( 'NONE',  ( 8.340720164204880049, -15.19402286670749191, -1.049415519506536665 ) ) ;
#26011 = CARTESIAN_POINT ( 'NONE',  ( -5.481623637317887265, 117.2526226941921834, -0.8295243230819944191 ) ) ;
#26012 = CARTESIAN_POINT ( 'NONE',  ( -0.1346051971226650268, 106.5118632461160217, -5.080372420286161095 ) ) ;
#26013 = DIRECTION ( 'NONE',  ( 0.8745520943968235761, -0.4849315768086558398, 8.537024980200821818E-16 ) ) ;
#26014 = CARTESIAN_POINT ( 'NONE',  ( 3.113094358168766451, 108.2626774329659440, -4.181916884918123856 ) ) ;
#26015 = CARTESIAN_POINT ( 'NONE',  ( 1.938979755385511261, 104.6144662015456817, 4.428504999821790022 ) ) ;
#26016 = CARTESIAN_POINT ( 'NONE',  ( 4.256838582791900194, 16.71066835407712858, 1.825063967593055558 ) ) ;
#26017 = CARTESIAN_POINT ( 'NONE',  ( -15.50061618130080987, 62.14374591690594940, 1.904999999999990035 ) ) ;
#26018 = DIRECTION ( 'NONE',  ( 2.664535259100375697E-15, 0.000000000000000000, 1.000000000000000000 ) ) ;
#26019 = CARTESIAN_POINT ( 'NONE',  ( 3.221735024265227398, -14.36526069886394730, 2.718910799868354378 ) ) ;
#26020 = CARTESIAN_POINT ( 'NONE',  ( 1.613589725761565008, 119.1892773189224783, -0.6629358561546615514 ) ) ;
#26021 = CARTESIAN_POINT ( 'NONE',  ( -1.937878880890249844, 116.8467566806161386, 0.3061478142745881481 ) ) ;
#26022 = CIRCLE ( 'NONE', #34193, 0.2540000000000000036 ) ;
#26023 = VERTEX_POINT ( 'NONE', #38251 ) ;
#26024 = CARTESIAN_POINT ( 'NONE',  ( 5.475330206976777525, 77.01756249999996840, 5.107412922131463695 ) ) ;
#26025 = ORIENTED_EDGE ( 'NONE', *, *, #24468, .F. ) ;
#26026 = CARTESIAN_POINT ( 'NONE',  ( -3.046231754824816118, 31.09810386281187533, 0.4001267285823233433 ) ) ;
#26027 = CARTESIAN_POINT ( 'NONE',  ( 2.279390105945505507, -15.60765617898064761, 5.834426787525912594 ) ) ;
#26028 = CARTESIAN_POINT ( 'NONE',  ( -11.46709954559049649, 121.1873859956591843, 1.221572053168039185 ) ) ;
#26029 = CARTESIAN_POINT ( 'NONE',  ( 0.02399864187730012949, 159.1630378086529731, -1.200990174154242363 ) ) ;
#26030 = CARTESIAN_POINT ( 'NONE',  ( 3.700881553190929374, 8.714383148187751615, -2.768892949411812854 ) ) ;
#26031 = CARTESIAN_POINT ( 'NONE',  ( -58.55703382916102129, -0.1428860932337914225, -0.5663864201305394142 ) ) ;
#26032 = ORIENTED_EDGE ( 'NONE', *, *, #25035, .T. ) ;
#26033 = CARTESIAN_POINT ( 'NONE',  ( 5.078986093043053707, 97.88346620154572975, 0.1014902294541244060 ) ) ;
#26034 = CARTESIAN_POINT ( 'NONE',  ( 0.4066243552752198398, 124.0591982226670211, 0.1013866577921580941 ) ) ;
#26035 = SURFACE_STYLE_FILL_AREA ( #23033 ) ;
#26036 = CARTESIAN_POINT ( 'NONE',  ( -15.29320056080895007, 150.6904849259475441, 1.473493523582195319 ) ) ;
#26037 = DIRECTION ( 'NONE',  ( -0.7770581983690896255, 0.6294287539883960392, -4.360450048231423821E-16 ) ) ;
#26038 = CARTESIAN_POINT ( 'NONE',  ( 18.50101540898958774, 149.0103496150362901, -1.723905467370217215 ) ) ;
#26039 = CARTESIAN_POINT ( 'NONE',  ( -6.769736154946738083, 118.6475953829349379, -1.187203428762516166 ) ) ;
#26040 = CARTESIAN_POINT ( 'NONE',  ( -58.87911280034276018, -0.2081424763510641984, -1.061797465414398100E-14 ) ) ;
#26041 = VERTEX_POINT ( 'NONE', #42086 ) ;
#26042 = CARTESIAN_POINT ( 'NONE',  ( 4.415775866151314233, 118.1645749254845441, -0.4805746343930200060 ) ) ;
#26043 = CARTESIAN_POINT ( 'NONE',  ( 10.78632646169009490, 153.0872561326487187, -0.6669751843662026225 ) ) ;
#26044 = ORIENTED_EDGE ( 'NONE', *, *, #37027, .F. ) ;
#26045 = CARTESIAN_POINT ( 'NONE',  ( -3.403275764582950114, 119.7942873563901713, -0.7909988017435811702 ) ) ;
#26046 = CARTESIAN_POINT ( 'NONE',  ( 3.790367410748021637, -15.17722879538144198, -0.1767333597861489025 ) ) ;
#26047 = EDGE_CURVE ( 'NONE', #10071, #120, #18845, .T. ) ;
#26048 = VECTOR ( 'NONE', #36363, 1000.000000000000227 ) ;
#26049 = CARTESIAN_POINT ( 'NONE',  ( -57.47393550255003447, 1.325481720219581661, -1.020368242535414227E-14 ) ) ;
#26050 = EDGE_CURVE ( 'NONE', #2334, #11330, #23718, .T. ) ;
#26051 = CARTESIAN_POINT ( 'NONE',  ( -4.843782464516869446, 117.6435980591638355, 0.9175585232979758255 ) ) ;
#26052 = CARTESIAN_POINT ( 'NONE',  ( 14.38208595515599875, 131.1674235819977241, 1.945708262771123076 ) ) ;
#26053 = FACE_OUTER_BOUND ( 'NONE', #20428, .T. ) ;
#26054 = EDGE_CURVE ( 'NONE', #15866, #4432, #37462, .T. ) ;
#26055 = CARTESIAN_POINT ( 'NONE',  ( -4.349660437102230048, 31.17966527223318707, -1.615541842050199461 ) ) ;
#26056 = CARTESIAN_POINT ( 'NONE',  ( 7.044359374033473564, 122.0696255612902519, 0.2151282384624544075 ) ) ;
#26057 = CARTESIAN_POINT ( 'NONE',  ( -5.451267667241070720E-14, 85.80437499999999318, 0.000000000000000000 ) ) ;
#26058 = CARTESIAN_POINT ( 'NONE',  ( -48.39470387610976587, 16.07729130905085313, -1.622931888101232678 ) ) ;
#26059 = CARTESIAN_POINT ( 'NONE',  ( 2.185374947706846704, 116.1939849232089443, -0.02259167694784758318 ) ) ;
#26060 = DIRECTION ( 'NONE',  ( 0.9998004120163608288, 0.000000000000000000, 0.01997839162482736852 ) ) ;
#26061 = AXIS2_PLACEMENT_3D ( 'NONE', #15063, #11882, #24871 ) ;
#26062 = CARTESIAN_POINT ( 'NONE',  ( -46.68342141079460106, 26.02334812023122268, -1.327713788494189862 ) ) ;
#26063 = CARTESIAN_POINT ( 'NONE',  ( -47.85244527695896011, 19.39403540832957518, 5.219971639306693056 ) ) ;
#26064 = CARTESIAN_POINT ( 'NONE',  ( -8.567664903271650090, 118.7102832696748607, -1.176849739173866594 ) ) ;
#26065 = CARTESIAN_POINT ( 'NONE',  ( -5.305748947172302721, 77.01756250000002524, 5.247078976224250013 ) ) ;
#26066 = CARTESIAN_POINT ( 'NONE',  ( -5.941750550382311147, 57.15000000000365077, 5.016500000000000625 ) ) ;
#26067 = DIRECTION ( 'NONE',  ( -0.01997839162482737546, -1.040247600000940825E-18, 0.9998004120163610509 ) ) ;
#26068 = CARTESIAN_POINT ( 'NONE',  ( -57.37345908981379949, 3.796002467274087078, 0.9053535129858855113 ) ) ;
#26069 = CARTESIAN_POINT ( 'NONE',  ( -57.64973313486724038, 1.352533784701764885, 1.499908592384902706 ) ) ;
#26070 = EDGE_CURVE ( 'NONE', #22433, #30888, #3531, .T. ) ;
#26071 = CARTESIAN_POINT ( 'NONE',  ( -14.75425959148295618, 120.3062992333385921, -0.06863422566743775100 ) ) ;
#26072 = AXIS2_PLACEMENT_3D ( 'NONE', #29570, #10387, #32984 ) ;
#26073 = ORIENTED_EDGE ( 'NONE', *, *, #36656, .T. ) ;
#26074 = CARTESIAN_POINT ( 'NONE',  ( -51.09183723991096571, 15.73968240350219538, -4.743875354843006598 ) ) ;
#26075 = CARTESIAN_POINT ( 'NONE',  ( 6.060350493389893067, 121.4410810028806509, 0.1068649412279469996 ) ) ;
#26076 = ORIENTED_EDGE ( 'NONE', *, *, #13555, .T. ) ;
#26077 = DIRECTION ( 'NONE',  ( -5.188838149069471174E-16, 1.699382548006136313E-16, 1.000000000000000000 ) ) ;
#26078 = CARTESIAN_POINT ( 'NONE',  ( -11.17680165766864775, 128.1157469881088105, -0.4152311708251573696 ) ) ;
#26079 = CARTESIAN_POINT ( 'NONE',  ( 5.218988718559132600, -14.41095047787725747, 3.833162268628383718 ) ) ;
#26080 = CARTESIAN_POINT ( 'NONE',  ( -9.254844111043031063, 119.0402042963619351, 0.8977872906997166336 ) ) ;
#26081 = CARTESIAN_POINT ( 'NONE',  ( -5.078986093043186045, 91.53346620154573543, -0.1014902294541237954 ) ) ;
#26082 = AXIS2_PLACEMENT_3D ( 'NONE', #15210, #12022, #34613 ) ;
#26083 = CARTESIAN_POINT ( 'NONE',  ( 1.410028229074493433, 159.6020224343070026, 0.1582310832764451114 ) ) ;
#26084 = CARTESIAN_POINT ( 'NONE',  ( 15.72120838691553502, 146.8976252958255486, 0.4481387442112281794 ) ) ;
#26085 = CARTESIAN_POINT ( 'NONE',  ( 4.829493779578470480, 118.5266822147775940, -0.7638424752985826238 ) ) ;
#26086 = CARTESIAN_POINT ( 'NONE',  ( -0.02445332296907207215, 6.119348097484421878, 0.9755048060674135213 ) ) ;
#26087 = CARTESIAN_POINT ( 'NONE',  ( -16.18495160125072374, 121.3864332154274877, -0.4845229560194668217 ) ) ;
#26088 = DIRECTION ( 'NONE',  ( -0.000000000000000000, -1.000000000000000000, -0.000000000000000000 ) ) ;
#26089 = DIRECTION ( 'NONE',  ( -6.353134868986659519E-16, 1.000000000000000000, 0.000000000000000000 ) ) ;
#26090 = ORIENTED_EDGE ( 'NONE', *, *, #26205, .T. ) ;
#26091 = CARTESIAN_POINT ( 'NONE',  ( 8.585969666846875015, 118.6243502972331498, 1.142660147408910642 ) ) ;
#26093 = ADVANCED_FACE ( 'NONE', ( #35687 ), #11807, .F. ) ;
#26092 = ORIENTED_EDGE ( 'NONE', *, *, #16981, .T. ) ;
#26094 = CARTESIAN_POINT ( 'NONE',  ( 14.95453923199683111, 61.75387968257833649, 5.016499999999999737 ) ) ;
#26095 = CARTESIAN_POINT ( 'NONE',  ( 14.34163035669542197, 121.9874158357064857, 1.600522166921893863 ) ) ;
#26096 = CARTESIAN_POINT ( 'NONE',  ( 10.04363327864678190, 120.6268241347409855, -1.191437567882422943 ) ) ;
#26097 = CARTESIAN_POINT ( 'NONE',  ( 0.5118484794875378663, 4.451237885527871363, -0.8280682483750020362 ) ) ;
#26098 = CARTESIAN_POINT ( 'NONE',  ( -8.372926607701892010, 8.771278641329313785, 0.9163881402227073147 ) ) ;
#26099 = CARTESIAN_POINT ( 'NONE',  ( -21.36223069762263194, 149.8571540977637255, -2.130384393597193782 ) ) ;
#26100 = CARTESIAN_POINT ( 'NONE',  ( 4.783395520282055280, 117.8481480307013385, -0.7930544963161749727 ) ) ;
#26101 = CARTESIAN_POINT ( 'NONE',  ( 5.183518906920014935, 115.4398124677065596, 1.515634836823672060 ) ) ;
#26102 = EDGE_CURVE ( 'NONE', #20793, #9715, #35471, .T. ) ;
#26103 = CARTESIAN_POINT ( 'NONE',  ( 8.687188811298828028, 122.3401343867201945, -0.7349857017399258341 ) ) ;
#26104 = CARTESIAN_POINT ( 'NONE',  ( -15.26332761227469881, 148.0152273645666980, -0.2540164781927347626 ) ) ;
#26105 = ORIENTED_EDGE ( 'NONE', *, *, #19897, .F. ) ;
#26106 = CARTESIAN_POINT ( 'NONE',  ( -1.300143943178302841, 119.1766673560425858, -0.6697961403939315383 ) ) ;
#26107 = CARTESIAN_POINT ( 'NONE',  ( 2.247313541653549240, -15.69307202063721718, 5.732350583303913893 ) ) ;
#26108 = CARTESIAN_POINT ( 'NONE',  ( -28.09515292912719175, 77.51021392068167870, -1.270000000000007345 ) ) ;
#26109 = EDGE_CURVE ( 'NONE', #16254, #33959, #11136, .T. ) ;
#26110 = CARTESIAN_POINT ( 'NONE',  ( -44.36446822842629700, 21.81554158013422651, -2.896954608336749892 ) ) ;
#26111 = VERTEX_POINT ( 'NONE', #26081 ) ;
#26112 = CIRCLE ( 'NONE', #7758, 5.588000000000006295 ) ;
#26113 = CARTESIAN_POINT ( 'NONE',  ( 5.054692016413384614, 119.8577235299091228, 1.014870397641471911 ) ) ;
#26114 = CARTESIAN_POINT ( 'NONE',  ( 3.682264917456192332, 88.99346620154574339, 0.07358041635423968885 ) ) ;
#26115 = CARTESIAN_POINT ( 'NONE',  ( -6.059261036834472591, 57.14999999999998437, 5.016499999999999737 ) ) ;
#26116 = AXIS2_PLACEMENT_3D ( 'NONE', #33770, #26526, #26740 ) ;
#26117 = CARTESIAN_POINT ( 'NONE',  ( -3.201024870708126357, 118.2446163226072713, 0.7148959180058855889 ) ) ;
#26118 = CARTESIAN_POINT ( 'NONE',  ( -5.435345482397000438, 30.30303275347894854, -6.432456514813170045 ) ) ;
#26119 = CARTESIAN_POINT ( 'NONE',  ( 15.71402047398548874, 147.5983985311728759, 1.037567014598419712 ) ) ;
#26120 = CARTESIAN_POINT ( 'NONE',  ( 1.973526102370556146, 116.9869758084673208, -0.3704244399607082849 ) ) ;
#26121 = CARTESIAN_POINT ( 'NONE',  ( -47.59458007651616640, 19.66657808744393066, -5.176039278150066814 ) ) ;
#26122 = TOROIDAL_SURFACE ( 'NONE', #9793, 0.3810000000000000608, 0.2540000000000000036 ) ;
#26123 = AXIS2_PLACEMENT_3D ( 'NONE', #16345, #19745, #6360 ) ;
#26124 = CARTESIAN_POINT ( 'NONE',  ( 15.70103477329399766, 145.5797129992483292, 0.3137440411564567100 ) ) ;
#26125 = EDGE_CURVE ( 'NONE', #39961, #11997, #41989, .T. ) ;
#26126 = CARTESIAN_POINT ( 'NONE',  ( -18.63485108555828873, 154.1203422869290023, -0.3484461891417473534 ) ) ;
#26127 = VERTEX_POINT ( 'NONE', #16490 ) ;
#26128 = CARTESIAN_POINT ( 'NONE',  ( 7.959411891889985213, 121.8595877113556156, -0.7022647005503769302 ) ) ;
#26129 = CARTESIAN_POINT ( 'NONE',  ( 2.664264518795053327, -15.44973899589986566, 5.798575810372247119 ) ) ;
#26130 = CIRCLE ( 'NONE', #14568, 14.73199999999999577 ) ;
#26131 = CARTESIAN_POINT ( 'NONE',  ( -14.42924251737987262, 139.0941462050048187, -0.8894241721302191817 ) ) ;
#26132 = CARTESIAN_POINT ( 'NONE',  ( 3.866302502687585907, -14.02971062843458228, 4.478402296968817531 ) ) ;
#26133 = CARTESIAN_POINT ( 'NONE',  ( -32.35036891424130090, 51.35816619018828533, 1.523999999999994692 ) ) ;
#26134 = CARTESIAN_POINT ( 'NONE',  ( 3.302029177305205732, 159.4671159221996959, 0.06598240135525389183 ) ) ;
#26135 = ORIENTED_EDGE ( 'NONE', *, *, #26690, .T. ) ;
#26136 = CARTESIAN_POINT ( 'NONE',  ( -4.274281473441157608, 3.541781053574249327, 1.790774723582081451 ) ) ;
#26137 = CARTESIAN_POINT ( 'NONE',  ( -9.822473411059320370, 117.9943479623217399, -0.1962763949404990327 ) ) ;
#26138 = CARTESIAN_POINT ( 'NONE',  ( -17.82828877264048373, 64.92754330167842625, -1.270000000000000018 ) ) ;
#26139 = DIRECTION ( 'NONE',  ( 6.353134868986659519E-16, -1.000000000000000000, 0.000000000000000000 ) ) ;
#26140 = EDGE_CURVE ( 'NONE', #22436, #30491, #22677, .T. ) ;
#26141 = CARTESIAN_POINT ( 'NONE',  ( -5.756513278485710927, 120.0202605514778185, 0.8483401204354447112 ) ) ;
#26142 = CARTESIAN_POINT ( 'NONE',  ( 3.900846188197024667, 12.44727460162280863, 2.488979119290085862 ) ) ;
#26143 = CARTESIAN_POINT ( 'NONE',  ( 18.04579964447621876, 154.0913862843578670, 1.474566393615006854 ) ) ;
#26144 = CARTESIAN_POINT ( 'NONE',  ( -0.09221630143976956850, 107.6766875080336376, 4.614880812453268533 ) ) ;
#26146 = CARTESIAN_POINT ( 'NONE',  ( 0.4301208033649062124, 117.9789173577105572, -0.5453690669796713575 ) ) ;
#26145 = CARTESIAN_POINT ( 'NONE',  ( 4.966122758792402614, 56.51499999999995083, 4.710630977848971668 ) ) ;
#26147 = CARTESIAN_POINT ( 'NONE',  ( 4.309711357183296343, 3.151582320728117725, 1.677628897243969464 ) ) ;
#26148 = CARTESIAN_POINT ( 'NONE',  ( -22.64839633469834013, 142.3612397021088611, -1.542087416992683924 ) ) ;
#26149 = ORIENTED_EDGE ( 'NONE', *, *, #32316, .T. ) ;
#26150 = CARTESIAN_POINT ( 'NONE',  ( -1.578387894090459653, 120.8584627942791627, 0.1358179495115143243 ) ) ;
#26151 = EDGE_CURVE ( 'NONE', #24227, #23040, #2973, .T. ) ;
#26152 = CARTESIAN_POINT ( 'NONE',  ( 5.858142917232623148, -13.84584594667595603, 2.526540219170608115 ) ) ;
#26153 = FACE_OUTER_BOUND ( 'NONE', #24471, .T. ) ;
#26154 = EDGE_CURVE ( 'NONE', #32528, #18094, #33400, .T. ) ;
#26155 = CARTESIAN_POINT ( 'NONE',  ( -2.611003341877406125, 107.7052943677586967, -4.533873330392383494 ) ) ;
#26156 = EDGE_LOOP ( 'NONE', ( #15718, #34942, #21199, #30163 ) ) ;
#26157 = CARTESIAN_POINT ( 'NONE',  ( 19.13882315974079873, 148.9694856701144090, 2.502273048283856660 ) ) ;
#26158 = CARTESIAN_POINT ( 'NONE',  ( 9.094996104468812348, 78.64197151092923832, 5.392902600000138769 ) ) ;
#26159 = FACE_OUTER_BOUND ( 'NONE', #29491, .T. ) ;
#26160 = CARTESIAN_POINT ( 'NONE',  ( -5.858194661467491571, 117.3723397083485622, 0.4592760973624645526 ) ) ;
#26161 = CARTESIAN_POINT ( 'NONE',  ( 3.265120802789828858, 159.4600617640778353, -0.2122772200314291535 ) ) ;
#26162 = CARTESIAN_POINT ( 'NONE',  ( 3.682264917456192332, 91.53346620154573543, 0.07358041635424013294 ) ) ;
#26163 = CARTESIAN_POINT ( 'NONE',  ( -46.63086599321469095, 26.12812040998877450, 1.284766365014880840 ) ) ;
#26164 = CARTESIAN_POINT ( 'NONE',  ( -49.54051387650593341, 20.87470723125096228, 2.270501476849533518 ) ) ;
#26165 = CARTESIAN_POINT ( 'NONE',  ( 2.085304100370665381, -15.07063515923644204, 5.677967908721369916 ) ) ;
#26166 = CARTESIAN_POINT ( 'NONE',  ( -53.75224695799815322, 9.373383622779334345, 3.688627211158417296 ) ) ;
#26167 = CARTESIAN_POINT ( 'NONE',  ( -58.82991074935231524, -0.2577531494038359794, -1.058401375502683064E-14 ) ) ;
#26168 = CARTESIAN_POINT ( 'NONE',  ( -4.683796573410287323, 118.0096004882185809, 0.5957989904303049311 ) ) ;
#26169 = CARTESIAN_POINT ( 'NONE',  ( -58.37241122568487128, -0.2962816677227614326, -1.020154024344285766E-14 ) ) ;
#26170 = ORIENTED_EDGE ( 'NONE', *, *, #33993, .T. ) ;
#26171 = CARTESIAN_POINT ( 'NONE',  ( -8.371648177948166847, 119.6424059396060215, -1.420761012106893650 ) ) ;
#26172 = CARTESIAN_POINT ( 'NONE',  ( -7.588497335288529655, 124.2943531750336490, -0.1606663149101727195 ) ) ;
#26173 = CARTESIAN_POINT ( 'NONE',  ( 4.829999151938469737, 117.7605300480266521, 0.9794162057613182704 ) ) ;
#26174 = CARTESIAN_POINT ( 'NONE',  ( -47.29859047510723258, 25.70208046547991287, -0.1062880809757916212 ) ) ;
#26175 = CARTESIAN_POINT ( 'NONE',  ( -10.62861998609546710, 124.7671305375842934, -1.166658412819147728 ) ) ;
#26176 = CARTESIAN_POINT ( 'NONE',  ( -3.658446277643336852, 115.7029863456469769, -1.617048514123410108 ) ) ;
#26177 = CARTESIAN_POINT ( 'NONE',  ( -6.059261036834476144, 56.51499999999998636, 4.381499999999999950 ) ) ;
#26178 = CARTESIAN_POINT ( 'NONE',  ( 9.132817075745611705E-16, 9.026346327358515609, 0.000000000000000000 ) ) ;
#26179 = CARTESIAN_POINT ( 'NONE',  ( 5.597156320496667448, 117.9391977826196296, -0.5238424959023464389 ) ) ;
#26180 = CARTESIAN_POINT ( 'NONE',  ( -16.96873827569995186, 146.4457527449227143, -1.929048950080525904 ) ) ;
#26181 = PRESENTATION_STYLE_ASSIGNMENT (( #3628 ) ) ;
#26182 = CARTESIAN_POINT ( 'NONE',  ( -6.905625000000052971, 85.80437499999999318, 8.456951552361939290E-16 ) ) ;
#26183 = CARTESIAN_POINT ( 'NONE',  ( -3.653537934457985692, 115.7029491755470900, 1.478493708770651560 ) ) ;
#26184 = CARTESIAN_POINT ( 'NONE',  ( -15.76292520415746168, 145.9043202870795994, -0.2477380866161832118 ) ) ;
#26185 = CARTESIAN_POINT ( 'NONE',  ( -1.251853189678833411, -4.679435864505671283, 4.458631606201990394 ) ) ;
#26187 = ORIENTED_EDGE ( 'NONE', *, *, #41797, .T. ) ;
#26186 = CARTESIAN_POINT ( 'NONE',  ( 22.97411545401776323, 149.2143936249396461, 1.313106760764511272 ) ) ;
#26188 = DIRECTION ( 'NONE',  ( -0.9998004120163609398, 0.000000000000000000, -0.01997839162482749689 ) ) ;
#26189 = CARTESIAN_POINT ( 'NONE',  ( 3.668568818830479028, -15.43917834477946727, 2.972162690469843049 ) ) ;
#26190 = CARTESIAN_POINT ( 'NONE',  ( -6.044862153450532460, 157.1185343457808301, 1.711190705598350625 ) ) ;
#26191 = CARTESIAN_POINT ( 'NONE',  ( 0.7602462924416659718, 13.52415170902173891, -0.6087277422976011820 ) ) ;
#26192 = CARTESIAN_POINT ( 'NONE',  ( -23.13850227319436925, 149.2833505036244048, -1.057685438456114735 ) ) ;
#26193 = CARTESIAN_POINT ( 'NONE',  ( 0.9725752971277935588, -10.50039532299128808, -0.08436647605774086345 ) ) ;
#26194 = VERTEX_POINT ( 'NONE', #17018 ) ;
#26195 = ORIENTED_EDGE ( 'NONE', *, *, #7941, .T. ) ;
#26196 = CARTESIAN_POINT ( 'NONE',  ( -43.13073682054402269, 20.84535665847938546, -5.417716557342317191E-15 ) ) ;
#26197 = CARTESIAN_POINT ( 'NONE',  ( 4.713882987175320949, 112.7966860322829206, 2.559857038700545928 ) ) ;
#26198 = APPLICATION_PROTOCOL_DEFINITION ( 'draft international standard', 'automotive_design', 1998, #35495 ) ;
#26199 = AXIS2_PLACEMENT_3D ( 'NONE', #36207, #39400, #1062 ) ;
#26200 = CARTESIAN_POINT ( 'NONE',  ( -12.68314523066112365, 130.7634385742845780, 0.6346334167959437611 ) ) ;
#26201 = CARTESIAN_POINT ( 'NONE',  ( 3.088592312018083152, -14.58504802601380490, 5.263618629775349333 ) ) ;
#26202 = CARTESIAN_POINT ( 'NONE',  ( 12.17146470397773683, 153.5325627063460843, -1.540419412064476079 ) ) ;
#26203 = CARTESIAN_POINT ( 'NONE',  ( -11.23789960528901233, 121.3367100885591015, -1.694033198309415900 ) ) ;
#26204 = CARTESIAN_POINT ( 'NONE',  ( -7.917360960270791281, 70.00264313970245666, -1.523999999999995802 ) ) ;
#26205 = EDGE_CURVE ( 'NONE', #38326, #34680, #26784, .T. ) ;
#26206 = CARTESIAN_POINT ( 'NONE',  ( 2.681353593581013328, -14.83682625404381028, 4.634604895792218571 ) ) ;
#26207 = CARTESIAN_POINT ( 'NONE',  ( -3.326449069927084778, 34.44917962613040885, 2.810111972534369507 ) ) ;
#26208 = CARTESIAN_POINT ( 'NONE',  ( 15.28485850284622494, 148.0141687878753203, 0.07717638215565311710 ) ) ;
#26209 = EDGE_LOOP ( 'NONE', ( #39776, #31556, #16563, #28942, #1028 ) ) ;
#26210 = CARTESIAN_POINT ( 'NONE',  ( -3.441191703046090566, 108.4907222760747487, 4.068004305127732145 ) ) ;
#26211 = CARTESIAN_POINT ( 'NONE',  ( 0.1714814745455566780, 105.9763118359762188, 5.301227498240227654 ) ) ;
#26212 = LINE ( 'NONE', #6421, #19115 ) ;
#26213 = CARTESIAN_POINT ( 'NONE',  ( -58.76944392236323012, -0.3049061203703323786, 0.2000781065762422262 ) ) ;
#26214 = CARTESIAN_POINT ( 'NONE',  ( 21.90070483041502669, 151.4392833230981239, 0.2858324510978372257 ) ) ;
#26215 = CARTESIAN_POINT ( 'NONE',  ( -3.592701615362679846, 108.6576027043044377, 3.989964801148524476 ) ) ;
#26216 = CARTESIAN_POINT ( 'NONE',  ( -0.5401806786426563978, 115.6909491485452435, 1.744860971564218932 ) ) ;
#26217 = CARTESIAN_POINT ( 'NONE',  ( 4.560443952884764229, -11.68867000232777542, 0.6947937212093100445 ) ) ;
#26218 = CARTESIAN_POINT ( 'NONE',  ( -2.234863377544184626, 32.75332796031084115, 0.9421588083577628892 ) ) ;
#26219 = CARTESIAN_POINT ( 'NONE',  ( 20.99120442346846716, 145.7918284779248665, 2.367408383378774239 ) ) ;
#26220 = AXIS2_PLACEMENT_3D ( 'NONE', #32750, #30378, #39568 ) ;
#26221 = CARTESIAN_POINT ( 'NONE',  ( 1.072590735131739414, 20.86836736082219801, 4.503669761903479341 ) ) ;
#26222 = CARTESIAN_POINT ( 'NONE',  ( -4.948315225313974608, -9.142465695005178361, 6.828157318318492486 ) ) ;
#26223 = CARTESIAN_POINT ( 'NONE',  ( -8.718980399793466063, 118.0112729258643469, -0.7777409526643788151 ) ) ;
#26224 = CARTESIAN_POINT ( 'NONE',  ( -3.231038154352895653, 124.0549386377059307, -0.1153833196696141400 ) ) ;
#26225 = DIRECTION ( 'NONE',  ( -5.188838149069471174E-16, 1.699382548006136313E-16, 1.000000000000000000 ) ) ;
#26226 = DIRECTION ( 'NONE',  ( 5.188838149069472160E-16, -1.699382548006136559E-16, -1.000000000000000000 ) ) ;
#26227 = CARTESIAN_POINT ( 'NONE',  ( -1.754637834204752389, 104.6144662015456674, 4.496842749848052101 ) ) ;
#26228 = CARTESIAN_POINT ( 'NONE',  ( 3.121479725567877228, 16.06095178295013071, 3.416230322513892137 ) ) ;
#26229 = CYLINDRICAL_SURFACE ( 'NONE', #10317, 0.5080000000000002292 ) ;
#26230 = CARTESIAN_POINT ( 'NONE',  ( 8.947566919452587848E-16, 9.293884745518887769, 0.000000000000000000 ) ) ;
#26231 = CARTESIAN_POINT ( 'NONE',  ( 2.904419875024614850, -13.46177902185440090, 0.8499660341922408158 ) ) ;
#26232 = CARTESIAN_POINT ( 'NONE',  ( 3.159661387648420305, 123.6198120039584154, -0.01957516827081329930 ) ) ;
#26233 = CARTESIAN_POINT ( 'NONE',  ( -22.94521658075157333, 142.4877946823990271, 0.4044642804735134600 ) ) ;
#26234 = ORIENTED_EDGE ( 'NONE', *, *, #19071, .F. ) ;
#26235 = FACE_OUTER_BOUND ( 'NONE', #31587, .T. ) ;
#26236 = VERTEX_POINT ( 'NONE', #21044 ) ;
#26237 = DIRECTION ( 'NONE',  ( 0.01731298258486638209, -0.9998501190848636533, 0.000000000000000000 ) ) ;
#26238 = CARTESIAN_POINT ( 'NONE',  ( 3.432040476525267891, -15.74971700692714904, 4.939269227581224442 ) ) ;
#26239 = CARTESIAN_POINT ( 'NONE',  ( -17.80465198604245458, 131.6735282812448986, 1.559227381006987434 ) ) ;
#26240 = CARTESIAN_POINT ( 'NONE',  ( 18.33177592110327225, 128.6097515361309149, -1.108544906447614720 ) ) ;
#26241 = CARTESIAN_POINT ( 'NONE',  ( 0.7007450612751181529, 9.901275517365906609, -4.597291952374415125 ) ) ;
#26242 = CARTESIAN_POINT ( 'NONE',  ( -58.61964679745516094, -0.2719338414218400723, -0.4055338230047252912 ) ) ;
#26243 = ORIENTED_EDGE ( 'NONE', *, *, #15372, .F. ) ;
#26244 = DIRECTION ( 'NONE',  ( 0.7308269722843605543, -0.6825627711659012498, 8.537024980200792236E-16 ) ) ;
#26245 = CARTESIAN_POINT ( 'NONE',  ( 2.157690779482308585, 123.3349985135950959, 0.1620144005770982609 ) ) ;
#26246 = B_SPLINE_SURFACE_WITH_KNOTS ( 'NONE', 5, 3, ( 
 ( #7456, #24451, #20835, #30019 ),
 ( #11461, #30228, #14239, #37055 ),
 ( #4478, #30646, #26830, #27245 ),
 ( #30854, #17853, #1067, #40261 ),
 ( #13832, #7873, #37455, #37254 ),
 ( #14035, #7665, #27456, #27039 ),
 ( #859, #40048, #1489, #40669 ),
 ( #40469, #11260, #20413, #33859 ) ),
 .UNSPECIFIED., .F., .F., .F.,
 ( 6, 2, 6 ),
 ( 4, 4 ),
 ( 0.000000000000000000, 0.5000000000000000000, 1.000000000000000000 ),
 ( -0.002373312499999995218, 0.03277393749999999578 ),
 .UNSPECIFIED. ) ;
#26247 = CARTESIAN_POINT ( 'NONE',  ( -8.008548551000092885, 121.6949282028273132, 0.7800530928440457812 ) ) ;
#26248 = CARTESIAN_POINT ( 'NONE',  ( -44.39753764704820327, 21.50835213917398647, 3.136200482385998800 ) ) ;
#26249 = CARTESIAN_POINT ( 'NONE',  ( 0.9814465556259852619, 157.4778559999684830, -1.561959177316861958 ) ) ;
#26250 = CARTESIAN_POINT ( 'NONE',  ( 0.01081828485855210013, 118.1092738308834669, -0.5413912121690738211 ) ) ;
#26251 = CARTESIAN_POINT ( 'NONE',  ( -57.67794393518098417, 1.927849678527493449, -1.763631237166056520 ) ) ;
#26252 = ORIENTED_EDGE ( 'NONE', *, *, #40223, .T. ) ;
#26253 = CARTESIAN_POINT ( 'NONE',  ( 4.547657880063963098, 118.1104688511466918, -0.5057482797829222498 ) ) ;
#26254 = CARTESIAN_POINT ( 'NONE',  ( 15.92216882203259232, 147.6644253265642135, -0.6463398217596317830 ) ) ;
#26255 = AXIS2_PLACEMENT_3D ( 'NONE', #25569, #21725, #2174 ) ;
#26256 = ORIENTED_EDGE ( 'NONE', *, *, #41215, .F. ) ;
#26257 = CARTESIAN_POINT ( 'NONE',  ( -16.55051581791506621, 149.4842840675632658, -2.199106316832546870 ) ) ;
#26258 = CARTESIAN_POINT ( 'NONE',  ( 3.375754317642519098, -15.02680299829225952, 2.760009546110721246 ) ) ;
#26259 = CYLINDRICAL_SURFACE ( 'NONE', #41547, 3.175000000000001155 ) ;
#26260 = CARTESIAN_POINT ( 'NONE',  ( -54.22787649382025421, 6.886497292746610377, -9.681224659302749425E-15 ) ) ;
#26261 = CARTESIAN_POINT ( 'NONE',  ( 3.679437910380295218, 2.726752568732802917, 2.794697870780981752 ) ) ;
#26262 = CARTESIAN_POINT ( 'NONE',  ( 15.22212811258876108, 150.6904849259475441, 2.083262412922771922 ) ) ;
#26263 = CARTESIAN_POINT ( 'NONE',  ( 2.026275176938348910, 36.00229031759788256, -0.4369541009056890912 ) ) ;
#26264 = CARTESIAN_POINT ( 'NONE',  ( -1.471791394198959102, 24.03230288535706549, 4.399545648925609065 ) ) ;
#26265 = CARTESIAN_POINT ( 'NONE',  ( 9.288927291931040386, 124.2653519604415067, 0.3477528771403741170 ) ) ;
#26266 = CARTESIAN_POINT ( 'NONE',  ( -1.176016126184881161, 105.9610483257683313, 5.207556883177536733 ) ) ;
#26268 = ORIENTED_EDGE ( 'NONE', *, *, #2518, .T. ) ;
#26267 = CARTESIAN_POINT ( 'NONE',  ( -47.30388380253317138, 17.78501317193704168, -2.251402236601650397 ) ) ;
#26269 = CARTESIAN_POINT ( 'NONE',  ( -5.561639213138736437, 116.7025976473698563, -0.1964723455066371971 ) ) ;
#26270 = DIRECTION ( 'NONE',  ( 0.9998004120163608288, 0.000000000000000000, 0.01997839162482760791 ) ) ;
#26271 = CARTESIAN_POINT ( 'NONE',  ( -46.68142054004553643, 26.02750436334470052, -1.325888764026806665 ) ) ;
#26272 = FACE_OUTER_BOUND ( 'NONE', #35275, .T. ) ;
#26273 = CARTESIAN_POINT ( 'NONE',  ( -30.15519950990045572, 69.97033940222173953, -1.524000000000010457 ) ) ;
#26274 = CARTESIAN_POINT ( 'NONE',  ( -5.965356522962928842, 53.58606250000000415, 5.016499999999999737 ) ) ;
#26275 = DIRECTION ( 'NONE',  ( 5.188838149069472160E-16, -1.699382548006136559E-16, -1.000000000000000000 ) ) ;
#26276 = CARTESIAN_POINT ( 'NONE',  ( -16.71197878298170991, 83.87086364642222236, 1.523999999999996691 ) ) ;
#26277 = CARTESIAN_POINT ( 'NONE',  ( -56.91937565786325592, 5.591339438888994984, 0.1632292574589306045 ) ) ;
#26278 = AXIS2_PLACEMENT_3D ( 'NONE', #7085, #20677, #24089 ) ;
#26279 = CARTESIAN_POINT ( 'NONE',  ( -58.33777482027510786, 1.113448835244251756, 1.208045587469420701 ) ) ;
#26280 = CARTESIAN_POINT ( 'NONE',  ( -16.00576599164912750, 121.2237126890796191, -0.08595866332889588735 ) ) ;
#26281 = TOROIDAL_SURFACE ( 'NONE', #18798, 5.080000000000005400, 0.5080000000000000071 ) ;
#26282 = VERTEX_POINT ( 'NONE', #33651 ) ;
#26283 = CARTESIAN_POINT ( 'NONE',  ( -52.32205026661357294, 13.67230311332622072, -4.407798173677540454 ) ) ;
#26284 = CARTESIAN_POINT ( 'NONE',  ( 7.804305114750069272, 122.5549487891343574, -0.07597547369942431184 ) ) ;
#26285 = ORIENTED_EDGE ( 'NONE', *, *, #7752, .F. ) ;
#26286 = CARTESIAN_POINT ( 'NONE',  ( -8.336765840796966032, 73.19241104973453105, -1.269999999999996687 ) ) ;
#26287 = CARTESIAN_POINT ( 'NONE',  ( -1.617373050801775625, 120.9968702744464366, -0.03231896268895485813 ) ) ;
#26288 = CARTESIAN_POINT ( 'NONE',  ( 4.135482704272881449, -14.73569165307708673, 5.015242562682193039 ) ) ;
#26289 = CARTESIAN_POINT ( 'NONE',  ( -1.228124343681062047, 158.9035955689636523, 1.375095950729814165 ) ) ;
#26290 = CARTESIAN_POINT ( 'NONE',  ( -3.130497002865707756, 23.39511390029671745, 3.426874451367011520 ) ) ;
#26291 = CARTESIAN_POINT ( 'NONE',  ( 15.91552649980314627, 121.2232988859741027, 0.6415868299260654162 ) ) ;
#26292 = CARTESIAN_POINT ( 'NONE',  ( 2.163718758107066709, -15.46264904772556825, 5.921791837560038907 ) ) ;
#26293 = CARTESIAN_POINT ( 'NONE',  ( 5.276310133815047543, 115.6909491485453145, -0.8120701714742106780 ) ) ;
#26294 = CARTESIAN_POINT ( 'NONE',  ( 0.4358653558703468045, -2.730035452555519271, 0.8728101606764442355 ) ) ;
#26295 = CARTESIAN_POINT ( 'NONE',  ( -18.61947985292905017, 154.1412379532633850, -0.5163013828871974020 ) ) ;
#26296 = CARTESIAN_POINT ( 'NONE',  ( -4.743925087698587006, 117.9014421663514725, 0.7646676084295724873 ) ) ;
#26297 = CARTESIAN_POINT ( 'NONE',  ( -11.34554992887676228, 77.73165686004496422, -1.523999999999998911 ) ) ;
#26298 = VERTEX_POINT ( 'NONE', #7663 ) ;
#26299 = CARTESIAN_POINT ( 'NONE',  ( 8.781532007625042269, 117.7401941391528624, 0.4292495202309390967 ) ) ;
#26300 = ORIENTED_EDGE ( 'NONE', *, *, #7190, .F. ) ;
#26301 = CARTESIAN_POINT ( 'NONE',  ( -14.02613073054681614, 152.5802402909829425, 1.631301951249305215 ) ) ;
#26302 = CARTESIAN_POINT ( 'NONE',  ( -58.36917081973859922, -0.2902516154645916058, -0.03021462763837517995 ) ) ;
#26303 = CARTESIAN_POINT ( 'NONE',  ( 6.782271978584973660, 118.5360090424673274, 1.159066879843025255 ) ) ;
#26304 = CARTESIAN_POINT ( 'NONE',  ( 0.03212618750947002916, 158.2819368290249713, -1.607725792532325171 ) ) ;
#26305 = CARTESIAN_POINT ( 'NONE',  ( 0.1234711523483410095, 5.102374915558315571, -0.9659065422363407594 ) ) ;
#26306 = CARTESIAN_POINT ( 'NONE',  ( -21.62407820142113835, 149.9601031839316079, -2.013249247985050339 ) ) ;
#26307 = CARTESIAN_POINT ( 'NONE',  ( 4.595251882992044123, 118.0172796872295891, -0.6951473410461010971 ) ) ;
#26308 = EDGE_CURVE ( 'NONE', #20372, #36001, #32224, .T. ) ;
#26309 = DIRECTION ( 'NONE',  ( 5.188838149069472160E-16, -1.699382548006136559E-16, -1.000000000000000000 ) ) ;
#26310 = EDGE_CURVE ( 'NONE', #27898, #35651, #22010, .T. ) ;
#26311 = CARTESIAN_POINT ( 'NONE',  ( 10.37991283549660437, 123.8962982355681817, -0.8252603836154487338 ) ) ;
#26312 = CARTESIAN_POINT ( 'NONE',  ( -14.17939111974024335, 138.8817910697950140, -0.2325274008182653396 ) ) ;
#26313 = EDGE_LOOP ( 'NONE', ( #14998, #36061 ) ) ;
#26314 = CARTESIAN_POINT ( 'NONE',  ( 0.03212616895145502249, 157.6269964811067155, -1.607724863813388971 ) ) ;
#26315 = CARTESIAN_POINT ( 'NONE',  ( 3.900291174488768053, -15.73247852219369847, 4.461464635514134969 ) ) ;
#26316 = CIRCLE ( 'NONE', #24947, 2.857500000000000817 ) ;
#26317 = DIRECTION ( 'NONE',  ( -5.206863593109713661E-17, 1.000000000000000000, -1.077750396879097183E-30 ) ) ;
#26318 = CARTESIAN_POINT ( 'NONE',  ( -46.07906060731711761, 24.80782705053048076, -1.769089518196001798 ) ) ;
#26320 = ORIENTED_EDGE ( 'NONE', *, *, #37367, .T. ) ;
#26319 = VECTOR ( 'NONE', #22173, 1000.000000000000000 ) ;
#26321 = CARTESIAN_POINT ( 'NONE',  ( 13.34752792037768820, 125.8771108566470502, 1.915935069336977659 ) ) ;
#26322 = CARTESIAN_POINT ( 'NONE',  ( -5.309060684617390516E-14, 83.56599999999998829, 0.000000000000000000 ) ) ;
#26323 = CARTESIAN_POINT ( 'NONE',  ( 4.910479103859797689, 115.7029491485453008, 1.454559715794871089 ) ) ;
#26324 = CARTESIAN_POINT ( 'NONE',  ( -0.2179432916433551026, 106.0530876078258586, 5.262233728842789837 ) ) ;
#26325 = CARTESIAN_POINT ( 'NONE',  ( -8.190863557275731566, 21.65400946394957060, -2.068261358883292989 ) ) ;
#26326 = CARTESIAN_POINT ( 'NONE',  ( 9.364230102553010582, 123.8909350679826815, 0.6996930829695083842 ) ) ;
#26327 = CARTESIAN_POINT ( 'NONE',  ( 0.3541790919670912419, 116.9919054422455531, -0.3273860145854423642 ) ) ;
#26328 = DIRECTION ( 'NONE',  ( 0.1538365266688606903, -0.9876883405951383255, 0.02839128237474894401 ) ) ;
#26329 = LINE ( 'NONE', #13342, #6586 ) ;
#26330 = VECTOR ( 'NONE', #12261, 1000.000000000000227 ) ;
#26331 = EDGE_CURVE ( 'NONE', #5685, #17866, #1653, .T. ) ;
#26332 = CARTESIAN_POINT ( 'NONE',  ( -8.217303172778619214, 117.5015518944296247, -0.1195796404652190448 ) ) ;
#26333 = ORIENTED_EDGE ( 'NONE', *, *, #9706, .F. ) ;
#26334 = CARTESIAN_POINT ( 'NONE',  ( 6.675603198613333511, 120.7516070878810410, -0.8047696622842539504 ) ) ;
#26335 = CARTESIAN_POINT ( 'NONE',  ( 6.242199107252148771, -13.90286925626189252, 1.333809230853582273 ) ) ;
#26336 = AXIS2_PLACEMENT_3D ( 'NONE', #18257, #31261, #15696 ) ;
#26337 = CARTESIAN_POINT ( 'NONE',  ( -15.38106487260184529, 148.0444422243178337, -0.8962548396073235502 ) ) ;
#26338 = CARTESIAN_POINT ( 'NONE',  ( 3.948573903914379457, -12.48127506095717010, 1.805458641749257520 ) ) ;
#26339 = CARTESIAN_POINT ( 'NONE',  ( -16.02745508617906012, 155.1095016151506911, 1.019363059911538860 ) ) ;
#26340 = CARTESIAN_POINT ( 'NONE',  ( -17.14500000000466784, 71.11999999999886768, 1.269999999999998241 ) ) ;
#26341 = CARTESIAN_POINT ( 'NONE',  ( 0.2950350728689354329, 116.4333835968663919, 0.04389667002116236227 ) ) ;
#26342 = EDGE_LOOP ( 'NONE', ( #41942, #36284, #10790, #37351, #23627 ) ) ;
#26343 = CARTESIAN_POINT ( 'NONE',  ( 4.636249899789679496, -11.37698174978397958, -0.2454043791197063895 ) ) ;
#26344 = CARTESIAN_POINT ( 'NONE',  ( -23.42514220146296111, 142.8382549601284097, -0.4680900899253088721 ) ) ;
#26345 = CARTESIAN_POINT ( 'NONE',  ( 18.35410564743290607, 77.35382415001784295, 5.016499999999999737 ) ) ;
#26346 = CARTESIAN_POINT ( 'NONE',  ( 1.217703060157562689, 106.0679358989203536, 5.195502566823263280 ) ) ;
#26347 = AXIS2_PLACEMENT_3D ( 'NONE', #27085, #10679, #26875 ) ;
#26348 = CARTESIAN_POINT ( 'NONE',  ( 6.997741591014696283, 121.4429130386087934, 0.8574795444661736932 ) ) ;
#26349 = CARTESIAN_POINT ( 'NONE',  ( -2.972019672840211513, 9.848453565018933986, 3.538668892428941781 ) ) ;
#26350 = CARTESIAN_POINT ( 'NONE',  ( 19.95201466422899728, 152.4248492066682559, 1.669502467017324854 ) ) ;
#26351 = DIRECTION ( 'NONE',  ( -0.3582377630123916856, 0.9336303900108853249, -3.445432962228668055E-16 ) ) ;
#26353 = CARTESIAN_POINT ( 'NONE',  ( 12.06131655867242713, 120.6765805525287334, -1.069212010736125817 ) ) ;
#26352 = CARTESIAN_POINT ( 'NONE',  ( -8.690931667554782081, 74.34623700195145091, 1.270000000000002238 ) ) ;
#26354 = CARTESIAN_POINT ( 'NONE',  ( 3.235533175430977515, 2.501875212487111977, 3.308963532380430284 ) ) ;
#26355 = CARTESIAN_POINT ( 'NONE',  ( -15.26873630740966270, 121.3917326167944708, -1.149126527656483043 ) ) ;
#26356 = EDGE_CURVE ( 'NONE', #9715, #9538, #13175, .T. ) ;
#26357 = ORIENTED_EDGE ( 'NONE', *, *, #20613, .F. ) ;
#26358 = CARTESIAN_POINT ( 'NONE',  ( 7.461249999999945537, 86.35999999999998522, 0.000000000000000000 ) ) ;
#26359 = CARTESIAN_POINT ( 'NONE',  ( -15.60869185768510903, 147.5518517437054982, 0.1389895172399198409 ) ) ;
#26360 = CARTESIAN_POINT ( 'NONE',  ( 5.456921283009238621, -14.23391906346564717, 3.426434758229824240 ) ) ;
#26361 = MECHANICAL_DESIGN_GEOMETRIC_PRESENTATION_REPRESENTATION (  '', ( #21570 ), #39329 ) ;
#26362 = CARTESIAN_POINT ( 'NONE',  ( -3.278664548829097747, 108.1634672882638029, -4.198944545392978789 ) ) ;
#26363 = EDGE_CURVE ( 'NONE', #34378, #20421, #3686, .T. ) ;
#26364 = ORIENTED_EDGE ( 'NONE', *, *, #41193, .T. ) ;
#26365 = CARTESIAN_POINT ( 'NONE',  ( 13.83536887852627650, 154.2684476645699760, 2.291766773079779718 ) ) ;
#26366 = PLANE ( 'NONE',  #41283 ) ;
#26367 = CARTESIAN_POINT ( 'NONE',  ( -6.057513928997641628, 57.78499999999998948, -1.904999999999999805 ) ) ;
#26368 = CARTESIAN_POINT ( 'NONE',  ( -22.55548643167962197, 142.2972183020237367, 0.7396483830486686450 ) ) ;
#26369 = CARTESIAN_POINT ( 'NONE',  ( 2.538140519494355374, 21.06397054095828381, 8.048466014368985455 ) ) ;
#26370 = PRODUCT_DEFINITION ( 'UNKNOWN', '', #34608, #25701 ) ;
#26371 = CARTESIAN_POINT ( 'NONE',  ( 1.406537315630064677, 159.5914066142653098, -0.2310332007158441836 ) ) ;
#26372 = CARTESIAN_POINT ( 'NONE',  ( -5.224085778414857550, 56.51500000000001478, -4.542437760755098530 ) ) ;
#26373 = CARTESIAN_POINT ( 'NONE',  ( -48.81378120017792099, 18.07100238705057649, 5.105379834343001910 ) ) ;
#26374 = CARTESIAN_POINT ( 'NONE',  ( -47.91489772873670461, 20.73163290703075745, 4.601312741204995227 ) ) ;
#26375 = CARTESIAN_POINT ( 'NONE',  ( 1.859021851459260022, -15.10376415035639930, 5.547171369656321183 ) ) ;
#26376 = CARTESIAN_POINT ( 'NONE',  ( -50.82551848962686591, 16.13924203555649228, 4.804203053272154911 ) ) ;
#26377 = CARTESIAN_POINT ( 'NONE',  ( -58.71329930298021083, -0.3143398509990111278, 0.2746998690518271946 ) ) ;
#26378 = ADVANCED_FACE ( 'NONE', ( #7871 ), #25414, .T. ) ;
#26379 = B_SPLINE_CURVE_WITH_KNOTS ( 'NONE', 3,
 ( #7348, #20941, #27349, #10322, #17337, #14339, #24142, #17126, #36735, #29707, #33548, #30127, #1381, #4379, #7972, #23291, #16917, #13935, #33966, #13523 ),
 .UNSPECIFIED., .F., .F.,
 ( 4, 2, 2, 2, 2, 2, 2, 2, 2, 4 ),
 ( -5.999999999384015929E-08, 0.002615939326670506469, 0.005231938653341007377, 0.007847937980011505249, 0.01046393730668200746, 0.01307993663335250793, 0.01438793629668775817, 0.01569593596002300667, 0.01831193528669351062, 0.02092793461336401456 ),
 .UNSPECIFIED. ) ;
#26380 = CARTESIAN_POINT ( 'NONE',  ( -4.603251683469835598, 118.0757897185588234, 0.5233029099187971322 ) ) ;
#26381 = CARTESIAN_POINT ( 'NONE',  ( -23.43300365160793319, 82.12916405548841681, 1.523999999999993360 ) ) ;
#26382 = VERTEX_POINT ( 'NONE', #7454 ) ;
#26383 = CARTESIAN_POINT ( 'NONE',  ( -47.19936399096372526, 20.24790404726484283, 5.251082349106850344 ) ) ;
#26384 = EDGE_CURVE ( 'NONE', #32222, #1192, #11053, .T. ) ;
#26385 = CARTESIAN_POINT ( 'NONE',  ( -3.841645322271367569, 119.0006533405734928, -0.9283627247572711072 ) ) ;
#26386 = CARTESIAN_POINT ( 'NONE',  ( -6.689329653978204782, 121.2318545172250737, -0.3418430003135978779 ) ) ;
#26387 = CARTESIAN_POINT ( 'NONE',  ( 4.437541795254049681, 118.1257943510456840, 0.7326559301581485606 ) ) ;
#26388 = CARTESIAN_POINT ( 'NONE',  ( -7.769844292200057012, 122.1031240515655298, -0.8163738826679363125 ) ) ;
#26389 = STYLED_ITEM ( 'NONE', ( #21727 ), #15308 ) ;
#26390 = CARTESIAN_POINT ( 'NONE',  ( -1.801924311864099293, 115.7029148620384404, -1.722817892843705234 ) ) ;
#26391 = ADVANCED_FACE ( 'NONE', ( #30433 ), #32724, .T. ) ;
#26392 = CARTESIAN_POINT ( 'NONE',  ( 1.138070077757084686, 117.9496053113818448, -1.345098318217916811 ) ) ;
#26393 = CARTESIAN_POINT ( 'NONE',  ( 5.774381877465427415, 118.4424948052634647, -0.4329097047088598660 ) ) ;
#26394 = CARTESIAN_POINT ( 'NONE',  ( -16.78017617680123763, 148.3581316477378493, -2.036619618061130677 ) ) ;
#26395 = CARTESIAN_POINT ( 'NONE',  ( 5.304438957985845526, 116.0444662015456885, -1.082911341041116637 ) ) ;
#26396 = CARTESIAN_POINT ( 'NONE',  ( -0.01443894962468954962, 159.4760848062415732, 0.7225840825867287931 ) ) ;
#26397 = CARTESIAN_POINT ( 'NONE',  ( 8.675687895398256799, 118.3610464811750802, -0.6699752535086603844 ) ) ;
#26398 = CARTESIAN_POINT ( 'NONE',  ( -15.38177525964082371, 147.8337523264461879, -0.2407145083428142707 ) ) ;
#26399 = CARTESIAN_POINT ( 'NONE',  ( -1.861891798414337940, 1.167894131763866250, -4.247245584637167504 ) ) ;
#26400 = CARTESIAN_POINT ( 'NONE',  ( 22.68171885890631145, 150.0520759213295889, 1.302983692151378436 ) ) ;
#26401 = CARTESIAN_POINT ( 'NONE',  ( -3.671158984043940170E-14, 57.78499999999999659, 0.000000000000000000 ) ) ;
#26402 = CARTESIAN_POINT ( 'NONE',  ( 2.102798109511007318, -15.25784609616889753, 5.176374340497880588 ) ) ;
#26403 = CARTESIAN_POINT ( 'NONE',  ( -11.96109417309370748, 154.9039014673913073, 1.746238851223627986 ) ) ;
#26404 = CARTESIAN_POINT ( 'NONE',  ( -0.4136891606132181431, 9.424461778640809584, 0.8817368238460310259 ) ) ;
#26405 = CARTESIAN_POINT ( 'NONE',  ( -20.06391502460639842, 128.8637844977697569, -0.9116527748870052461 ) ) ;
#26406 = AXIS2_PLACEMENT_3D ( 'NONE', #35756, #38739, #6571 ) ;
#26407 = CARTESIAN_POINT ( 'NONE',  ( -0.8351715869602673870, 27.76506109569598024, 0.5290732382595327854 ) ) ;
#26408 = EDGE_LOOP ( 'NONE', ( #23662, #16935, #12461, #4797 ) ) ;
#26409 = ORIENTED_EDGE ( 'NONE', *, *, #40491, .T. ) ;
#26410 = CARTESIAN_POINT ( 'NONE',  ( -46.67338572489352089, 16.85372243840493311, 0.3683569569372045494 ) ) ;
#26411 = CARTESIAN_POINT ( 'NONE',  ( 7.065765265293006969, 122.4340714744230496, 0.2508917249367682567 ) ) ;
#26412 = DIRECTION ( 'NONE',  ( 1.000000000000000000, 0.000000000000000000, 0.000000000000000000 ) ) ;
#26413 = CARTESIAN_POINT ( 'NONE',  ( -0.01341678693510457362, 156.4123495908283985, 0.6714308817992611367 ) ) ;
#26414 = CARTESIAN_POINT ( 'NONE',  ( 2.161572811135036964, -15.02537755669194830, 5.771884496758437066 ) ) ;
#26415 = CARTESIAN_POINT ( 'NONE',  ( 16.62515567699070473, 149.4842840675632658, -1.536177446654198198 ) ) ;
#26416 = CARTESIAN_POINT ( 'NONE',  ( -19.42145995676313674, 149.0830822498907082, -2.502058577541587336 ) ) ;
#26417 = DIRECTION ( 'NONE',  ( -0.4849315768086535638, -0.8745520943968251304, -1.030032898892975065E-16 ) ) ;
#26418 = CARTESIAN_POINT ( 'NONE',  ( 2.766857707386623400, -13.29092698609396450, 0.4080254275553683585 ) ) ;
#26419 = CARTESIAN_POINT ( 'NONE',  ( -0.5146975708209950984, 37.55987809028739832, 0.05064662351078883656 ) ) ;
#26420 = CARTESIAN_POINT ( 'NONE',  ( 1.606403942294383214, 120.9755568995931156, -0.03214495494220263178 ) ) ;
#26421 = ORIENTED_EDGE ( 'NONE', *, *, #33993, .F. ) ;
#26422 = CARTESIAN_POINT ( 'NONE',  ( -5.278861607444886417, 115.7725975576095720, 0.7828656677038698941 ) ) ;
#26423 = CARTESIAN_POINT ( 'NONE',  ( 15.21260244842765452, 9.026346327358513832, 0.000000000000000000 ) ) ;
#26424 = SHAPE_REPRESENTATION ( 'Pivot Pins', ( #3275 ), #32513 ) ;
#26425 = CARTESIAN_POINT ( 'NONE',  ( -10.92199999999999704, 16.51000000000000156, 0.000000000000000000 ) ) ;
#26426 = DIRECTION ( 'NONE',  ( -0.8745520943968466687, 0.4849315768086143730, -6.829619984160688614E-16 ) ) ;
#26427 = ADVANCED_FACE ( 'NONE', ( #20204 ), #14993, .F. ) ;
#26428 = CARTESIAN_POINT ( 'NONE',  ( 3.292377373361659920, 159.4686222989141697, -0.02724393823342678017 ) ) ;
#26429 = AXIS2_PLACEMENT_3D ( 'NONE', #19662, #39071, #39280 ) ;
#26430 = CARTESIAN_POINT ( 'NONE',  ( -3.580579253266132689, 108.6681208952157078, 3.986884027299105071 ) ) ;
#26431 = CIRCLE ( 'NONE', #17606, 0.5080000000000030047 ) ;
#26432 = DIRECTION ( 'NONE',  ( 0.9998004120163609398, 0.000000000000000000, 0.01997839162482749689 ) ) ;
#26433 = LINE ( 'NONE', #23425, #39906 ) ;
#26434 = CARTESIAN_POINT ( 'NONE',  ( -3.328555392133318858, 33.88165127674241717, 1.160568618710268618 ) ) ;
#26435 = CARTESIAN_POINT ( 'NONE',  ( 13.08065502438826400, 121.7804325175133755, 1.718327614618424315 ) ) ;
#26436 = CARTESIAN_POINT ( 'NONE',  ( 4.353980591602404360, 23.44215234368072487, -1.583070106892425111 ) ) ;
#26437 = CARTESIAN_POINT ( 'NONE',  ( -6.911983299595774177, -11.51556667111630894, -4.837919318831837678 ) ) ;
#26438 = CARTESIAN_POINT ( 'NONE',  ( -5.493189927730356636, 117.6942598834481686, -1.012164059239212710 ) ) ;
#26439 = CARTESIAN_POINT ( 'NONE',  ( -1.569662112149406763, 118.6366899268033279, -0.8670489899392761490 ) ) ;
#26440 = DIRECTION ( 'NONE',  ( -0.8745520943968250194, 0.4849315768086535083, -5.424246918827963022E-16 ) ) ;
#26441 = CARTESIAN_POINT ( 'NONE',  ( -10.28897677580358128, 56.51499999999998636, -4.381499999999999950 ) ) ;
#26442 = CARTESIAN_POINT ( 'NONE',  ( 2.143370549553493820, 105.1244188156866954, 4.894740234150261493 ) ) ;
#26443 = CARTESIAN_POINT ( 'NONE',  ( -2.755274729907521980, 20.69627551736597226, -3.746277899328600558 ) ) ;
#26444 = EDGE_CURVE ( 'NONE', #24193, #32067, #4444, .T. ) ;
#26445 = DIRECTION ( 'NONE',  ( 5.188838149069472160E-16, -1.699382548006136559E-16, -1.000000000000000000 ) ) ;
#26446 = CARTESIAN_POINT ( 'NONE',  ( -18.35410564743290607, 77.35382415001784295, -5.016499999999999737 ) ) ;
#26447 = CARTESIAN_POINT ( 'NONE',  ( 2.237742905438162122, -15.06201634873256801, 5.120316289255383069 ) ) ;
#26448 = CARTESIAN_POINT ( 'NONE',  ( 1.980194564007054403, 113.2583846565721757, -2.436415359710689010 ) ) ;
#26449 = CARTESIAN_POINT ( 'NONE',  ( -22.47867321467015955, 150.2745577238280816, 0.5153050491938901967 ) ) ;
#26450 = EDGE_CURVE ( 'NONE', #34427, #35121, #14237, .T. ) ;
#26451 = FACE_OUTER_BOUND ( 'NONE', #35727, .T. ) ;
#26452 = VERTEX_POINT ( 'NONE', #8070 ) ;
#26453 = CARTESIAN_POINT ( 'NONE',  ( -5.460438898883190006, 56.51499999999997215, 4.448267477574868067 ) ) ;
#26454 = VERTEX_POINT ( 'NONE', #37252 ) ;
#26455 = CARTESIAN_POINT ( 'NONE',  ( -6.065440317703094664, 31.08949202354850172, -0.5906148415105061389 ) ) ;
#26456 = CARTESIAN_POINT ( 'NONE',  ( 5.620948709224020234, -15.12563517700941951, 1.754161952847088868 ) ) ;
#26457 = CARTESIAN_POINT ( 'NONE',  ( -19.51325853822230272, 141.0981142166620259, 1.725252114789138647 ) ) ;
#26458 = CARTESIAN_POINT ( 'NONE',  ( 14.13727225732671222, 121.3807765770047666, -0.9276936697596736003 ) ) ;
#26459 = CARTESIAN_POINT ( 'NONE',  ( 0.8332047475417917459, 28.58290516567101491, -0.5069163209656499802 ) ) ;
#26460 = CARTESIAN_POINT ( 'NONE',  ( -58.78715887833730847, -0.2958247752677126141, -0.1682579856030674004 ) ) ;
#26461 = ORIENTED_EDGE ( 'NONE', *, *, #31687, .T. ) ;
#26462 = CARTESIAN_POINT ( 'NONE',  ( -4.918661145027864556, 117.4102335145295370, -1.102851133234106662 ) ) ;
#26463 = CARTESIAN_POINT ( 'NONE',  ( 0.9302644990744406428, 122.9246775559910390, 0.2070653534288171282 ) ) ;
#26464 = CARTESIAN_POINT ( 'NONE',  ( -1.452025732293910965, 120.0849730816093910, 0.4508766852696775573 ) ) ;
#26465 = LINE ( 'NONE', #23889, #9599 ) ;
#26466 = CIRCLE ( 'NONE', #12204, 0.5080000000000002292 ) ;
#26467 = CARTESIAN_POINT ( 'NONE',  ( 3.371641211477126809, 119.4525916976722897, -0.7211689390744320249 ) ) ;
#26468 = CLOSED_SHELL ( 'NONE', ( #31779, #31356, #33394, #18032, #9713, #26896, #8217, #41483, #35482, #41130, #9677, #1171, #35220, #7225, #40741, #203, #20395, #39138, #13159, #9295, #17291, #30443, #36318, #36557, #39305, #27934, #14109, #5649, #29091, #17502, #12537, #28721, #40774, #22283, #27883, #29577, #24791, #11840, #40165, #24016, #25653, #31400, #23843, #638, #41265, #39151, #17733, #164, #18451, #13367, #13029, #21097, #24609, #21175, #20126, #4757, #11479, #13669, #9558, #1165, #7417, #3413, #41854, #29217, #36751, #24292, #13855, #24646, #8760, #5585, #4780, #3524, #31284, #32963, #6343, #21619, #37651, #33468, #5305, #19106, #18806, #6130, #38583, #5346, #12117, #33142, #9912, #29741, #34515, #11817, #17212, #21958, #24653, #15933, #28088, #3579, #31087, #11268, #40459, #9956, #21154, #28981, #25064, #28253, #17453, #19079, #26427, #21955, #39844, #35027, #36026, #6785, #11527, #17966, #10221, #9503, #32551, #5128, #6983, #11486, #28517, #5609, #23002, #30769, #12171, #41817, #13338, #15984, #15710, #9458, #5876, #34713, #403, #30815, #24515, #12629, #19637, #30039, #24083, #35288, #8163, #21705, #17197, #4537, #16573, #20178, #16173, #2699, #23752, #17259, #3444, #4814, #20321, #39627, #2984, #38653, #12859, #12831, #20070, #15804, #4724 ) ) ;
#26469 = CARTESIAN_POINT ( 'NONE',  ( -3.096092393557038580, 118.0390668470448929, -0.8277768005040341270 ) ) ;
#26470 = CARTESIAN_POINT ( 'NONE',  ( -58.37241122568488549, -0.2962816677227753104, -0.2416009568454014489 ) ) ;
#26471 = ORIENTED_EDGE ( 'NONE', *, *, #19395, .T. ) ;
#26472 = CARTESIAN_POINT ( 'NONE',  ( 4.507247720737455943, 118.1170994507041030, -0.5526904508501585545 ) ) ;
#26473 = CARTESIAN_POINT ( 'NONE',  ( 9.439557112687584350, 123.9587481073520223, -0.3264598115655270028 ) ) ;
#26474 = ORIENTED_EDGE ( 'NONE', *, *, #38908, .T. ) ;
#26475 = CARTESIAN_POINT ( 'NONE',  ( -7.267393677827440612, 155.8804291298944236, -1.807016794997827525 ) ) ;
#26476 = CARTESIAN_POINT ( 'NONE',  ( 2.678036876842718517, -15.12020262989130437, 4.533791366373512766 ) ) ;
#26477 = CARTESIAN_POINT ( 'NONE',  ( 1.165615098987396347, 105.1232203586557290, -5.215136134052268169 ) ) ;
#26478 = CARTESIAN_POINT ( 'NONE',  ( -56.37342374758031127, 3.980281407817698458, 2.237022232197619864 ) ) ;
#26479 = CARTESIAN_POINT ( 'NONE',  ( -3.586339569854333664, 7.474549112184490696, -2.913498476264247294 ) ) ;
#26480 = CARTESIAN_POINT ( 'NONE',  ( 5.103418814394237835, 120.3680889145531552, 0.8767301089910152223 ) ) ;
#26481 = CARTESIAN_POINT ( 'NONE',  ( 2.979675570102178650, 39.20946620154573026, 0.2712499303477601820 ) ) ;
#26482 = CARTESIAN_POINT ( 'NONE',  ( 4.513502956352341222, 8.064680226961385756, -0.9949261897555528034 ) ) ;
#26483 = CARTESIAN_POINT ( 'NONE',  ( -0.001255909994615970462, 120.9722815239556439, 0.06285087176068887560 ) ) ;
#26484 = CARTESIAN_POINT ( 'NONE',  ( -5.369399562154598904, 64.90898011766716991, -1.269999999999993578 ) ) ;
#26485 = EDGE_CURVE ( 'NONE', #19701, #10361, #36950, .T. ) ;
#26486 = AXIS2_PLACEMENT_3D ( 'NONE', #26182, #33228, #35577 ) ;
#26487 = CARTESIAN_POINT ( 'NONE',  ( -51.51920269172890698, 12.50394502492935978, -2.730133853924327170 ) ) ;
#26488 = CARTESIAN_POINT ( 'NONE',  ( -2.183972911347295209, 116.1856571598952144, -0.06668066542220674187 ) ) ;
#26489 = CARTESIAN_POINT ( 'NONE',  ( 18.63504953328963154, 154.1157618415863624, 0.3723726386282266709 ) ) ;
#26490 = DIRECTION ( 'NONE',  ( 5.188838149069472160E-16, -1.699382548006136559E-16, -1.000000000000000000 ) ) ;
#26491 = CARTESIAN_POINT ( 'NONE',  ( -10.55305098051677248, 77.31887769575739355, -1.269999999999998241 ) ) ;
#26492 = DIRECTION ( 'NONE',  ( -5.188838149069471174E-16, 1.699382548006136313E-16, 1.000000000000000000 ) ) ;
#26493 = CARTESIAN_POINT ( 'NONE',  ( -5.305748947172281405, 53.58606250000000415, 5.247078976224250013 ) ) ;
#26494 = EDGE_CURVE ( 'NONE', #17488, #17144, #36802, .T. ) ;
#26495 = CARTESIAN_POINT ( 'NONE',  ( -29.82321757229076908, 71.17901112636586447, 1.269999999999991802 ) ) ;
#26496 = DIRECTION ( 'NONE',  ( 0.7548010569845216011, 0.6559537821943317581, 2.801824109679580762E-16 ) ) ;
#26497 = CARTESIAN_POINT ( 'NONE',  ( -58.60381103753274346, 0.5214191424347813797, 0.2072982876684393294 ) ) ;
#26498 = CARTESIAN_POINT ( 'NONE',  ( -57.00508801794419611, 2.691366720778187727, 1.977812201481533583 ) ) ;
#26499 = CARTESIAN_POINT ( 'NONE',  ( -3.792432603185484474, 116.7736770086926867, 0.1904249565637312347 ) ) ;
#26500 = ORIENTED_EDGE ( 'NONE', *, *, #72, .F. ) ;
#26501 = CARTESIAN_POINT ( 'NONE',  ( -54.22526503003591358, 12.24891082007571086, -1.741649939400669478 ) ) ;
#26502 = CARTESIAN_POINT ( 'NONE',  ( -6.044933042564573533, 121.4357306406764252, -0.1374383516041701447 ) ) ;
#26503 = VERTEX_POINT ( 'NONE', #40667 ) ;
#26504 = CARTESIAN_POINT ( 'NONE',  ( 4.825036788390894671, 62.83146620154573014, 0.09641571798141751470 ) ) ;
#26505 = CARTESIAN_POINT ( 'NONE',  ( -9.106973723525666031, 153.9337724597031070, -0.2264262902970467783 ) ) ;
#26506 = CARTESIAN_POINT ( 'NONE',  ( 5.414172367154487908, -13.81390647261572546, 3.268633212004894872 ) ) ;
#26507 = CARTESIAN_POINT ( 'NONE',  ( -21.26977539036090548, 145.8710773725474610, 1.472442194194814702 ) ) ;
#26508 = CARTESIAN_POINT ( 'NONE',  ( 4.619096255015035624, 27.05588869245799089, -0.3994036469054788596 ) ) ;
#26509 = CARTESIAN_POINT ( 'NONE',  ( 16.76609992697660800, 155.2615993841311877, 0.7433399007605487885 ) ) ;
#26510 = CARTESIAN_POINT ( 'NONE',  ( 2.125773701607508226, -15.49174028809012427, 5.936015161737096868 ) ) ;
#26511 = CARTESIAN_POINT ( 'NONE',  ( -4.349660437102230048, 31.17966527223318707, -1.615541842050199461 ) ) ;
#26512 = CARTESIAN_POINT ( 'NONE',  ( 0.8097498057273965211, -0.1318080948593848278, -0.5455758836208917106 ) ) ;
#26513 = CARTESIAN_POINT ( 'NONE',  ( -23.27880353394132484, 149.3453998935430604, -0.6192278183506784162 ) ) ;
#26514 = CARTESIAN_POINT ( 'NONE',  ( -10.86251533436417915, 78.45482716897161879, -1.904999999999999583 ) ) ;
#26515 = CARTESIAN_POINT ( 'NONE',  ( 4.936888680085094627, 117.4097579285739954, 1.082126315060445876 ) ) ;
#26516 = CARTESIAN_POINT ( 'NONE',  ( 5.537423627294297823, 116.8704610243493107, 0.5072075918636228531 ) ) ;
#26517 = VERTEX_POINT ( 'NONE', #8277 ) ;
#26518 = CARTESIAN_POINT ( 'NONE',  ( -17.52489820599672399, 148.6234142586927476, 1.577473031907404843 ) ) ;
#26519 = B_SPLINE_CURVE_WITH_KNOTS ( 'NONE', 3,
 ( #24054, #13846, #26844, #7887, #23842, #4285, #30242, #1082, #36864, #20849, #33874, #7680, #20639, #33669, #20017, #5749, #38109, #40683, #40482, #18489, #37469, #25106, #28305, #11475, #34085, #21466, #41311, #8925, #12116, #27673, #40889, #8508, #21059, #2125, #18701, #2342, #15087, #31495, #34294, #15299, #37267, #21263, #24464, #8294, #18280, #5122, #18075, #37893, #21890, #11692, #31077, #28089, #34919, #1916, #14878, #27880, #31712, #5327, #24677, #2553, #15514, #11276, #37686, #34497, #8086, #41100, #31281, #8717, #11906, #34703, #24895, #24260, #21679, #4913, #17867, #5532, #30868, #1713, #14668, #25316, #25935, #2759, #22723, #28516, #15715 ),
 .UNSPECIFIED., .F., .F.,
 ( 4, 2, 2, 1, 1, 1, 1, 2, 2, 2, 1, 2, 2, 2, 2, 1, 1, 1, 2, 2, 2, 2, 1, 1, 1, 1, 2, 2, 2, 2, 1, 1, 2, 2, 2, 2, 2, 2, 2, 2, 2, 2, 2, 1, 2, 2, 2, 2, 2, 4 ),
 ( 0.000000000000000000, 0.1250000000000123512, 0.1875000000000185407, 0.2187500000000216216, 0.2343750000000231482, 0.2421875000000239253, 0.2460937500000243139, 0.2480468750000243139, 0.2500000000000243139, 0.3125000000000244804, 0.3437500000000247025, 0.3593750000000248135, 0.3750000000000248690, 0.4375000000000253686, 0.4687500000000257017, 0.4843750000000259792, 0.4921875000000259792, 0.4960937500000259792, 0.4980468750000258682, 0.5000000000000256462, 0.5625000000000250910, 0.5937500000000248690, 0.6093750000000248690, 0.6171875000000250910, 0.6210937500000254241, 0.6230468750000255351, 0.6240234375000253131, 0.6250000000000252021, 0.6875000000000200950, 0.7187500000000175415, 0.7343750000000163203, 0.7421875000000157652, 0.7460937500000154321, 0.7500000000000150990, 0.7812500000000131006, 0.7968750000000121014, 0.8125000000000111022, 0.8281250000000101030, 0.8359375000000096589, 0.8398437500000094369, 0.8437500000000093259, 0.8593750000000084377, 0.8671875000000079936, 0.8710937500000077716, 0.8730468750000076605, 0.8750000000000075495, 0.9062500000000056621, 0.9218750000000046629, 0.9375000000000037748, 1.000000000000000000 ),
 .UNSPECIFIED. ) ;
#26520 = CARTESIAN_POINT ( 'NONE',  ( -57.92026434645431010, 0.6774725698580426059, -0.9613144842853563743 ) ) ;
#26521 = CARTESIAN_POINT ( 'NONE',  ( 16.78381336521968237, 153.6818489539412553, 2.151947388239847214 ) ) ;
#26522 = CARTESIAN_POINT ( 'NONE',  ( 17.85428843624163520, 135.5811125208551857, -1.719929978336786291 ) ) ;
#26523 = CARTESIAN_POINT ( 'NONE',  ( -0.9497947497622778457, -2.244019015280241280, -0.2169513509177584398 ) ) ;
#26524 = CARTESIAN_POINT ( 'NONE',  ( 0.008945125900382298184, 117.5133074443058945, -0.4476506782301715726 ) ) ;
#26525 = CARTESIAN_POINT ( 'NONE',  ( 4.547353028811151887, 118.0891687680434359, -0.5919780852068863286 ) ) ;
#26526 = DIRECTION ( 'NONE',  ( -0.1951894777626509980, -0.9807655518882909540, 3.317599696243019336E-15 ) ) ;
#26527 = AXIS2_PLACEMENT_3D ( 'NONE', #23103, #23738, #36758 ) ;
#26528 = CARTESIAN_POINT ( 'NONE',  ( 5.181828529332998201, 120.8264575521020987, -0.4749581527667975922 ) ) ;
#26529 = CARTESIAN_POINT ( 'NONE',  ( -1.572870384098571162, 156.2570369995211479, 0.04660437260867185405 ) ) ;
#26530 = ORIENTED_EDGE ( 'NONE', *, *, #9615, .T. ) ;
#26531 = CARTESIAN_POINT ( 'NONE',  ( 0.01111639999512560942, 119.1634951276629550, -0.5563101126475826774 ) ) ;
#26533 = CARTESIAN_POINT ( 'NONE',  ( 3.313323393711395948, -15.78004832563367721, 4.785553473879357256 ) ) ;
#26532 = AXIS2_PLACEMENT_3D ( 'NONE', #5259, #12264, #21197 ) ;
#26534 =( REPRESENTATION_RELATIONSHIP ('NONE','NONE', #30767, #23419 ) REPRESENTATION_RELATIONSHIP_WITH_TRANSFORMATION ( #23623 )SHAPE_REPRESENTATION_RELATIONSHIP( ) );
#26535 = CARTESIAN_POINT ( 'NONE',  ( -4.989370312398730078, 31.45840840832646990, -0.6923657333659851698 ) ) ;
#26536 = CARTESIAN_POINT ( 'NONE',  ( -4.508402063874162202, 118.0683172002946861, -0.8182161505956602188 ) ) ;
#26537 = CARTESIAN_POINT ( 'NONE',  ( -51.02479983779974049, 14.46739584830851477, -4.600955224801065668 ) ) ;
#26538 = CARTESIAN_POINT ( 'NONE',  ( 4.149473596290089716, 118.2393519115161382, 0.3953539362545949176 ) ) ;
#26539 = CARTESIAN_POINT ( 'NONE',  ( 7.646026353518021068, 156.1362479297160348, 1.963328325631339411 ) ) ;
#26540 = DIRECTION ( 'NONE',  ( -0.9998004120163610509, -5.205824365704083805E-17, -0.01997839162482764261 ) ) ;
#26541 = CARTESIAN_POINT ( 'NONE',  ( 9.822473411059192472, 117.9943479623217399, 0.1962763949404991992 ) ) ;
#26542 = CARTESIAN_POINT ( 'NONE',  ( 8.403146708066456583, 17.13307930518084632, 0.5673920214783956251 ) ) ;
#26543 = CARTESIAN_POINT ( 'NONE',  ( 3.002817136647192964, 156.1079525116674631, 0.5547493173044987236 ) ) ;
#26544 = CARTESIAN_POINT ( 'NONE',  ( 22.85738479169573978, 148.8343141121478652, -0.6244747819152590695 ) ) ;
#26545 = CARTESIAN_POINT ( 'NONE',  ( -42.04985097881030498, 22.19100705996983436, -1.479702663569509413 ) ) ;
#26546 = VERTEX_POINT ( 'NONE', #21875 ) ;
#26547 = CARTESIAN_POINT ( 'NONE',  ( 0.3649948940937479125, 118.7629491485454025, 1.279691011652545285 ) ) ;
#26548 = UNCERTAINTY_MEASURE_WITH_UNIT (LENGTH_MEASURE( 1.000000000000000082E-05 ), #7512, 'distance_accuracy_value', 'NONE');
#26549 = CARTESIAN_POINT ( 'NONE',  ( -21.67502463668058255, 132.7302833492884417, -0.4113505826877427718 ) ) ;
#26550 = ORIENTED_EDGE ( 'NONE', *, *, #8135, .T. ) ;
#26551 = CARTESIAN_POINT ( 'NONE',  ( 5.481075915974320978, 120.6674672184742008, -0.5362211561704884888 ) ) ;
#26552 = CARTESIAN_POINT ( 'NONE',  ( -8.730044398489210877, 118.0746546384499140, 0.4875147713271164585 ) ) ;
#26553 = CARTESIAN_POINT ( 'NONE',  ( -9.378755113003734323, 124.2036136473707018, -0.5113998741172592899 ) ) ;
#26554 = CARTESIAN_POINT ( 'NONE',  ( 4.181132250215417123, -13.15738584483822038, 3.071181452022354819 ) ) ;
#26555 = CARTESIAN_POINT ( 'NONE',  ( -14.85424080674767211, 121.7713424311148032, 0.8456621969668064454 ) ) ;
#26556 = CARTESIAN_POINT ( 'NONE',  ( -7.868930244179279221, 69.75330307926518003, -1.269999999999995799 ) ) ;
#26557 = CARTESIAN_POINT ( 'NONE',  ( 13.43562511198101994, 156.9186530619738562, 0.2898375456858041654 ) ) ;
#26558 = EDGE_LOOP ( 'NONE', ( #32132, #35846, #32357, #41104 ) ) ;
#26559 = CARTESIAN_POINT ( 'NONE',  ( -0.2095918955067871126, -8.989892990265463624, -4.636818132431064221 ) ) ;
#26560 = CARTESIAN_POINT ( 'NONE',  ( -21.68875320759065062, 132.7412702629105468, -0.4333929054516006962 ) ) ;
#26561 = CARTESIAN_POINT ( 'NONE',  ( -6.059261036834475256, 57.15000000000000568, 5.016499999999999737 ) ) ;
#26562 = FACE_BOUND ( 'NONE', #5748, .T. ) ;
#26563 = CARTESIAN_POINT ( 'NONE',  ( -6.754070470910083834, 120.2528407669736765, 0.9389083524474073350 ) ) ;
#26564 = CARTESIAN_POINT ( 'NONE',  ( 2.990331240142678038, -7.206181497205274233, 3.547999066060627094 ) ) ;
#26565 = CARTESIAN_POINT ( 'NONE',  ( 2.946415863238953214, 117.2422168882539211, 0.6071713939981751018 ) ) ;
#26566 = DIRECTION ( 'NONE',  ( 0.9336303900108928744, 0.3582377630123714241, 0.000000000000000000 ) ) ;
#26568 = CARTESIAN_POINT ( 'NONE',  ( 0.02969037535068312292, 158.7301711276701894, -1.485827791648137275 ) ) ;
#26567 = CARTESIAN_POINT ( 'NONE',  ( -6.538677740023618411E-14, 75.27746620154573520, -7.356392042280733227E-18 ) ) ;
#26569 = CARTESIAN_POINT ( 'NONE',  ( -4.503669762702418033, -0.7216326387320324276, 1.072590735790061922 ) ) ;
#26570 = CARTESIAN_POINT ( 'NONE',  ( -4.831157780894042908, 117.2114307359545649, -0.6331281246675557473 ) ) ;
#26571 = ORIENTED_EDGE ( 'NONE', *, *, #16805, .T. ) ;
#26572 = CARTESIAN_POINT ( 'NONE',  ( -0.002455802209265526767, 120.8958299794632438, 0.1228983847502215371 ) ) ;
#26573 = CARTESIAN_POINT ( 'NONE',  ( 2.850629920820032748, -15.47419331854960056, 5.714803783126763292 ) ) ;
#26574 = AXIS2_PLACEMENT_3D ( 'NONE', #18762, #8566, #38590 ) ;
#26575 = CARTESIAN_POINT ( 'NONE',  ( -8.438477507926631205, 69.62414081991882142, -1.269999999999996021 ) ) ;
#26576 = CARTESIAN_POINT ( 'NONE',  ( -2.278603859588497205, 107.0255785817557665, -4.818371926714549502 ) ) ;
#26577 = ORIENTED_EDGE ( 'NONE', *, *, #2142, .T. ) ;
#26578 = CARTESIAN_POINT ( 'NONE',  ( 11.81048985551409913, 122.0047285378078357, 1.760929439237068239 ) ) ;
#26579 = CARTESIAN_POINT ( 'NONE',  ( -5.106395947886140263, 78.95054594174945350, 5.392902600000138769 ) ) ;
#26580 = CARTESIAN_POINT ( 'NONE',  ( -46.95911617132933458, 24.98948415085536823, -1.986615011824472088 ) ) ;
#26581 = CARTESIAN_POINT ( 'NONE',  ( -17.95360460524307555, 154.0540368679750998, 0.8775891217286384549 ) ) ;
#26582 = CARTESIAN_POINT ( 'NONE',  ( 4.500746820419270655, 24.54286538861932598, -7.153999163526271410 ) ) ;
#26583 = CARTESIAN_POINT ( 'NONE',  ( 15.92638198489182066, 148.2453349897154737, 1.585317681524597955 ) ) ;
#26584 = ADVANCED_FACE ( 'NONE', ( #22086 ), #5516, .T. ) ;
#26585 = CARTESIAN_POINT ( 'NONE',  ( 8.196853576809875364, 117.5993832199734328, -0.1745776481207346187 ) ) ;
#26586 = CARTESIAN_POINT ( 'NONE',  ( 10.28897677580358305, 57.14999999999999858, -5.016499999999999737 ) ) ;
#26587 = CARTESIAN_POINT ( 'NONE',  ( -49.16877686933415248, 17.52905763403498085, 5.029729607253535129 ) ) ;
#26588 = CARTESIAN_POINT ( 'NONE',  ( -47.99264284736476327, 22.55967899981254376, 2.517363275470459794 ) ) ;
#26589 = AXIS2_PLACEMENT_3D ( 'NONE', #35913, #10118, #2906 ) ;
#26590 = DIRECTION ( 'NONE',  ( -1.000000000000000000, 1.288607544181256449E-16, 0.000000000000000000 ) ) ;
#26591 = CARTESIAN_POINT ( 'NONE',  ( -53.65759266121656879, 11.01975743955735432, 4.003319250743206936 ) ) ;
#26592 = CARTESIAN_POINT ( 'NONE',  ( -58.29986746207860904, 0.4137999759807384215, 1.006442112984123227 ) ) ;
#26593 = EDGE_CURVE ( 'NONE', #36287, #22648, #8700, .T. ) ;
#26594 = CARTESIAN_POINT ( 'NONE',  ( -4.413217288059840371, 118.1641560473096888, 0.4831912002420357122 ) ) ;
#26595 = DIRECTION ( 'NONE',  ( 0.000000000000000000, 0.000000000000000000, 1.000000000000000000 ) ) ;
#26596 = B_SPLINE_SURFACE_WITH_KNOTS ( 'NONE', 1, 3, ( 
 ( #19604, #23003, #39222, #6640, #32616, #3449, #16626, #32832, #16412, #29418, #258, #36244, #36031, #26216, #7064, #13233, #32202, #6844 ),
 ( #19815, #3035, #3661, #20028, #33046, #16842, #29842, #680, #28326, #2574, #37488, #2360, #18721, #21487, #27899, #5345, #34103, #11924 ) ),
 .UNSPECIFIED., .F., .F., .F.,
 ( 2, 2 ),
 ( 4, 2, 2, 2, 2, 2, 2, 2, 4 ),
 ( 0.000000000000000000, 1.000000000000000000 ),
 ( 0.000000000000000000, 0.2500000000000000000, 0.5000000000000000000, 0.6250000000000000000, 0.7500000000000000000, 0.8125000000000000000, 0.8750000000000000000, 0.9375000000000000000, 1.000000000000000000 ),
 .UNSPECIFIED. ) ;
#26597 = ORIENTED_EDGE ( 'NONE', *, *, #8405, .F. ) ;
#26598 = CARTESIAN_POINT ( 'NONE',  ( -44.13308345971568514, 24.21351174012166396, 1.567149544246648762 ) ) ;
#26599 = CARTESIAN_POINT ( 'NONE',  ( -3.864517893783868008, 119.0220221803404286, -0.9271182341797493676 ) ) ;
#26600 = CARTESIAN_POINT ( 'NONE',  ( -1.973215784349786839, 106.6933082031156772, -4.964841027628618342 ) ) ;
#26602 = CARTESIAN_POINT ( 'NONE',  ( 4.585520833345769987, 118.0414727501857897, 0.8249672653002678713 ) ) ;
#26601 = TOROIDAL_SURFACE ( 'NONE', #40878, 4.826000000000000512, 0.5080000000000000071 ) ;
#26603 = CARTESIAN_POINT ( 'NONE',  ( -2.692664463852660450, 120.6505882111413683, -0.3986361418428904235 ) ) ;
#26604 = CARTESIAN_POINT ( 'NONE',  ( 4.829164506186364392, 117.3993836135881565, -1.010517262250789194 ) ) ;
#26605 = CARTESIAN_POINT ( 'NONE',  ( 2.677032024553319012, 107.2224589468338536, -4.627058715154634960 ) ) ;
#26606 = CARTESIAN_POINT ( 'NONE',  ( -17.20807765353001528, 147.1820577694790018, -2.053081559533529887 ) ) ;
#26607 = EDGE_CURVE ( 'NONE', #14618, #31748, #17461, .T. ) ;
#26608 = CARTESIAN_POINT ( 'NONE',  ( -17.14500000000466784, 71.11999999999886768, 1.269999999999998241 ) ) ;
#26609 = CARTESIAN_POINT ( 'NONE',  ( 7.880211965457339041, 122.2234151243416989, -0.4724049390182752939 ) ) ;
#26610 = CARTESIAN_POINT ( 'NONE',  ( -1.556981180954984945, 156.2629499403934119, 0.08452657509653109524 ) ) ;
#26611 = CARTESIAN_POINT ( 'NONE',  ( -4.288638401707804526, -7.253218809911426312, -1.756103832032595680 ) ) ;
#26612 = CARTESIAN_POINT ( 'NONE',  ( 13.11470433356379139, 119.8381915656929380, 0.9809890993017411631 ) ) ;
#26613 = CARTESIAN_POINT ( 'NONE',  ( 5.010184479710102501, 117.3993854065330851, 0.7504461923096029663 ) ) ;
#26614 = CARTESIAN_POINT ( 'NONE',  ( 3.240743527130751200, -15.12236442990058727, 3.435505395146291274 ) ) ;
#26615 = CARTESIAN_POINT ( 'NONE',  ( -9.673022701212307339, 121.1143850344477215, 1.180881524473704980 ) ) ;
#26616 = CARTESIAN_POINT ( 'NONE',  ( -0.5387148418522960114, 9.198764818822382949, 0.8109227438555447476 ) ) ;
#26617 = CARTESIAN_POINT ( 'NONE',  ( -0.3196863354300110704, 116.7093555017326452, -0.2333483032394376433 ) ) ;
#26618 = CARTESIAN_POINT ( 'NONE',  ( 0.9169382621377788478, -11.15192339915171793, 0.3232733857163304081 ) ) ;
#26619 = EDGE_LOOP ( 'NONE', ( #7398, #29460 ) ) ;
#26620 = CARTESIAN_POINT ( 'NONE',  ( -45.30933510662926977, 19.89173180141312614, 2.333898071402933816 ) ) ;
#26621 = CARTESIAN_POINT ( 'NONE',  ( 4.807558371750517701, 117.0601473006971105, 0.9798501506189062349 ) ) ;
#26622 = CARTESIAN_POINT ( 'NONE',  ( -0.6059414056334104792, 120.5739061664170606, 0.2722191786371237487 ) ) ;
#26623 = EDGE_CURVE ( 'NONE', #25646, #21812, #38826, .T. ) ;
#26624 = CARTESIAN_POINT ( 'NONE',  ( 3.953338583042130150, -12.61280045678425665, 2.014973703158344787 ) ) ;
#26625 = CARTESIAN_POINT ( 'NONE',  ( 5.873575024772715203, 120.4133487461328826, -0.7716123655894259192 ) ) ;
#26626 = CARTESIAN_POINT ( 'NONE',  ( -18.24829758291891579, 150.1405190176936344, -2.471583571221721343 ) ) ;
#26627 = CARTESIAN_POINT ( 'NONE',  ( -17.22465686008793995, 48.97870818484556565, -1.269999999999997131 ) ) ;
#26628 = CIRCLE ( 'NONE', #40896, 0.2540000000000045555 ) ;
#26629 = CARTESIAN_POINT ( 'NONE',  ( 2.104008947125556528, -15.14483647969354330, 5.217645225406672971 ) ) ;
#26630 = CARTESIAN_POINT ( 'NONE',  ( -4.842996840569961492, 117.4782722638060761, -1.161985943875174065 ) ) ;
#26631 = EDGE_CURVE ( 'NONE', #7830, #12023, #11063, .T. ) ;
#26632 = CARTESIAN_POINT ( 'NONE',  ( 2.818990841020078797, 121.0122979933374978, -0.009253692138209281687 ) ) ;
#26633 = ORIENTED_EDGE ( 'NONE', *, *, #38625, .F. ) ;
#26634 = CARTESIAN_POINT ( 'NONE',  ( -4.798386392178022319, 114.9758031406785221, 1.576502096137255782 ) ) ;
#26635 = DIRECTION ( 'NONE',  ( -0.8745520943968235761, 0.4849315768086558398, -5.691349986800547879E-16 ) ) ;
#26636 = EDGE_CURVE ( 'NONE', #20372, #32706, #15453, .T. ) ;
#26637 = CIRCLE ( 'NONE', #35496, 0.2540000000000010583 ) ;
#26638 = CARTESIAN_POINT ( 'NONE',  ( 11.58677707360137710, 55.24500000000000455, -4.474811398758258285 ) ) ;
#26639 = CARTESIAN_POINT ( 'NONE',  ( 23.38383716176057803, 142.7868430859564626, 0.3143897558744219167 ) ) ;
#26640 = CARTESIAN_POINT ( 'NONE',  ( -4.060783872423834318, 109.8065891650451249, 3.521960838153598505 ) ) ;
#26641 = AXIS2_PLACEMENT_3D ( 'NONE', #6698, #19667, #3727 ) ;
#26642 = CARTESIAN_POINT ( 'NONE',  ( -3.107210190573434616, 118.0750721850716474, 0.8420533518679624851 ) ) ;
#26643 = CARTESIAN_POINT ( 'NONE',  ( 11.32678463655034129, 56.02547433970789115, 4.456118031212549013 ) ) ;
#26644 = CARTESIAN_POINT ( 'NONE',  ( 0.2629046284512602805, 36.79895747838261855, -0.7350018967835904027 ) ) ;
#26645 = CARTESIAN_POINT ( 'NONE',  ( 20.66962185543543384, 147.7542213611591535, 2.445644978772825162 ) ) ;
#26646 = CARTESIAN_POINT ( 'NONE',  ( 3.707542801486926276, 23.89195667223011910, -2.776928957275885068 ) ) ;
#26647 = CARTESIAN_POINT ( 'NONE',  ( -7.328769482851726025, 13.23335216599729947, 4.212906450523355772 ) ) ;
#26648 = CARTESIAN_POINT ( 'NONE',  ( -5.518892555433418501, 117.8876361237244907, -1.069160601140542344 ) ) ;
#26649 = CARTESIAN_POINT ( 'NONE',  ( -0.7466139261200300803, 119.9044272045951374, -0.6467483038796004724 ) ) ;
#26650 = DIRECTION ( 'NONE',  ( -1.011795553208986377E-16, -1.000000000000000000, 0.000000000000000000 ) ) ;
#26651 = AXIS2_PLACEMENT_3D ( 'NONE', #18505, #31510, #2357 ) ;
#26652 = CARTESIAN_POINT ( 'NONE',  ( -3.056332105116442932, 108.4800906826746143, -4.214630652369057096 ) ) ;
#26653 = CARTESIAN_POINT ( 'NONE',  ( -4.814395258470165473, 104.6144662015522755, 2.302979290232680221 ) ) ;
#26654 = VECTOR ( 'NONE', #32897, 1000.000000000000114 ) ;
#26655 = CARTESIAN_POINT ( 'NONE',  ( -0.01876340930523686876, 19.73428105357427853, -4.634220987317214657 ) ) ;
#26656 = CARTESIAN_POINT ( 'NONE',  ( -10.12396263145945774, 65.41168055974398499, 1.270000000000002904 ) ) ;
#26657 = CARTESIAN_POINT ( 'NONE',  ( -15.27962295839633811, 80.49293118800726177, -1.524000000000001576 ) ) ;
#26658 = CARTESIAN_POINT ( 'NONE',  ( 2.604768916882071128, -14.79682312136586297, 4.847387382002324330 ) ) ;
#26659 = CARTESIAN_POINT ( 'NONE',  ( 3.306315723242806648, 118.9685052735122355, -0.5531158949559312754 ) ) ;
#26660 = CARTESIAN_POINT ( 'NONE',  ( -14.83366055447124943, 120.8492938200443092, 0.4607208393402018043 ) ) ;
#26661 = CARTESIAN_POINT ( 'NONE',  ( 4.854437695190745750, 117.4070755028450748, -0.9982814861801205808 ) ) ;
#26662 = ORIENTED_EDGE ( 'NONE', *, *, #15232, .T. ) ;
#26663 = LINE ( 'NONE', #39671, #28391 ) ;
#26664 = EDGE_LOOP ( 'NONE', ( #26025, #27801, #19276, #12889 ) ) ;
#26665 = CARTESIAN_POINT ( 'NONE',  ( 0.1949087904810302418, 33.82644263972942156, 0.4054292462034596034 ) ) ;
#26666 = CARTESIAN_POINT ( 'NONE',  ( 4.998192975942944649, -15.53260140147937030, 2.284796345537305928 ) ) ;
#26667 = CARTESIAN_POINT ( 'NONE',  ( -13.23674331388984093, 122.5785676075921060, 1.297564987558605498 ) ) ;
#26668 = CARTESIAN_POINT ( 'NONE',  ( 18.02024205669863477, 128.5942011134444272, -1.207605415130186710 ) ) ;
#26669 = CARTESIAN_POINT ( 'NONE',  ( 0.8991110484329473129, 28.35728145135693268, -0.3789830077994447155 ) ) ;
#26670 = CARTESIAN_POINT ( 'NONE',  ( 5.981046608238687057, 78.88093534801383555, 5.016500000000000625 ) ) ;
#26671 = EDGE_CURVE ( 'NONE', #34241, #20108, #40215, .T. ) ;
#26672 = ORIENTED_EDGE ( 'NONE', *, *, #18294, .T. ) ;
#26673 = CARTESIAN_POINT ( 'NONE',  ( -4.967168320455268571, 117.4023968188195681, -1.002192383175803503 ) ) ;
#26674 = CARTESIAN_POINT ( 'NONE',  ( 2.033169340629980226, 122.5452913651401587, 0.2335185838714209372 ) ) ;
#26675 = CARTESIAN_POINT ( 'NONE',  ( -10.38102865001225261, 154.1877054190025262, 1.364427777124047392 ) ) ;
#26676 = DIRECTION ( 'NONE',  ( -0.01997839162482737546, -1.040247600000939284E-18, 0.9998004120163610509 ) ) ;
#26677 =( BOUNDED_CURVE ( )  B_SPLINE_CURVE ( 3, ( #3388, #16354, #19136, #3607 ),
 .UNSPECIFIED., .F., .T. ) 
 B_SPLINE_CURVE_WITH_KNOTS ( ( 4, 4 ),
 ( 0.6093138467282562809, 1.570796326794900111 ),
 .UNSPECIFIED. ) 
 CURVE ( )  GEOMETRIC_REPRESENTATION_ITEM ( )  RATIONAL_B_SPLINE_CURVE ( ( 1.000000000000000000, 0.9244349266169025192, 0.9244349266169025192, 1.000000000000000000 ) ) 
 REPRESENTATION_ITEM ( '' )  );
#26678 = EDGE_CURVE ( 'NONE', #13951, #6380, #23853, .T. ) ;
#26679 = CARTESIAN_POINT ( 'NONE',  ( 18.37664568872238036, 148.6295804641074483, -1.698537578660717751 ) ) ;
#26680 = CARTESIAN_POINT ( 'NONE',  ( -4.954158841009661529, 118.5534682650580862, -1.066189120819955205 ) ) ;
#26681 = DIRECTION ( 'NONE',  ( -0.9998004120163608288, -4.016384292689131511E-17, -0.01997839162482749342 ) ) ;
#26682 = VERTEX_POINT ( 'NONE', #24612 ) ;
#26683 = CARTESIAN_POINT ( 'NONE',  ( 4.373555915921281567, 118.1839305412106000, -0.4384691235614320837 ) ) ;
#26684 = CARTESIAN_POINT ( 'NONE',  ( 1.677891416185167017, 156.3096136994911092, -0.5101806352362399100 ) ) ;
#26685 = EDGE_LOOP ( 'NONE', ( #17635, #7384 ) ) ;
#26686 = CARTESIAN_POINT ( 'NONE',  ( 2.112177293979604187, -15.34403890755049815, 5.167321579062071457 ) ) ;
#26687 = EDGE_CURVE ( 'NONE', #11397, #39243, #8228, .T. ) ;
#26688 = DIRECTION ( 'NONE',  ( 5.188838149069472160E-16, -1.699382548006136559E-16, -1.000000000000000000 ) ) ;
#26689 = CIRCLE ( 'NONE', #8319, 0.3809999999999984510 ) ;
#26690 = EDGE_CURVE ( 'NONE', #7253, #18068, #9556, .T. ) ;
#26691 = B_SPLINE_CURVE_WITH_KNOTS ( 'NONE', 3,
 ( #9591, #18960, #18748, #28351, #41360, #31967 ),
 .UNSPECIFIED., .F., .F.,
 ( 4, 2, 4 ),
 ( 0.7472851912383878803, 0.8736425956191939957, 1.000000000000000000 ),
 .UNSPECIFIED. ) ;
#26692 = CARTESIAN_POINT ( 'NONE',  ( -48.43799250123541356, 18.62746361536937911, 5.176101822176825351 ) ) ;
#26693 = CARTESIAN_POINT ( 'NONE',  ( 3.490194016315742331, 12.22236127277748174, 3.029891289224248219 ) ) ;
#26694 = CARTESIAN_POINT ( 'NONE',  ( 9.008986559116410220, 121.9018297702777858, 1.332107995734232109 ) ) ;
#26695 = CARTESIAN_POINT ( 'NONE',  ( -1.007477757134449536, 31.95321293912196836, 2.022349366842921103 ) ) ;
#26696 = EDGE_CURVE ( 'NONE', #41779, #26975, #25224, .T. ) ;
#26697 = CARTESIAN_POINT ( 'NONE',  ( -1.576536484031922480, 10.66345178295009788, -4.350723848753511369 ) ) ;
#26698 = CARTESIAN_POINT ( 'NONE',  ( 5.289698609639951421, 121.3432423864224177, 0.1753557357117460358 ) ) ;
#26699 = CARTESIAN_POINT ( 'NONE',  ( -30.45812239790965492, 71.16801738242446618, -1.524000000000007793 ) ) ;
#26700 = CIRCLE ( 'NONE', #10373, 7.461249999999999716 ) ;
#26701 = CARTESIAN_POINT ( 'NONE',  ( -50.52646075385809610, 14.05410990099204049, -2.888145277534023947 ) ) ;
#26702 = CARTESIAN_POINT ( 'NONE',  ( 2.163736596230561027, 116.3505410131987787, -0.2071778447972208170 ) ) ;
#26703 = CARTESIAN_POINT ( 'NONE',  ( 15.19604463793433169, 156.0859089222169587, 0.3036531364422415669 ) ) ;
#26704 = CYLINDRICAL_SURFACE ( 'NONE', #179, 2.540000000000002256 ) ;
#26705 = DIRECTION ( 'NONE',  ( 0.9998004120163609398, 4.016384292689130894E-17, 0.01997839162482749689 ) ) ;
#26706 = CARTESIAN_POINT ( 'NONE',  ( 5.314256983240370324, 105.1224655745845382, -0.4585143440169748841 ) ) ;
#26707 = CARTESIAN_POINT ( 'NONE',  ( -5.965356522962928842, 65.30181249999996851, 5.016499999999999737 ) ) ;
#26708 = CARTESIAN_POINT ( 'NONE',  ( -46.95911617132934879, 24.98948415085533270, 1.986615011824473864 ) ) ;
#26709 = CARTESIAN_POINT ( 'NONE',  ( -33.20758249455312239, 49.81222039523557044, 1.523999999999993804 ) ) ;
#26710 = CARTESIAN_POINT ( 'NONE',  ( -58.73915225836901044, 0.1638436772961188170, -1.071698628919754437E-14 ) ) ;
#26711 = CARTESIAN_POINT ( 'NONE',  ( -57.26626398570029863, 3.526386058942967860, 2.205039086913747948 ) ) ;
#26712 = CARTESIAN_POINT ( 'NONE',  ( -22.51579307796286145, 137.1624432810789358, -0.01304004454942945049 ) ) ;
#26713 = ORIENTED_EDGE ( 'NONE', *, *, #33225, .F. ) ;
#26714 = CARTESIAN_POINT ( 'NONE',  ( -56.91937565786339803, 5.591339438888828894, -1.085802076254212195E-14 ) ) ;
#26715 = CARTESIAN_POINT ( 'NONE',  ( -6.982215578972839509, 121.9499294214156464, -0.1835727084940861342 ) ) ;
#26716 = EDGE_LOOP ( 'NONE', ( #11481, #32902, #7488, #13143 ) ) ;
#26717 = CARTESIAN_POINT ( 'NONE',  ( 3.794806421782703776, 115.7029491485452724, -1.459834282783267767 ) ) ;
#26718 = CARTESIAN_POINT ( 'NONE',  ( -15.77055413937423367, 146.5697412905949477, -0.3665361178749758087 ) ) ;
#26719 = CARTESIAN_POINT ( 'NONE',  ( 6.311525104866394287, -14.07095602924590594, 0.9561848504773229340 ) ) ;
#26720 = CARTESIAN_POINT ( 'NONE',  ( -1.147165779964402832, 117.8708904510121016, 0.5694250185432009337 ) ) ;
#26721 = CARTESIAN_POINT ( 'NONE',  ( 4.622858883031034871, 26.85595184169372018, 0.2084198311932835834 ) ) ;
#26722 = AXIS2_PLACEMENT_3D ( 'NONE', #12422, #2217, #5625 ) ;
#26723 = CARTESIAN_POINT ( 'NONE',  ( 22.90211176506257829, 150.1344166263168347, 0.9094179090926688414 ) ) ;
#26724 = CARTESIAN_POINT ( 'NONE',  ( 14.67165028172560604, 148.8681294118411813, 0.4913509943341035635 ) ) ;
#26725 = CARTESIAN_POINT ( 'NONE',  ( 4.037907715354051241, 27.70556447992504445, -2.267523456217593214 ) ) ;
#26726 = CARTESIAN_POINT ( 'NONE',  ( 0.1248384507886338285, 1.166626901725996035, -0.9703616065359238485 ) ) ;
#26727 = CARTESIAN_POINT ( 'NONE',  ( -8.204617290884389291, 117.5299140688306352, -0.3545595769132391384 ) ) ;
#26728 = CARTESIAN_POINT ( 'NONE',  ( 5.475330206976797953, 57.14999999999999858, -5.107412922131463695 ) ) ;
#26729 = CARTESIAN_POINT ( 'NONE',  ( 4.862391452034746209, 117.4079971399760609, 1.166187604725966054 ) ) ;
#26730 = ORIENTED_EDGE ( 'NONE', *, *, #14115, .T. ) ;
#26731 = CARTESIAN_POINT ( 'NONE',  ( 2.218330162228713043, 116.2574865890770184, 0.1610120948260720108 ) ) ;
#26732 = CARTESIAN_POINT ( 'NONE',  ( -3.787250209144910507, 156.8112981010400802, 1.501541828261893308 ) ) ;
#26733 = CARTESIAN_POINT ( 'NONE',  ( -57.76243589657412514, 1.018525044351360709, -1.139292060318100042 ) ) ;
#26734 = CARTESIAN_POINT ( 'NONE',  ( -0.01023305610377599727, 117.8848902025789158, 0.5121039721716187376 ) ) ;
#26735 = CARTESIAN_POINT ( 'NONE',  ( 6.722174884993919797, 119.4737997143703012, -1.022258653430867970 ) ) ;
#26736 = CARTESIAN_POINT ( 'NONE',  ( 0.6771123631923940955, -5.471153235863896569, -0.7014129483058207937 ) ) ;
#26737 = CARTESIAN_POINT ( 'NONE',  ( -9.211590693262630580, 119.0402042963619351, -1.266790605762086575 ) ) ;
#26738 = CARTESIAN_POINT ( 'NONE',  ( 4.683543233604185119, 118.0095664619904028, -0.5959560594456849714 ) ) ;
#26739 = VECTOR ( 'NONE', #31888, 1000.000000000000000 ) ;
#26740 = DIRECTION ( 'NONE',  ( -0.9807655518882955059, 0.1951894777626270172, -8.537024980200854359E-16 ) ) ;
#26741 = AXIS2_PLACEMENT_3D ( 'NONE', #9819, #22785, #27012 ) ;
#26742 = CARTESIAN_POINT ( 'NONE',  ( 7.857169925943599864, 121.9903164032602518, -0.5981771023335124005 ) ) ;
#26743 = CARTESIAN_POINT ( 'NONE',  ( 4.792324638223571576, 56.51998046905274009, -4.972049999999996750 ) ) ;
#26744 = ORIENTED_EDGE ( 'NONE', *, *, #3971, .F. ) ;
#26745 = CARTESIAN_POINT ( 'NONE',  ( -11.21148455117568687, 122.4230570912197038, -1.693600966768365357 ) ) ;
#26746 = CARTESIAN_POINT ( 'NONE',  ( 2.515823494799488191, -15.76102479606726625, 5.403604998519412561 ) ) ;
#26747 = CARTESIAN_POINT ( 'NONE',  ( -4.558369097197020992, 31.49133049583777932, -0.6947524270963534310 ) ) ;
#26748 = CARTESIAN_POINT ( 'NONE',  ( -4.656319957792719677, 118.0096513897839685, -0.7824823237528982789 ) ) ;
#26749 = EDGE_CURVE ( 'NONE', #27753, #32986, #16357, .T. ) ;
#26750 = CARTESIAN_POINT ( 'NONE',  ( -53.65759266121656879, 11.01975743955735432, -4.003319250743225588 ) ) ;
#26751 = CARTESIAN_POINT ( 'NONE',  ( 4.065926199369043204, 118.2429491485453354, 0.3080910687088499467 ) ) ;
#26752 = CARTESIAN_POINT ( 'NONE',  ( 18.33584167903955731, 146.8095856830544790, 2.399012226062094744 ) ) ;
#26753 = FACE_OUTER_BOUND ( 'NONE', #17292, .T. ) ;
#26754 = VECTOR ( 'NONE', #31257, 1000.000000000000000 ) ;
#26755 = CARTESIAN_POINT ( 'NONE',  ( -6.439802422954663176E-14, 159.6054662015457382, 9.942593405483322146E-17 ) ) ;
#26756 = CARTESIAN_POINT ( 'NONE',  ( 8.424193198035354158, 17.36166136180145259, -0.6763034115371487909 ) ) ;
#26757 = CARTESIAN_POINT ( 'NONE',  ( 9.078381139985610915, 123.6795089456687577, 0.5923855214342147457 ) ) ;
#26758 = CARTESIAN_POINT ( 'NONE',  ( 21.72212103179832710, 136.7703657609320658, -0.7093728523935389774 ) ) ;
#26759 = CARTESIAN_POINT ( 'NONE',  ( -9.795036404550216957, 65.29837086945681790, -1.269999999999996021 ) ) ;
#26760 = ORIENTED_EDGE ( 'NONE', *, *, #32338, .T. ) ;
#26761 = LINE ( 'NONE', #39554, #11329 ) ;
#26762 = CIRCLE ( 'NONE', #28114, 0.2539999999999978941 ) ;
#26763 = CARTESIAN_POINT ( 'NONE',  ( -23.29076518286613862, 149.3500807853454546, -0.3882996703880463585 ) ) ;
#26764 = ORIENTED_EDGE ( 'NONE', *, *, #25293, .F. ) ;
#26765 = CARTESIAN_POINT ( 'NONE',  ( -5.326936277661974195, 120.5144646293056780, -0.7944123752729133070 ) ) ;
#26766 = CARTESIAN_POINT ( 'NONE',  ( -10.73808814597608574, 77.14487411131506178, 1.524000000000001132 ) ) ;
#26767 = VERTEX_POINT ( 'NONE', #37825 ) ;
#26768 = CARTESIAN_POINT ( 'NONE',  ( -10.53234188159483686, 153.0603347025997323, -0.7465333597200853877 ) ) ;
#26769 = CARTESIAN_POINT ( 'NONE',  ( 3.953338583042130150, -12.61280045678425665, 2.014973703158344787 ) ) ;
#26770 = CARTESIAN_POINT ( 'NONE',  ( -17.38882309766602319, 125.1846915036903027, 0.8043053978789255209 ) ) ;
#26771 = CARTESIAN_POINT ( 'NONE',  ( -4.218275339060285845, 155.8585684991085714, -0.08429118021179402009 ) ) ;
#26772 = CARTESIAN_POINT ( 'NONE',  ( 3.300851927471557090, 159.4676453237595410, 0.08072286411353209179 ) ) ;
#26773 = ORIENTED_EDGE ( 'NONE', *, *, #18254, .T. ) ;
#26774 = CARTESIAN_POINT ( 'NONE',  ( 3.746277899330032302, -0.8937244826341392834, -2.755274729908455900 ) ) ;
#26775 = CARTESIAN_POINT ( 'NONE',  ( -0.8860745468267199332, 116.4323782974132513, -0.03055428320029199979 ) ) ;
#26776 = CARTESIAN_POINT ( 'NONE',  ( -26.29578028364076658, 73.87584665086983193, -1.270000000000006013 ) ) ;
#26777 = DIRECTION ( 'NONE',  ( -0.9891443546370349837, 0.000000000000000000, 0.1469470846586743984 ) ) ;
#26778 = CARTESIAN_POINT ( 'NONE',  ( 8.223111631096672980, 120.3648856214035590, 1.439954315622481662 ) ) ;
#26779 = CARTESIAN_POINT ( 'NONE',  ( -3.522755225739859775, -9.592572062075928940, 3.019445982675781348 ) ) ;
#26780 = CARTESIAN_POINT ( 'NONE',  ( 15.97393847379841070, 155.1095016151506911, 1.658827062323852797 ) ) ;
#26781 = CARTESIAN_POINT ( 'NONE',  ( -58.36601048454644314, 0.2708230324007659950, -0.9148880203699379932 ) ) ;
#26783 = CARTESIAN_POINT ( 'NONE',  ( 19.67014042257518724, 150.6586468064772646, -1.570413873854537234 ) ) ;
#26782 = CARTESIAN_POINT ( 'NONE',  ( 5.706393392168676471, 56.51499999999914792, 5.041882957346167871 ) ) ;
#26784 = CIRCLE ( 'NONE', #37009, 0.2539999999999973390 ) ;
#26785 = CARTESIAN_POINT ( 'NONE',  ( -2.329872802932658082, -2.670747431267189498, -3.990024091085845548 ) ) ;
#26786 = CARTESIAN_POINT ( 'NONE',  ( -22.05995121575398343, 150.4421090420883900, -1.612468304426259103 ) ) ;
#26787 = VERTEX_POINT ( 'NONE', #14604 ) ;
#26788 = AXIS2_PLACEMENT_3D ( 'NONE', #24414, #8458, #21625 ) ;
#26789 = CARTESIAN_POINT ( 'NONE',  ( -0.6772589037151361957, 156.3292479207028407, 0.3306685775513075742 ) ) ;
#26790 = CARTESIAN_POINT ( 'NONE',  ( 4.840206765044483994, -15.05961300585426166, 4.264492456498921946 ) ) ;
#26791 = CARTESIAN_POINT ( 'NONE',  ( -42.63057730194618244, 21.82620848986212181, 1.774738817929873758 ) ) ;
#26792 = TOROIDAL_SURFACE ( 'NONE', #4376, 3.683000000000000718, 0.5080000000000000071 ) ;
#26793 = CARTESIAN_POINT ( 'NONE',  ( -3.582589445373201009, 109.6950671057752373, -3.736549424469191916 ) ) ;
#26794 = ORIENTED_EDGE ( 'NONE', *, *, #20356, .F. ) ;
#26795 = CARTESIAN_POINT ( 'NONE',  ( 8.358437701610622383, 156.6436466068687423, 2.074018175080058146 ) ) ;
#26796 = CARTESIAN_POINT ( 'NONE',  ( -6.617255152258657249E-14, 94.83546620154572793, -2.708805023911452991E-18 ) ) ;
#26797 = CIRCLE ( 'NONE', #17272, 0.5080000000000000071 ) ;
#26798 = CARTESIAN_POINT ( 'NONE',  ( -30.08804090436192169, 69.76339842363584864, -1.270000000000007345 ) ) ;
#26799 = CARTESIAN_POINT ( 'NONE',  ( -15.15503192428649371, 121.4505734225448066, 0.6300967139502822167 ) ) ;
#26800 = CARTESIAN_POINT ( 'NONE',  ( -4.414756536061148928, 7.050034479431100287, -7.184669936685727620 ) ) ;
#26801 = CARTESIAN_POINT ( 'NONE',  ( 15.33786013020720773, 149.0334586719817764, 1.566117276479743303 ) ) ;
#26802 = FACE_OUTER_BOUND ( 'NONE', #14545, .T. ) ;
#26803 = CARTESIAN_POINT ( 'NONE',  ( 14.99898601413110022, 156.1447123740162226, -0.3355057415612999749 ) ) ;
#26804 = DIRECTION ( 'NONE',  ( 1.000000000000000000, 0.000000000000000000, 0.000000000000000000 ) ) ;
#26805 = AXIS2_PLACEMENT_3D ( 'NONE', #42008, #39014, #22788 ) ;
#26806 = CARTESIAN_POINT ( 'NONE',  ( -56.16595168976004970, 4.414070172726168195, 2.362198540470026309 ) ) ;
#26807 = CARTESIAN_POINT ( 'NONE',  ( -47.63491852694408379, 24.04202919463459409, 1.290898778641160094 ) ) ;
#26808 = CARTESIAN_POINT ( 'NONE',  ( -3.212720104892762052, 117.3993812109657711, 1.261607097357493323 ) ) ;
#26809 = CARTESIAN_POINT ( 'NONE',  ( -49.59816314059867182, 17.91649583374774224, 5.069000701391649599 ) ) ;
#26810 = CARTESIAN_POINT ( 'NONE',  ( -58.59441299015681182, -0.2213268877428872239, 0.4750018593813392642 ) ) ;
#26811 = CARTESIAN_POINT ( 'NONE',  ( -4.407706242951269893, 118.1630026188911415, 0.4884894518719885559 ) ) ;
#26812 = CARTESIAN_POINT ( 'NONE',  ( 3.893689849856083462, 109.0594030058512232, -3.652599047905514595 ) ) ;
#26813 = VERTEX_POINT ( 'NONE', #14815 ) ;
#26814 = CARTESIAN_POINT ( 'NONE',  ( -46.25688858429102623, 20.73875112231587892, 4.700046123029338219 ) ) ;
#26815 = CARTESIAN_POINT ( 'NONE',  ( 3.996284611207044257, 119.1072997412182701, -0.7644371380813023142 ) ) ;
#26816 = CARTESIAN_POINT ( 'NONE',  ( -7.112984908206943402, 122.4243137415680280, -0.2517356677811183885 ) ) ;
#26817 = CARTESIAN_POINT ( 'NONE',  ( 4.508147239578550902, 118.0682817303566310, 0.8183067226364422186 ) ) ;
#26818 = CARTESIAN_POINT ( 'NONE',  ( -3.128511139047554401, 156.1781389015385457, -0.8559903927114130839 ) ) ;
#26819 = AXIS2_PLACEMENT_3D ( 'NONE', #5337, #25119, #38120 ) ;
#26820 = CARTESIAN_POINT ( 'NONE',  ( -1.557005993388528964, 115.7027528728559531, -1.730858768160303596 ) ) ;
#26821 = CARTESIAN_POINT ( 'NONE',  ( -5.309060684617390516E-14, 83.56599999999998829, 0.000000000000000000 ) ) ;
#26822 = CARTESIAN_POINT ( 'NONE',  ( -6.656543858376176668E-14, 104.6144662015457243, -3.850115147268248130E-19 ) ) ;
#26823 = CARTESIAN_POINT ( 'NONE',  ( -0.7897433827105079240, 156.7682548876429109, -1.239156740209750307 ) ) ;
#26824 = CARTESIAN_POINT ( 'NONE',  ( -6.583861033951825950E-14, 91.02546620154572565, 1.480257718193877056E-29 ) ) ;
#26825 = CARTESIAN_POINT ( 'NONE',  ( -45.93641268020314783, 20.77718376654426180, 4.359287402722423543 ) ) ;
#26826 = CARTESIAN_POINT ( 'NONE',  ( 8.778228370994069607, 117.8144977861501701, -0.2251889147252496837 ) ) ;
#26827 = CARTESIAN_POINT ( 'NONE',  ( -10.06125758770563117, 125.9185081520631257, -0.05443999739187975473 ) ) ;
#26828 = DIRECTION ( 'NONE',  ( 0.4849315768086427392, 0.8745520943968311256, 7.999751396575047988E-15 ) ) ;
#26829 = CARTESIAN_POINT ( 'NONE',  ( 22.78320035282265721, 142.4248215231809240, 1.435786487410106727 ) ) ;
#26830 = CARTESIAN_POINT ( 'NONE',  ( 5.305748947172213015, 65.30181249999998272, -5.247078976224250013 ) ) ;
#26831 = CARTESIAN_POINT ( 'NONE',  ( 1.980066450162843106, -15.31690195035381663, 5.269506609478212589 ) ) ;
#26832 = CARTESIAN_POINT ( 'NONE',  ( -18.88959041316451604, 148.1672603684278329, 1.723054188180887847 ) ) ;
#26833 = CARTESIAN_POINT ( 'NONE',  ( -0.2078495401522961472, -3.970246887572310257, -0.9510052327550873041 ) ) ;
#26834 = CARTESIAN_POINT ( 'NONE',  ( -22.39330865153385020, 150.7562895891929031, -1.036336034128335193 ) ) ;
#26835 = CARTESIAN_POINT ( 'NONE',  ( 0.7510871189337386955, -11.68616409646884158, 0.6196617644748384501 ) ) ;
#26836 = B_SPLINE_CURVE_WITH_KNOTS ( 'NONE', 5,
 ( #384, #2735, #28902, #39346, #9523, #18890 ),
 .UNSPECIFIED., .F., .F.,
 ( 6, 6 ),
 ( 0.000000000000000000, 1.000000000000000000 ),
 .UNSPECIFIED. ) ;
#26837 = ORIENTED_EDGE ( 'NONE', *, *, #7319, .F. ) ;
#26838 = CARTESIAN_POINT ( 'NONE',  ( -42.98746435103614516, 21.25571956186866984, 0.9029888148949687388 ) ) ;
#26839 = CARTESIAN_POINT ( 'NONE',  ( 7.643894675291481811, 124.7210964017841377, 0.1527028184316447379 ) ) ;
#26840 = CARTESIAN_POINT ( 'NONE',  ( -5.888833980634905707, 121.2452591720019370, 0.3608419296047723490 ) ) ;
#26841 = CARTESIAN_POINT ( 'NONE',  ( 4.908419482240064191, -12.74103600948764381, 2.406175225133469819 ) ) ;
#26842 = CARTESIAN_POINT ( 'NONE',  ( 17.57956382101102477, 146.6691408387931688, -1.464727724346841953 ) ) ;
#26843 = CARTESIAN_POINT ( 'NONE',  ( -14.48730688186172166, 125.6573275863457866, -2.042335292678053360 ) ) ;
#26844 = CARTESIAN_POINT ( 'NONE',  ( 4.299095875381824250, 115.7036751318245678, 1.546138500147263839 ) ) ;
#26845 = EDGE_CURVE ( 'NONE', #14389, #909, #9035, .T. ) ;
#26846 = CARTESIAN_POINT ( 'NONE',  ( 1.979956398862833922, -15.17398463081316784, 5.317940750273952411 ) ) ;
#26847 = CARTESIAN_POINT ( 'NONE',  ( -4.932839847226206054, 117.4753194895807979, -1.061409891849272036 ) ) ;
#26848 = CARTESIAN_POINT ( 'NONE',  ( 15.81024248929834641, 146.2514283349100594, 0.08545504004084580885 ) ) ;
#26849 = ORIENTED_EDGE ( 'NONE', *, *, #19865, .F. ) ;
#26850 = CARTESIAN_POINT ( 'NONE',  ( -2.918314285971537636, 107.9144754008294029, 4.333296045763540327 ) ) ;
#26851 = CARTESIAN_POINT ( 'NONE',  ( 1.615233038652823305, 106.5840813593882075, 5.022315509531020794 ) ) ;
#26852 = CARTESIAN_POINT ( 'NONE',  ( -17.14499999999999957, 71.11999999999999034, 5.079999999999997407 ) ) ;
#26853 = CARTESIAN_POINT ( 'NONE',  ( -4.721633889153055819, 27.87760190724945275, 0.5093158822365639882 ) ) ;
#26854 = CARTESIAN_POINT ( 'NONE',  ( 22.97142009758390557, 150.1545470440437953, 0.2295619762022475807 ) ) ;
#26855 = CARTESIAN_POINT ( 'NONE',  ( -10.32579803928178031, 77.06797118195436269, -1.523999999999998245 ) ) ;
#26856 = CARTESIAN_POINT ( 'NONE',  ( 1.824049531341678021, -15.68876244400656184, 5.768564601460718144 ) ) ;
#26857 = DIRECTION ( 'NONE',  ( -1.000000000000000000, 9.627370216492862708E-17, 0.000000000000000000 ) ) ;
#26858 = DIRECTION ( 'NONE',  ( -0.9998004120163608288, 0.000000000000000000, -0.01997839162482749342 ) ) ;
#26859 = CARTESIAN_POINT ( 'NONE',  ( 19.36210883413055583, 150.5708382285403388, 2.397539767985719994 ) ) ;
#26860 = ORIENTED_EDGE ( 'NONE', *, *, #38613, .T. ) ;
#26861 = CARTESIAN_POINT ( 'NONE',  ( -5.416678580886389760, 20.69493382693234196, -6.515560366292809213 ) ) ;
#26862 = CARTESIAN_POINT ( 'NONE',  ( -2.347363924070998475, 117.2563622648257962, -0.6826054999005346513 ) ) ;
#26863 = CARTESIAN_POINT ( 'NONE',  ( -1.232226514449051402, 109.2701902778323557, -3.967559291276892885 ) ) ;
#26864 = CARTESIAN_POINT ( 'NONE',  ( -5.230039278750650666, 78.94094791484918971, 5.321858878494039047 ) ) ;
#26865 = CARTESIAN_POINT ( 'NONE',  ( -10.45722248778828423, 56.52709681235293715, -5.016499999999999737 ) ) ;
#26866 = DIRECTION ( 'NONE',  ( 0.7770581983690878491, -0.6294287539883980376, 5.101669463485847584E-16 ) ) ;
#26867 = CARTESIAN_POINT ( 'NONE',  ( -3.812863311134618183, 2.017465188139291765, -2.614655560905410958 ) ) ;
#26868 = CARTESIAN_POINT ( 'NONE',  ( -24.23745918283205114, 82.38670122043342303, -1.524000000000006461 ) ) ;
#26869 = CARTESIAN_POINT ( 'NONE',  ( -5.268467657037344765, 115.6909491485453003, 0.8695824031848999880 ) ) ;
#26870 = CARTESIAN_POINT ( 'NONE',  ( 2.107392885931908211, -15.11054218480166433, 5.236909061670549370 ) ) ;
#26871 = EDGE_CURVE ( 'NONE', #3266, #37307, #15691, .T. ) ;
#26872 = CARTESIAN_POINT ( 'NONE',  ( 3.904686386324433656, 121.5791280715047122, -0.1678698840778539148 ) ) ;
#26873 = CARTESIAN_POINT ( 'NONE',  ( -22.62544200675493400, 150.0155710288180444, 0.5141704484958254939 ) ) ;
#26874 = CARTESIAN_POINT ( 'NONE',  ( 8.798071512540863282, 117.6842349196870572, 0.1758064070670784795 ) ) ;
#26875 = DIRECTION ( 'NONE',  ( -0.8745520943968241312, 0.4849315768086548406, -5.691349986800536046E-16 ) ) ;
#26876 = VERTEX_POINT ( 'NONE', #41034 ) ;
#26877 = CARTESIAN_POINT ( 'NONE',  ( -2.762866373388253471, 104.6144662015512097, -4.566024155138136642 ) ) ;
#26878 = CARTESIAN_POINT ( 'NONE',  ( 4.176612884749554944, -15.71584146423912820, 3.621469129306375656 ) ) ;
#26879 = CARTESIAN_POINT ( 'NONE',  ( -20.20415560162858881, 149.0333503175929479, 1.664251383091793768 ) ) ;
#26880 = CARTESIAN_POINT ( 'NONE',  ( 0.5513313392710353922, 29.23057874652566923, -0.8050760855368327418 ) ) ;
#26881 = ORIENTED_EDGE ( 'NONE', *, *, #40687, .F. ) ;
#26882 = CARTESIAN_POINT ( 'NONE',  ( -23.49500000000000455, 71.11999999999999034, 1.904999999999985372 ) ) ;
#26883 = CARTESIAN_POINT ( 'NONE',  ( 1.969999177844855121, 122.1523088006674840, 0.2733757396980690535 ) ) ;
#26884 = SHAPE_REPRESENTATION_RELATIONSHIP ( 'NONE' , 'NONE' ,  #22056, #41738 ) ;
#26885 = CARTESIAN_POINT ( 'NONE',  ( -4.935370518415244767, 156.1188696671683260, 1.185051001079852284 ) ) ;
#26886 = CARTESIAN_POINT ( 'NONE',  ( 1.912930843383831236, 118.1189424416472207, 0.9466463369225973645 ) ) ;
#26887 = CARTESIAN_POINT ( 'NONE',  ( 0.5200570697820592336, 119.3183582894065893, -0.5597423419424873980 ) ) ;
#26888 = CARTESIAN_POINT ( 'NONE',  ( -1.110739552455700663, 158.5855360310326319, -1.562719372149667274 ) ) ;
#26889 = DIRECTION ( 'NONE',  ( 0.9998004120163608288, 4.016384292689131511E-17, 0.01997839162482749342 ) ) ;
#26890 = CARTESIAN_POINT ( 'NONE',  ( 4.161853366895682527, 118.2393569085959371, -0.2292923879269599674 ) ) ;
#26891 = CARTESIAN_POINT ( 'NONE',  ( 12.05713894362174798, 151.9703418938154584, -0.4396675171196798848 ) ) ;
#26892 = ORIENTED_EDGE ( 'NONE', *, *, #7173, .F. ) ;
#26893 = CARTESIAN_POINT ( 'NONE',  ( 2.598075364112794716, -15.28479904474297513, 4.671545106743766773 ) ) ;
#26894 = CARTESIAN_POINT ( 'NONE',  ( 11.37822013471344995, 56.06794068206381354, -5.016500000000108983 ) ) ;
#26895 = CARTESIAN_POINT ( 'NONE',  ( -56.57399730107074021, 3.557946380840032674, 2.108622681941778154 ) ) ;
#26896 = ADVANCED_FACE ( 'NONE', ( #27817 ), #33393, .T. ) ;
#26897 = CIRCLE ( 'NONE', #32336, 16.60960244842765832 ) ;
#26898 = CARTESIAN_POINT ( 'NONE',  ( 3.900846188197024667, 12.44727460162280863, 2.488979119290085862 ) ) ;
#26899 = CARTESIAN_POINT ( 'NONE',  ( 6.954653016369009677, 155.6889469082406947, 1.616181084571816307 ) ) ;
#26900 = CARTESIAN_POINT ( 'NONE',  ( -2.502258884723083554, 30.19631072378583170, 1.542227018752644119 ) ) ;
#26901 = CARTESIAN_POINT ( 'NONE',  ( -2.755274729907521980, 20.69627551736597226, -3.746277899328600558 ) ) ;
#26902 = CARTESIAN_POINT ( 'NONE',  ( 15.77366026095708129, 146.5725700477668170, 0.4436318658883101618 ) ) ;
#26903 = DIRECTION ( 'NONE',  ( -5.188838149069471174E-16, 1.699382548006136313E-16, 1.000000000000000000 ) ) ;
#26904 = EDGE_CURVE ( 'NONE', #22816, #9488, #8652, .T. ) ;
#26905 = CARTESIAN_POINT ( 'NONE',  ( -50.84949806483947299, 11.71728973011885344, -0.3797569051948266328 ) ) ;
#26906 = CARTESIAN_POINT ( 'NONE',  ( -5.542008918447461241, 116.7834412270213562, -0.4238622777438119105 ) ) ;
#26907 = DIRECTION ( 'NONE',  ( 0.01997839162482749689, 1.040247600000945640E-18, -0.9998004120163610509 ) ) ;
#26908 = LINE ( 'NONE', #7536, #23957 ) ;
#26909 = CARTESIAN_POINT ( 'NONE',  ( -3.831877602099685198, 71.07198261757335445, 1.270000000000005347 ) ) ;
#26910 = CARTESIAN_POINT ( 'NONE',  ( -29.24397885296949440, 65.27318422236065487, -1.524000000000773181 ) ) ;
#26911 = CARTESIAN_POINT ( 'NONE',  ( 5.579263951540290201, 8.940976842658965751, -6.340258638080404019 ) ) ;
#26912 = CARTESIAN_POINT ( 'NONE',  ( -28.42835727709238114, 77.69497285144578314, -1.524000000000007793 ) ) ;
#26913 = CARTESIAN_POINT ( 'NONE',  ( -17.14499999999999957, 71.11999999999999034, 5.016499999999999737 ) ) ;
#26914 = CARTESIAN_POINT ( 'NONE',  ( -57.83255607995954506, 2.614142775670388996, 0.5104628509321454954 ) ) ;
#26915 = CARTESIAN_POINT ( 'NONE',  ( 0.006734421711972093244, 121.9236798544229003, -0.3370180007451226700 ) ) ;
#26916 = CARTESIAN_POINT ( 'NONE',  ( -0.004910662370487326248, 159.5928157220454295, 0.2457496255665023166 ) ) ;
#26917 = ORIENTED_EDGE ( 'NONE', *, *, #7082, .T. ) ;
#26918 = CARTESIAN_POINT ( 'NONE',  ( -58.05887703936295452, 1.806656698574160558, -1.362798277128405289 ) ) ;
#26919 = CARTESIAN_POINT ( 'NONE',  ( -6.969786809622995349, 121.9471538115466700, -0.2197179574160783577 ) ) ;
#26920 = EDGE_CURVE ( 'NONE', #17114, #30952, #25041, .T. ) ;
#26921 =( BOUNDED_CURVE ( )  B_SPLINE_CURVE ( 3, ( #37317, #8134, #21107, #3915 ),
 .UNSPECIFIED., .F., .T. ) 
 B_SPLINE_CURVE_WITH_KNOTS ( ( 4, 4 ),
 ( 1.303225233037621953E-32, 1.570796326794896558 ),
 .UNSPECIFIED. ) 
 CURVE ( )  GEOMETRIC_REPRESENTATION_ITEM ( )  RATIONAL_B_SPLINE_CURVE ( ( 1.000000000000000000, 0.8047378541243649375, 0.8047378541243649375, 1.000000000000000000 ) ) 
 REPRESENTATION_ITEM ( '' )  );
#26922 = EDGE_LOOP ( 'NONE', ( #37369, #39935, #14085, #25146, #37931, #37487, #25896, #5501 ) ) ;
#26923 = CARTESIAN_POINT ( 'NONE',  ( -22.95370498042275642, 82.54569470718179502, 1.269999999999993356 ) ) ;
#26924 = CARTESIAN_POINT ( 'NONE',  ( -6.499560145427196289, 121.7799842514348541, -0.1589113151347878727 ) ) ;
#26925 = CARTESIAN_POINT ( 'NONE',  ( 6.166227012738786151, -13.75546675568918609, 1.699147612634045235 ) ) ;
#26926 = CARTESIAN_POINT ( 'NONE',  ( -12.06131655867255503, 120.6765805525287334, 1.069212010736126039 ) ) ;
#26927 = CARTESIAN_POINT ( 'NONE',  ( -3.957843245660688680, 22.95775517496322848, 2.395914033147342970 ) ) ;
#26928 = CARTESIAN_POINT ( 'NONE',  ( 23.23349130944691154, 142.6711341654318801, 0.9216821775544488116 ) ) ;
#26929 = ADVANCED_FACE ( 'NONE', ( #349 ), #35483, .T. ) ;
#26930 = CARTESIAN_POINT ( 'NONE',  ( 2.202447430380541249, -15.40435026327015322, 5.902591840625516895 ) ) ;
#26931 = CARTESIAN_POINT ( 'NONE',  ( 2.889066315880882030, 25.55657059589919911, 3.609430016826872478 ) ) ;
#26932 = CARTESIAN_POINT ( 'NONE',  ( -0.9739946362265716751, -5.975847910206034896, -0.08934465120823924245 ) ) ;
#26933 = CARTESIAN_POINT ( 'NONE',  ( -11.65197432296793068, 118.7334002725740874, -0.4428703322330640457 ) ) ;
#26934 = DIRECTION ( 'NONE',  ( -0.9998004120163610509, -5.205824365704083805E-17, -0.01997839162482749689 ) ) ;
#26935 = DIRECTION ( 'NONE',  ( 5.188838149069472160E-16, -1.699382548006136559E-16, -1.000000000000000000 ) ) ;
#26936 = AXIS2_PLACEMENT_3D ( 'NONE', #38090, #34065, #37248 ) ;
#26937 = CARTESIAN_POINT ( 'NONE',  ( 2.248466038385836807, 116.3129351467598127, 0.2264917513733100685 ) ) ;
#26938 = CARTESIAN_POINT ( 'NONE',  ( -5.873949295438763762, 120.1673030736515955, 0.8402073876045392797 ) ) ;
#26939 = CARTESIAN_POINT ( 'NONE',  ( -57.62437015934663265, 1.316655653385057079, -1.280333191779400082 ) ) ;
#26940 = CARTESIAN_POINT ( 'NONE',  ( -0.02768730785358111679, 158.9256195073445213, 1.385586103196075891 ) ) ;
#26941 = CARTESIAN_POINT ( 'NONE',  ( 19.22350799450994430, 148.9694856701144090, -1.735702374547824167 ) ) ;
#26942 = CARTESIAN_POINT ( 'NONE',  ( -0.9685753864191435358, -11.31243604255521085, 0.1179740209226832204 ) ) ;
#26943 = CARTESIAN_POINT ( 'NONE',  ( -19.06843068773027383, 131.8899703912256314, -2.039348754248471174 ) ) ;
#26944 = CARTESIAN_POINT ( 'NONE',  ( -46.52557095416602806, 23.25943309041075224, -3.047882326417284293 ) ) ;
#26945 = CARTESIAN_POINT ( 'NONE',  ( 3.897805094127884118, 104.6144662015456674, 2.864625571244531876 ) ) ;
#26946 = CARTESIAN_POINT ( 'NONE',  ( 10.66674206690810500, 124.7671305375842934, -0.7411263988551108906 ) ) ;
#26947 = EDGE_CURVE ( 'NONE', #28739, #22885, #4854, .T. ) ;
#26948 = CARTESIAN_POINT ( 'NONE',  ( -7.783246152616193569, 154.6561476914895081, -0.1555277812256514736 ) ) ;
#26949 = VERTEX_POINT ( 'NONE', #12686 ) ;
#26950 = CARTESIAN_POINT ( 'NONE',  ( -7.646026353518148966, 156.1362479297160348, -1.963328325631339411 ) ) ;
#26951 = CARTESIAN_POINT ( 'NONE',  ( 4.270102617218862306, -15.70017440876955739, 3.434341872514240723 ) ) ;
#26952 = CARTESIAN_POINT ( 'NONE',  ( -11.56352105402813280, 78.55269139521317356, -1.523999999999999133 ) ) ;
#26953 = CARTESIAN_POINT ( 'NONE',  ( -4.554733065532879266, 118.0858692952890863, -0.7374014039634101403 ) ) ;
#26954 = CARTESIAN_POINT ( 'NONE',  ( -54.77668461537430034, 8.146287316968315650, -3.518595155146543529 ) ) ;
#26955 = CARTESIAN_POINT ( 'NONE',  ( 4.065926199369043204, 118.2429491485453354, 0.3080910687088499467 ) ) ;
#26956 = B_SPLINE_SURFACE_WITH_KNOTS ( 'NONE', 3, 3, ( 
 ( #1360, #36713, #11550, #1151, #24332, #17520, #14318, #27330, #4775, #7953, #30727, #1576, #37337, #4980, #17937, #30940, #24533, #2832, #16000, #34779, #31787, #9003, #9214, #19201, #37969, #21970, #24755, #15585, #2626, #32209, #34571, #35000, #28800, #38605 ),
 ( #5820, #12408, #28590, #15161, #28382, #18776, #35403, #41598, #35202, #41172, #28167, #8578, #21752, #37754, #31994, #22377, #25400, #38186, #11976, #38402, #22171, #9411, #18569, #40960, #15792, #3042, #6028, #21542, #5398, #6230, #18990, #24970, #8794, #41388 ),
 ( #5613, #11766, #41814, #12193, #18354, #31360, #12610, #25597, #2203, #31576, #2416, #15376, #25186, #3457, #36460, #29209, #3245, #26649, #6434, #12812, #39228, #19822, #10038, #478, #16634, #16204, #16419, #23010, #23431, #6647, #20241, #4096, #19408, #7071 ),
 ( #52, #9620, #7279, #13451, #13659, #20035, #13018, #3669, #32415, #35620, #32624, #33054, #28999, #3884, #33267, #9829, #16849, #687, #42016, #25802, #26439, #36038, #38808, #29641, #35831, #29425, #39021, #266, #39443, #19611, #10461, #26012, #6853, #36250 ),
 ( #22796, #13240, #10246, #26224, #32839, #23217, #22588, #29849, #39657, #36884, #27074, #30472, #14691, #10667, #1527, #39871, #27283, #23865, #1733, #1316, #20663, #30892, #895, #11500, #37491, #14273, #37287, #26863, #27696, #21080, #7702, #30262, #4513, #40704 ),
 ( #34105, #24486, #8314, #21286, #30679, #40297, #23648, #4726, #33689, #17474, #40082, #11090, #17678, #24077, #34315, #33478, #37089, #24282, #17055, #7907, #36670, #27495, #20871, #7491, #14483, #30057, #33895, #13869, #40503, #11298, #20451, #8106, #4308, #4932 ),
 ( #17890, #17271, #1103, #14070, #10877, #18937, #31101, #41757, #25547, #18512, #25342, #14899, #31945, #31518, #8739, #11714, #2362, #38550, #27901, #12139, #1940, #5974, #24701, #5769, #41120, #40909, #28539, #15739, #21490, #38133, #15321, #11926, #37915, #5555 ),
 ( #21700, #34522, #28328, #5348, #41336, #2148, #2783, #35149, #25131, #37707, #9363, #38345, #28744, #8948, #9163, #12558, #18302, #8530, #34724, #22326, #31303, #15107, #5144, #28110, #24918, #21915, #34945, #18723, #31733, #2576, #15537, #41546, #12354, #18098 ),
 ( #22120, #6800, #16150, #3835, #32153, #6384, #15948, #13610, #19768, #19989, #13398, #22539, #9984, #38758, #19354, #29801, #28945, #32360, #35775, #32789, #39607, #33007, #16584, #3400, #10410, #41962, #3188, #1, #3619, #9568, #29154, #29593, #35351, #35566 ),
 ( #25960, #6179, #26172, #7021, #427, #16367, #22957, #26386, #39393, #36200, #39177, #2986, #12966, #6590, #38967, #12761, #25750, #32567, #35985, #10195, #23165, #9777, #22744, #19558, #29373, #212, #16799, #641, #13187, #26600, #19148, #14225, #20607, #21033 ),
 ( #27232, #33639, #30215, #14019, #23810, #26816, #4046, #27026, #39824, #4466, #23600, #36831, #20399, #34055, #11245, #7651, #17006, #1686, #1474, #24230, #17423, #14431, #37240, #36621, #30005, #40034, #30837, #7441, #10618, #4884, #845, #7233, #30421, #40246 ),
 ( #11040, #33427, #10829, #1268, #17839, #1055, #14640, #40654, #13817, #27439, #7858, #24023, #40455, #37040, #4256, #27641, #17218, #20819, #23382, #20193, #33845, #8058, #4673, #17631, #30631, #36415, #33218, #37658, #34675, #34890, #2095, #2525, #8482, #12088 ) ),
 .UNSPECIFIED., .F., .F., .F.,
 ( 4, 1, 1, 1, 1, 1, 3, 4 ),
 ( 4, 1, 1, 1, 1, 1, 1, 1, 1, 1, 1, 1, 1, 1, 1, 1, 1, 1, 1, 2, 1, 1, 1, 1, 1, 1, 1, 1, 1, 1, 4 ),
 ( 0.000000000000000000, 0.1666666666666666574, 0.2500000000000000000, 0.5000000000000000000, 0.5555555555555555802, 0.7500000000000000000, 1.000000000000000000, 1.010000000000000009 ),
 ( 0.000000000000000000, 0.02126250000000000015, 0.04252500000000000030, 0.06378749999999999698, 0.08505000000000000060, 0.1063125000000000042, 0.1275749999999999940, 0.1488374999999999837, 0.1701000000000000012, 0.1913624999999999909, 0.2126250000000000084, 0.2338874999999999704, 0.2551500000000000434, 0.2764124999999999499, 0.2870437499999999864, 0.2976749999999999674, 0.3083062500000000039, 0.3189375000000000404, 0.3295687499999999659, 0.3402000000000000024, 0.4226750000000000229, 0.5051499999999999879, 0.5876249999999998419, 0.6700999999999999179, 0.7525749999999999940, 0.7938125000000000320, 0.8350499999999999590, 0.8762874999999994419, 0.9175249999999994799, 0.9587624999999999620, 1.000000000000000000 ),
 .UNSPECIFIED. ) ;
#26957 = CARTESIAN_POINT ( 'NONE',  ( 14.87841870982556358, 131.2528086460777388, 2.073644862699850933 ) ) ;
#26958 = DIRECTION ( 'NONE',  ( -0.01997839162482793057, 0.000000000000000000, 0.9998004120163608288 ) ) ;
#26959 = CARTESIAN_POINT ( 'NONE',  ( 11.73725613052199535, 118.7267541726749869, 0.2187512536375166017 ) ) ;
#26960 = AXIS2_PLACEMENT_3D ( 'NONE', #3411, #15751, #35578 ) ;
#26961 = CARTESIAN_POINT ( 'NONE',  ( 5.158690622980511620, 18.63085216599767691, -6.696816702733363158 ) ) ;
#26962 = CARTESIAN_POINT ( 'NONE',  ( 9.269771126213358414, 123.9149913687586064, 0.6034020272129928530 ) ) ;
#26963 = EDGE_CURVE ( 'NONE', #15388, #41065, #2813, .T. ) ;
#26964 = EDGE_CURVE ( 'NONE', #32861, #4233, #19099, .T. ) ;
#26965 = AXIS2_PLACEMENT_3D ( 'NONE', #25444, #35879, #28844 ) ;
#26966 = CARTESIAN_POINT ( 'NONE',  ( 15.27126642897840192, 121.5932973536894934, -0.6323128539531662762 ) ) ;
#26967 = AXIS2_PLACEMENT_3D ( 'NONE', #11706, #18504, #37083 ) ;
#26968 = CARTESIAN_POINT ( 'NONE',  ( -4.808149584360944750, 105.1224662015457483, 0.4147572885131461939 ) ) ;
#26969 = DIRECTION ( 'NONE',  ( -0.1728608224830406603, -1.098208118798718614E-16, 0.9849462604886047856 ) ) ;
#26970 = CARTESIAN_POINT ( 'NONE',  ( -10.82496502431745000, 157.9086237439880733, -0.1564342443379707071 ) ) ;
#26971 = ORIENTED_EDGE ( 'NONE', *, *, #12305, .T. ) ;
#26972 = CARTESIAN_POINT ( 'NONE',  ( -47.07934102874911986, 22.98505637820354153, -3.579966862081940260 ) ) ;
#26973 = CARTESIAN_POINT ( 'NONE',  ( 8.002845466965794685, 121.6569013250319387, -0.7958636649122211582 ) ) ;
#26974 = CARTESIAN_POINT ( 'NONE',  ( -8.778228370994318297, 117.8144977861501701, 0.2251889147251710244 ) ) ;
#26975 = VERTEX_POINT ( 'NONE', #15657 ) ;
#26976 = CARTESIAN_POINT ( 'NONE',  ( -4.826173324110722973, 117.7976308133446821, -0.9239831869685056764 ) ) ;
#26977 = CARTESIAN_POINT ( 'NONE',  ( -2.942445288855481511, 156.0884104482065595, -0.3607664148606968268 ) ) ;
#26978 = CARTESIAN_POINT ( 'NONE',  ( 4.564001774108119136, -12.95384785397724059, 2.770574723176509657 ) ) ;
#26979 = CARTESIAN_POINT ( 'NONE',  ( -21.63845757858517871, 150.4657531037631486, 1.001545151475624174 ) ) ;
#26980 = CARTESIAN_POINT ( 'NONE',  ( -41.08171237912078055, 23.06270199366201368, 1.270028482464937936 ) ) ;
#26981 = CARTESIAN_POINT ( 'NONE',  ( 5.786284826928784319, 116.9447284183608389, 0.1988161383433787732 ) ) ;
#26982 = EDGE_CURVE ( 'NONE', #5344, #38115, #35698, .T. ) ;
#26983 = ORIENTED_EDGE ( 'NONE', *, *, #32173, .F. ) ;
#26984 = CARTESIAN_POINT ( 'NONE',  ( -3.832284926465886254, -5.753926550059754064, 2.584458424559757272 ) ) ;
#26985 = CARTESIAN_POINT ( 'NONE',  ( -22.83504831576704674, 150.4065277667444036, -0.4818782557684027079 ) ) ;
#26986 = CARTESIAN_POINT ( 'NONE',  ( -7.772068811996249771, 69.25462295839062676, 1.270000000000003570 ) ) ;
#26987 = FACE_OUTER_BOUND ( 'NONE', #15532, .T. ) ;
#26988 = VERTEX_POINT ( 'NONE', #26094 ) ;
#26989 = CARTESIAN_POINT ( 'NONE',  ( 4.368446179951305020, 118.5872638624673243, 1.043865840824246716 ) ) ;
#26990 = CARTESIAN_POINT ( 'NONE',  ( -2.168033660621066172, 0.5777166996233511487, 4.103230905123370853 ) ) ;
#26991 = CARTESIAN_POINT ( 'NONE',  ( 9.442718531279737704, 118.5748184150550060, 1.042386753229705088 ) ) ;
#26992 = CARTESIAN_POINT ( 'NONE',  ( -50.51080154061983052, 15.37413104944036668, -4.759117110719017774 ) ) ;
#26994 = CARTESIAN_POINT ( 'NONE',  ( 20.91036014055495684, 148.6614476615901594, -1.563091210272363085 ) ) ;
#26993 = CARTESIAN_POINT ( 'NONE',  ( -6.616924617768071466E-14, 97.37546620154573418, 7.965525879364083286E-30 ) ) ;
#26995 = CARTESIAN_POINT ( 'NONE',  ( 1.294644163514462987, -7.843371450943685375, 4.453423563430108700 ) ) ;
#26996 = CARTESIAN_POINT ( 'NONE',  ( -15.11776246977262694, 121.4505734225448066, -1.235019191190165344 ) ) ;
#26997 = ORIENTED_EDGE ( 'NONE', *, *, #13171, .T. ) ;
#26998 = TOROIDAL_SURFACE ( 'NONE', #10657, 0.3810000000000014486, 0.2540000000000000036 ) ;
#26999 = CARTESIAN_POINT ( 'NONE',  ( -8.581106358026319825, 123.3373102669514765, -0.01935445114830152899 ) ) ;
#27000 = CARTESIAN_POINT ( 'NONE',  ( 6.419191409189793696, -13.32337952207179832, 0.5587850172365541601 ) ) ;
#27001 = CARTESIAN_POINT ( 'NONE',  ( -42.48565245465179885, 21.90714463913253240, 1.692305106577786322 ) ) ;
#27002 = DIRECTION ( 'NONE',  ( -1.000000000000000000, 9.627370216492862708E-17, 0.000000000000000000 ) ) ;
#27003 = VERTEX_POINT ( 'NONE', #6937 ) ;
#27004 = CARTESIAN_POINT ( 'NONE',  ( 10.72551448100089111, 121.7859837122882283, 1.665033671525604442 ) ) ;
#27005 = CARTESIAN_POINT ( 'NONE',  ( -26.01970228765382132, 72.88622078690372064, -1.524000000000005794 ) ) ;
#27006 = CARTESIAN_POINT ( 'NONE',  ( -14.39766717389552220, 60.02151067229126369, 1.905000000000008686 ) ) ;
#27007 = CIRCLE ( 'NONE', #3888, 6.349999999999999645 ) ;
#27008 = AXIS2_PLACEMENT_3D ( 'NONE', #18641, #22040, #3316 ) ;
#27009 = CARTESIAN_POINT ( 'NONE',  ( -3.922549711534387917, 117.3164332630744298, 0.5226386447273276836 ) ) ;
#27010 = CARTESIAN_POINT ( 'NONE',  ( -2.144872632962109726, 6.596990873201863614, -8.179991544870226505 ) ) ;
#27011 = CARTESIAN_POINT ( 'NONE',  ( 16.44150122627317856, 146.0252812507985141, 1.609049209688531157 ) ) ;
#27012 = DIRECTION ( 'NONE',  ( -1.000000000000000000, 0.000000000000000000, 0.000000000000000000 ) ) ;
#27013 = CARTESIAN_POINT ( 'NONE',  ( 23.09108451844687693, 149.2510847660714148, -0.2673146292145802128 ) ) ;
#27014 = DIRECTION ( 'NONE',  ( -0.8745520943968243532, 0.4849315768086547296, -5.361993529360573944E-16 ) ) ;
#27015 = VECTOR ( 'NONE', #4407, 1000.000000000000227 ) ;
#27016 = CARTESIAN_POINT ( 'NONE',  ( -57.43646543250576997, 1.720973480456895910, 1.454608885177623767 ) ) ;
#27017 = CARTESIAN_POINT ( 'NONE',  ( -48.00704091872448487, 20.04541143072568232, 5.176114466449816653 ) ) ;
#27018 = CARTESIAN_POINT ( 'NONE',  ( -49.39021242113546606, 17.77731941784099234, 5.290631085210035778 ) ) ;
#27019 = CARTESIAN_POINT ( 'NONE',  ( -58.55448969609990684, -0.1373465052187913260, 0.5737898672011175760 ) ) ;
#27020 = CARTESIAN_POINT ( 'NONE',  ( -4.537165138249189766, 118.1142604855938316, 0.5194510162086110050 ) ) ;
#27021 = CARTESIAN_POINT ( 'NONE',  ( 0.6790819876102632824, 105.9272292791364265, -5.296718569794414577 ) ) ;
#27022 = VECTOR ( 'NONE', #30730, 1000.000000000000000 ) ;
#27023 = VERTEX_POINT ( 'NONE', #38471 ) ;
#27024 = CARTESIAN_POINT ( 'NONE',  ( -47.04837031381860157, 23.61299024743492581, 3.054033755318061871 ) ) ;
#27025 = CARTESIAN_POINT ( 'NONE',  ( 8.350555576214318876, 119.9924706458420758, -1.116089668697638260 ) ) ;
#27026 = CARTESIAN_POINT ( 'NONE',  ( -6.711594774621165271, 121.2247800624193133, -0.3423702293131483665 ) ) ;
#27027 = CARTESIAN_POINT ( 'NONE',  ( 4.543433710119733071, 118.0881514374072196, 0.7498910874544754135 ) ) ;
#27028 = CARTESIAN_POINT ( 'NONE',  ( -16.00153516066852077, 147.3640369757652877, -1.286050259728349410 ) ) ;
#27029 = FACE_OUTER_BOUND ( 'NONE', #24179, .T. ) ;
#27030 = CARTESIAN_POINT ( 'NONE',  ( 0.7141878136923727194, 118.1651004746852749, -0.8604252410570366605 ) ) ;
#27031 = CARTESIAN_POINT ( 'NONE',  ( 7.639359131133803160, 124.2918010433613745, 0.1437932647211237758 ) ) ;
#27032 = CARTESIAN_POINT ( 'NONE',  ( -14.47722597845739223, 150.4300676932417389, -1.698653275673423835 ) ) ;
#27033 = DIRECTION ( 'NONE',  ( 5.188838149069472160E-16, -1.699382548006136559E-16, -1.000000000000000000 ) ) ;
#27034 = CARTESIAN_POINT ( 'NONE',  ( -47.22690022493003426, 20.09066223305351784, 5.151063612125013513 ) ) ;
#27035 = CARTESIAN_POINT ( 'NONE',  ( 8.019189887688648710, 121.5801876769127006, -0.8265596201061345960 ) ) ;
#27036 = CARTESIAN_POINT ( 'NONE',  ( 7.002510706568009446, 121.9568449752713661, 0.1399268290605550913 ) ) ;
#27037 = DIRECTION ( 'NONE',  ( -0.01731298258488772612, 0.9998501190848633202, -1.788962107505314604E-16 ) ) ;
#27038 = CARTESIAN_POINT ( 'NONE',  ( 14.81745968805112312, 156.1223461918646933, 1.150419650929870752 ) ) ;
#27039 = CARTESIAN_POINT ( 'NONE',  ( 5.871452009091314039, 53.58606249999999704, -5.016499999999999737 ) ) ;
#27040 = CARTESIAN_POINT ( 'NONE',  ( 2.778183380295619287, -15.08691762314898277, 4.378844564414270835 ) ) ;
#27041 = CARTESIAN_POINT ( 'NONE',  ( -18.72287149482797730, 147.1333978507680627, 1.701234099286256463 ) ) ;
#27042 = CARTESIAN_POINT ( 'NONE',  ( -0.9497947497622778457, -2.244019015280241280, -0.2169513509177584398 ) ) ;
#27043 = CARTESIAN_POINT ( 'NONE',  ( -0.3250403508453759693, 116.7787044104018861, -0.2632219653755002997 ) ) ;
#27044 = AXIS2_PLACEMENT_3D ( 'NONE', #41196, #5845, #38424 ) ;
#27045 = CARTESIAN_POINT ( 'NONE',  ( -0.9222101193809760789, -5.324732007522724686, 0.3213417913276819249 ) ) ;
#27046 = ORIENTED_EDGE ( 'NONE', *, *, #15398, .F. ) ;
#27047 = CARTESIAN_POINT ( 'NONE',  ( -48.19617591663109835, 18.61566378669634503, 4.750300018642145794 ) ) ;
#27048 = CARTESIAN_POINT ( 'NONE',  ( 4.381926848743999514, 111.2539628214143903, 3.135495374750700837 ) ) ;
#27049 = PRODUCT_CONTEXT ( 'NONE', #28694, 'mechanical' ) ;
#27050 = CARTESIAN_POINT ( 'NONE',  ( -16.08724493259849453, 146.0544122543811341, 0.5338004346038370818 ) ) ;
#27051 = CARTESIAN_POINT ( 'NONE',  ( 4.778187575955942457, -13.11831155531867310, 3.026993680286476973 ) ) ;
#27052 = CARTESIAN_POINT ( 'NONE',  ( 3.455858276899827608, 119.9243055703230851, -0.6230356542855078894 ) ) ;
#27053 = VERTEX_POINT ( 'NONE', #15869 ) ;
#27054 = CARTESIAN_POINT ( 'NONE',  ( -12.48017577322021232, 122.5542284311838870, -1.820249166172293265 ) ) ;
#27055 = CARTESIAN_POINT ( 'NONE',  ( 4.372915526211548887, 104.6144662015457527, 2.049786579368134021 ) ) ;
#27056 = CARTESIAN_POINT ( 'NONE',  ( 2.234143439902941175, -15.10063862499563747, 5.099642030148213934 ) ) ;
#27057 = CARTESIAN_POINT ( 'NONE',  ( -4.755622421505391273, 117.4716786420896284, -1.195466823065375994 ) ) ;
#27058 = CARTESIAN_POINT ( 'NONE',  ( 15.66469409602187746, 147.2250547476223801, 0.08357164438767009096 ) ) ;
#27059 = VECTOR ( 'NONE', #277, 1000.000000000000114 ) ;
#27060 = ORIENTED_EDGE ( 'NONE', *, *, #644, .T. ) ;
#27061 = DIRECTION ( 'NONE',  ( -1.000000000000000000, 0.000000000000000000, 0.000000000000000000 ) ) ;
#27062 = CARTESIAN_POINT ( 'NONE',  ( 3.799804381934697606, 109.6290786634575483, 3.753174195237087840 ) ) ;
#27063 = DIRECTION ( 'NONE',  ( 4.017660918040594346E-17, -1.000000000000000000, -2.376309959284834438E-19 ) ) ;
#27064 = CARTESIAN_POINT ( 'NONE',  ( -6.540217103314379345E-14, 82.64346620154573486, 2.383338306179204368E-29 ) ) ;
#27065 = CARTESIAN_POINT ( 'NONE',  ( 18.64921795038422658, 125.2334963081946313, 0.1144521110716927581 ) ) ;
#27066 = CARTESIAN_POINT ( 'NONE',  ( -30.75918919842648336, 69.77432548395512413, 1.523999999999991806 ) ) ;
#27067 = CARTESIAN_POINT ( 'NONE',  ( 2.109569702550104786, -15.45397857566253919, 5.961763561042187298 ) ) ;
#27068 = CARTESIAN_POINT ( 'NONE',  ( 1.589478822742971683E-15, 16.51000000000000156, 0.000000000000000000 ) ) ;
#27069 = CARTESIAN_POINT ( 'NONE',  ( -3.212145564005312259, 31.43389969159332509, 0.5456719981668799457 ) ) ;
#27070 = CARTESIAN_POINT ( 'NONE',  ( -0.03067001211942077879, 158.6015251912307633, 1.534852821454057992 ) ) ;
#27071 = EDGE_LOOP ( 'NONE', ( #41418, #15883, #2101, #33039 ) ) ;
#27072 = CARTESIAN_POINT ( 'NONE',  ( -0.9765287272027848298, 24.25689591457997452, 8.364652468500624494 ) ) ;
#27073 = CARTESIAN_POINT ( 'NONE',  ( 8.671363884827380630, 118.3858182005267707, -0.6829674701833058359 ) ) ;
#27074 = CARTESIAN_POINT ( 'NONE',  ( -2.642867612521379250, 121.0686911241271702, -0.3905210903889252405 ) ) ;
#27075 = CARTESIAN_POINT ( 'NONE',  ( 4.756814328053569518, 117.4032681585788396, 1.206529665642613658 ) ) ;
#27076 = CARTESIAN_POINT ( 'NONE',  ( -2.274862078065374771, 107.2457239391372354, -4.729709913239623198 ) ) ;
#27077 = CARTESIAN_POINT ( 'NONE',  ( -0.002462548248923642717, 123.7646714092002611, 0.1232359841711014870 ) ) ;
#27078 = CARTESIAN_POINT ( 'NONE',  ( -2.948169924849943335, 1.592661447142720732, -3.562413953034572867 ) ) ;
#27079 = DIRECTION ( 'NONE',  ( -5.188838149069472160E-16, 1.699382548006136559E-16, 1.000000000000000000 ) ) ;
#27080 = CARTESIAN_POINT ( 'NONE',  ( -4.831828830118795715, 118.5264896598256854, 0.7503674394378322399 ) ) ;
#27081 = CARTESIAN_POINT ( 'NONE',  ( 3.001448597307602828, -14.49079452896849496, 4.301892286087903194 ) ) ;
#27082 = CARTESIAN_POINT ( 'NONE',  ( 0.1065646865914871844, 105.8844662015457061, -5.332932678536314697 ) ) ;
#27083 = CARTESIAN_POINT ( 'NONE',  ( -22.97084167624232975, 148.6798292920915117, 0.5140709287734972488 ) ) ;
#27084 = CARTESIAN_POINT ( 'NONE',  ( -2.993548618139343809, 30.66372051476451688, 4.100031124125591120 ) ) ;
#27085 = CARTESIAN_POINT ( 'NONE',  ( -14.38915334913366983, 80.27078028363496287, 1.523999999999998467 ) ) ;
#27086 = ORIENTED_EDGE ( 'NONE', *, *, #26671, .F. ) ;
#27087 = DIRECTION ( 'NONE',  ( 5.188838149069472160E-16, -1.699382548006136559E-16, -1.000000000000000000 ) ) ;
#27088 = CARTESIAN_POINT ( 'NONE',  ( 4.902411944313367798, -15.42400938342815309, 0.6670879667284028702 ) ) ;
#27089 = CARTESIAN_POINT ( 'NONE',  ( -5.018689047519398372, 118.8869175073591578, 0.8997529482361045217 ) ) ;
#27090 = CARTESIAN_POINT ( 'NONE',  ( -3.832284926465886254, -5.753926550059754064, 2.584458424559757272 ) ) ;
#27091 = VERTEX_POINT ( 'NONE', #28875 ) ;
#27092 = DIRECTION ( 'NONE',  ( -0.4849315768086535083, -0.8745520943968250194, -1.030032898892975065E-16 ) ) ;
#27093 = CARTESIAN_POINT ( 'NONE',  ( 0.6699575554300896130, 116.0160817474902331, 1.654834682733560713 ) ) ;
#27094 = CARTESIAN_POINT ( 'NONE',  ( -10.60975745311351481, 123.7931190674884050, 0.9249770984159895182 ) ) ;
#27095 = CARTESIAN_POINT ( 'NONE',  ( -4.807616723150741400, 117.4049522327240709, -1.198082295914128403 ) ) ;
#27096 = CARTESIAN_POINT ( 'NONE',  ( 7.897101653775039587, 156.2605297791399437, -1.696642280025655536 ) ) ;
#27097 = CARTESIAN_POINT ( 'NONE',  ( -1.154696340448394309, 118.0995038195805904, -0.6495305470935904824 ) ) ;
#27098 = CYLINDRICAL_SURFACE ( 'NONE', #22691, 0.6350000000000014522 ) ;
#27099 = MECHANICAL_DESIGN_GEOMETRIC_PRESENTATION_REPRESENTATION (  '', ( #6014 ), #30463 ) ;
#27100 = CARTESIAN_POINT ( 'NONE',  ( 4.159944195614486695, 118.2392574709719497, -0.2314631920685276401 ) ) ;
#27101 = CARTESIAN_POINT ( 'NONE',  ( 0.008148072696519268604, 156.3406798448389168, -0.4077628766201953359 ) ) ;
#27102 = ORIENTED_EDGE ( 'NONE', *, *, #37125, .T. ) ;
#27103 = CARTESIAN_POINT ( 'NONE',  ( 3.134532381368876575, -15.16579696257060128, 3.749817985361381112 ) ) ;
#27104 = CARTESIAN_POINT ( 'NONE',  ( -5.003023251195230614, 117.4023580318003184, 0.8028984813139020682 ) ) ;
#27105 = CARTESIAN_POINT ( 'NONE',  ( -3.682264917456324671, 104.1064662015457287, -0.07358041635423968885 ) ) ;
#27106 = CARTESIAN_POINT ( 'NONE',  ( 4.064497669612420871, 2.951628549105334898, 2.233594334442648766 ) ) ;
#27107 = CARTESIAN_POINT ( 'NONE',  ( 16.66101725429939506, 148.5304741467402323, 2.032660103712368382 ) ) ;
#27108 = CARTESIAN_POINT ( 'NONE',  ( 1.657835265779881828, 35.17127109692723508, 1.237340896742229690 ) ) ;
#27109 = CARTESIAN_POINT ( 'NONE',  ( -6.479951895127766370, 122.5560431351108974, -0.01853871597398567064 ) ) ;
#27110 = CIRCLE ( 'NONE', #14180, 8.794749999999993406 ) ;
#27111 = CARTESIAN_POINT ( 'NONE',  ( 1.325333094648095011, 19.28447512809159292, -4.440015753949128730 ) ) ;
#27112 = CARTESIAN_POINT ( 'NONE',  ( 4.590565121197709431, 121.2030596905490540, 0.1190299148670779517 ) ) ;
#27113 = CARTESIAN_POINT ( 'NONE',  ( 3.682264917456191888, 97.88346620154572975, 0.07358041635424013294 ) ) ;
#27114 = CARTESIAN_POINT ( 'NONE',  ( -55.03835892454119261, 5.996057868307938854, -1.012875379724342828 ) ) ;
#27115 = CARTESIAN_POINT ( 'NONE',  ( -2.176638237496801409, 116.2240395599583564, -0.1684747500132947051 ) ) ;
#27116 = DIRECTION ( 'NONE',  ( 5.188838149069472160E-16, -1.699382548006136559E-16, -1.000000000000000000 ) ) ;
#27117 = CARTESIAN_POINT ( 'NONE',  ( -46.86449850479133517, 25.52520254179917103, -1.615770181641761560 ) ) ;
#27118 = DIRECTION ( 'NONE',  ( -0.01876124593811915112, -0.9998239923360757730, 0.000000000000000000 ) ) ;
#27119 = CARTESIAN_POINT ( 'NONE',  ( -30.03903471050079688, 57.95649848187943576, -1.269999999999909424 ) ) ;
#27120 = CARTESIAN_POINT ( 'NONE',  ( -8.432237393326710517, 2.893158626077577900, 0.2611430682616783239 ) ) ;
#27121 = CARTESIAN_POINT ( 'NONE',  ( -5.224225368397744873, 56.51499999999979451, 5.327462281792842091 ) ) ;
#27122 = DIRECTION ( 'NONE',  ( -0.9998004120163608288, -5.205824365704081956E-17, -0.01997839162482748995 ) ) ;
#27123 = CARTESIAN_POINT ( 'NONE',  ( -58.82374062945601167, -0.06097470622967726683, 0.2234658159561953850 ) ) ;
#27124 = EDGE_CURVE ( 'NONE', #21375, #20566, #13057, .T. ) ;
#27125 = CARTESIAN_POINT ( 'NONE',  ( 0.05238710761679706701, 113.0327356262574341, -2.621665085262908423 ) ) ;
#27126 = CARTESIAN_POINT ( 'NONE',  ( -23.28378132671084089, 148.8247458934765461, -0.01018146431420857180 ) ) ;
#27127 = VERTEX_POINT ( 'NONE', #27769 ) ;
#27128 = CARTESIAN_POINT ( 'NONE',  ( -58.03112897257378933, 1.932186039288422030, -1.137512825365928348 ) ) ;
#27129 = DIRECTION ( 'NONE',  ( 5.188838149069472160E-16, -1.699382548006136559E-16, -1.000000000000000000 ) ) ;
#27130 = CIRCLE ( 'NONE', #3342, 13.46199999999999619 ) ;
#27131 = VERTEX_POINT ( 'NONE', #21778 ) ;
#27132 = CARTESIAN_POINT ( 'NONE',  ( -47.73297240351458015, 19.53746995444953072, -5.217258361096882346 ) ) ;
#27133 = CARTESIAN_POINT ( 'NONE',  ( -9.006184665392849453, 123.9742709865185191, -0.2138692079817591241 ) ) ;
#27134 = CARTESIAN_POINT ( 'NONE',  ( 3.844517683078125803, -15.15487594273597161, 5.256808347261554104 ) ) ;
#27135 = CARTESIAN_POINT ( 'NONE',  ( -16.12297089460582100, 125.3625853296581312, 1.240993850804037013 ) ) ;
#27136 = CARTESIAN_POINT ( 'NONE',  ( 23.02941925350872410, 142.5499849734818838, 1.196609915892170584 ) ) ;
#27137 = CARTESIAN_POINT ( 'NONE',  ( 15.19088230065812617, 143.3954212834698865, 0.5062221952166892081 ) ) ;
#27138 = CARTESIAN_POINT ( 'NONE',  ( 4.300553167417687561, 27.50566818391071422, -1.719522505244270860 ) ) ;
#27139 = CARTESIAN_POINT ( 'NONE',  ( 0.9581433470387596962, -10.92824219907890360, 0.1848338584972420151 ) ) ;
#27140 = CARTESIAN_POINT ( 'NONE',  ( -22.62002883431073741, 150.6357905964555925, -0.7802727354960531381 ) ) ;
#27141 = CARTESIAN_POINT ( 'NONE',  ( -52.46933349272310920, 12.09275889387806480, -4.271936536825034381 ) ) ;
#27142 = EDGE_CURVE ( 'NONE', #32704, #37473, #36136, .T. ) ;
#27143 = CARTESIAN_POINT ( 'NONE',  ( 4.862200918029492058, 117.4104105557795634, 1.165822508186273865 ) ) ;
#27144 = EDGE_LOOP ( 'NONE', ( #37891, #16953 ) ) ;
#27145 = CARTESIAN_POINT ( 'NONE',  ( -8.789204892644862710, 117.7553426919097745, 0.1101893534113697198 ) ) ;
#27146 = CARTESIAN_POINT ( 'NONE',  ( -0.5348915910374654192, 119.5442839488369628, 0.5285302399602643808 ) ) ;
#27147 = CARTESIAN_POINT ( 'NONE',  ( -58.20240292368494295, 0.06644746378797894426, -0.5499427731179303835 ) ) ;
#27148 = CARTESIAN_POINT ( 'NONE',  ( 19.59580906854006699, 147.4874203640471535, -1.738765900131762576 ) ) ;
#27149 = CARTESIAN_POINT ( 'NONE',  ( 0.9235644399502331847, -7.204839741120207641, 0.3177745608231433705 ) ) ;
#27150 = CARTESIAN_POINT ( 'NONE',  ( -13.86838617718244393, 121.5005676099359846, -1.565740997395133949 ) ) ;
#27151 = CARTESIAN_POINT ( 'NONE',  ( -47.65206802627297833, 20.46304711373551299, -5.210715034831075343 ) ) ;
#27152 = FACE_OUTER_BOUND ( 'NONE', #26342, .T. ) ;
#27153 = CARTESIAN_POINT ( 'NONE',  ( 12.34427413551888719, 128.4316967252784991, -0.8534409008407578545 ) ) ;
#27154 = CARTESIAN_POINT ( 'NONE',  ( -14.67500508075667298, 148.8517222230099719, -0.2932415260845991356 ) ) ;
#27155 = EDGE_LOOP ( 'NONE', ( #36793, #2257, #11948, #38157 ) ) ;
#27156 = CARTESIAN_POINT ( 'NONE',  ( -17.40616913868966620, 140.3598469681121514, -2.385085200778919834 ) ) ;
#27157 = CARTESIAN_POINT ( 'NONE',  ( 4.642828252855901283, -15.60299999947604910, 2.403246459791627210 ) ) ;
#27158 = CARTESIAN_POINT ( 'NONE',  ( -6.513165593194060347E-14, 68.92746620154572668, -8.865348866426607246E-18 ) ) ;
#27159 = CARTESIAN_POINT ( 'NONE',  ( -4.434135272687235840, 118.1246147528386530, -0.7353779375332715196 ) ) ;
#27160 = EDGE_CURVE ( 'NONE', #332, #26503, #17728, .T. ) ;
#27161 = CARTESIAN_POINT ( 'NONE',  ( -56.21344593158320180, 5.939860726778031896, -2.828251681716873911 ) ) ;
#27162 = CARTESIAN_POINT ( 'NONE',  ( 4.756814333351318425, 117.4032681585794791, 1.206529664789174339 ) ) ;
#27163 = CARTESIAN_POINT ( 'NONE',  ( 15.09997037988943802, 131.2890697635526465, 2.122864649987123098 ) ) ;
#27164 = DIRECTION ( 'NONE',  ( -0.9998501190848634312, -0.01731298258488003436, -8.537024980200781389E-16 ) ) ;
#27165 = EDGE_CURVE ( 'NONE', #29654, #36953, #22467, .T. ) ;
#27166 = VECTOR ( 'NONE', #16321, 1000.000000000000227 ) ;
#27167 = CIRCLE ( 'NONE', #675, 0.2540000000000023350 ) ;
#27168 = CARTESIAN_POINT ( 'NONE',  ( 4.717508175643458479, 116.7562497393984415, 0.08034061319516429267 ) ) ;
#27169 = EDGE_CURVE ( 'NONE', #17039, #37617, #41579, .T. ) ;
#27170 = CARTESIAN_POINT ( 'NONE',  ( 6.435022864794023079, 6.566661361801033436, 5.478585407919045025 ) ) ;
#27171 = CARTESIAN_POINT ( 'NONE',  ( 7.919085485410333192, 154.5997988942315260, 0.6546929905378093828 ) ) ;
#27172 = CARTESIAN_POINT ( 'NONE',  ( 1.024802081479738280, 117.0751458430253393, -0.3787107017154777155 ) ) ;
#27173 = CARTESIAN_POINT ( 'NONE',  ( -13.85159022459153988, 12.96416000000000146, 5.016499999999999737 ) ) ;
#27174 = CARTESIAN_POINT ( 'NONE',  ( -58.36439606173801309, -0.2818266832427390733, 0.2195612235341721508 ) ) ;
#27175 = CARTESIAN_POINT ( 'NONE',  ( -16.23473294303261483, 121.3954344197762083, -0.2182100806314834218 ) ) ;
#27176 = EDGE_LOOP ( 'NONE', ( #2044, #34838 ) ) ;
#27177 = CARTESIAN_POINT ( 'NONE',  ( -47.24381373535820217, 25.63803778330989047, -0.2531820549803648901 ) ) ;
#27178 = CARTESIAN_POINT ( 'NONE',  ( 5.954738066914381456, 121.4009902524702369, -0.05856541418628991025 ) ) ;
#27179 = DIRECTION ( 'NONE',  ( 4.017660918040594346E-17, -1.000000000000000000, -2.376309959284834438E-19 ) ) ;
#27180 = ORIENTED_EDGE ( 'NONE', *, *, #36377, .T. ) ;
#27181 = CARTESIAN_POINT ( 'NONE',  ( 0.5071815534827258665, 115.7034655862730830, -1.744310922642317907 ) ) ;
#27182 = CARTESIAN_POINT ( 'NONE',  ( -9.426771831325675421, 124.2753396726362780, -0.5138045435804896588 ) ) ;
#27183 = CARTESIAN_POINT ( 'NONE',  ( 3.798736437616232919, -14.27876630094554500, 4.860596070177301442 ) ) ;
#27184 = CARTESIAN_POINT ( 'NONE',  ( -8.033985789953094425, 118.2752802814886053, 0.7207832311977436790 ) ) ;
#27185 = DIRECTION ( 'NONE',  ( -0.1951894777626589361, -0.9807655518882891776, 6.538892540527331846E-17 ) ) ;
#27186 = CARTESIAN_POINT ( 'NONE',  ( 0.8970928355477491012, 116.4604358222411236, 0.08699291512134199600 ) ) ;
#27187 = VERTEX_POINT ( 'NONE', #16446 ) ;
#27188 = CARTESIAN_POINT ( 'NONE',  ( -2.983771112188844832, -5.329111280313512999, 3.548611825089460048 ) ) ;
#27189 = CARTESIAN_POINT ( 'NONE',  ( -15.72148175706237971, 120.8394623874526275, -0.3311059221235124195 ) ) ;
#27190 = DIRECTION ( 'NONE',  ( 0.01997839162482749689, 1.040247600000945640E-18, -0.9998004120163610509 ) ) ;
#27191 = AXIS2_PLACEMENT_3D ( 'NONE', #31344, #20960, #24956 ) ;
#27192 = CARTESIAN_POINT ( 'NONE',  ( -10.34239276132902319, 65.15305678602257444, -1.523999999999996247 ) ) ;
#27193 = EDGE_LOOP ( 'NONE', ( #25911, #24914, #3804, #20993 ) ) ;
#27194 = CARTESIAN_POINT ( 'NONE',  ( 6.430476594291733683, 119.6278830040221948, 1.257881746540687740 ) ) ;
#27195 = VECTOR ( 'NONE', #14188, 1000.000000000000227 ) ;
#27196 = CARTESIAN_POINT ( 'NONE',  ( -3.029891238501105644, -9.367638731076009861, 3.490193963561483148 ) ) ;
#27197 = CARTESIAN_POINT ( 'NONE',  ( 22.02091170609368831, 149.7938220333360846, 1.879853634988783551 ) ) ;
#27198 = CARTESIAN_POINT ( 'NONE',  ( -58.59897934080607484, -0.2308949485131245316, -0.4634499375560702239 ) ) ;
#27199 = CARTESIAN_POINT ( 'NONE',  ( 13.60271346700648465, 122.2126086331852974, -1.213557020469313574 ) ) ;
#27200 = CARTESIAN_POINT ( 'NONE',  ( -2.488979065607898722, -9.142725400274830605, 3.900846118434742493 ) ) ;
#27201 = CARTESIAN_POINT ( 'NONE',  ( -5.389281185859767120, 158.9671755112622122, -1.064713296837521694 ) ) ;
#27202 = ORIENTED_EDGE ( 'NONE', *, *, #16771, .T. ) ;
#27203 = EDGE_LOOP ( 'NONE', ( #30166, #34921, #39899, #4962 ) ) ;
#27204 = EDGE_CURVE ( 'NONE', #26282, #41701, #37477, .T. ) ;
#27205 = CARTESIAN_POINT ( 'NONE',  ( -8.936721596564296988, 123.7033391712731145, 0.04711667938246253545 ) ) ;
#27206 = CARTESIAN_POINT ( 'NONE',  ( 6.387155697962850986, -12.89254730397265725, 0.3290856906432634288 ) ) ;
#27207 = EDGE_CURVE ( 'NONE', #22515, #29093, #29236, .T. ) ;
#27208 = CARTESIAN_POINT ( 'NONE',  ( -47.72134626993259587, 19.52826264940933498, 5.191136457141920957 ) ) ;
#27209 = DIRECTION ( 'NONE',  ( 5.206863593109713661E-17, -1.000000000000000000, 1.077750396879097183E-30 ) ) ;
#27210 = ORIENTED_EDGE ( 'NONE', *, *, #10863, .F. ) ;
#27211 = CARTESIAN_POINT ( 'NONE',  ( 11.61050889437339784, 122.1450671466348439, 1.749762830748087694 ) ) ;
#27212 = LINE ( 'NONE', #40227, #7291 ) ;
#27213 = CARTESIAN_POINT ( 'NONE',  ( 4.756911902486301358, 117.3993836135862949, 1.207145067066230038 ) ) ;
#27214 = CARTESIAN_POINT ( 'NONE',  ( -14.59306090326471050, 120.9595740141730289, 0.6228583445698290255 ) ) ;
#27215 = EDGE_CURVE ( 'NONE', #18538, #26454, #8899, .T. ) ;
#27216 = CARTESIAN_POINT ( 'NONE',  ( -3.896388542364412455, 10.26897056970580380, 7.485861278012786002 ) ) ;
#27217 = CARTESIAN_POINT ( 'NONE',  ( 7.725927843277549556, 122.1869765257964673, 0.7315739442948010485 ) ) ;
#27218 = CARTESIAN_POINT ( 'NONE',  ( -3.682264917456324227, 91.02546620154572565, -0.07358041635423968885 ) ) ;
#27219 = CIRCLE ( 'NONE', #40166, 3.175000000000001155 ) ;
#27220 = CARTESIAN_POINT ( 'NONE',  ( 21.14621813959886865, 132.3956117394162106, -0.2431941713936562333 ) ) ;
#27221 = CARTESIAN_POINT ( 'NONE',  ( -30.45812239790965492, 71.16801738242446618, -1.270000000000007567 ) ) ;
#27222 = EDGE_CURVE ( 'NONE', #35734, #38903, #777, .T. ) ;
#27223 = CARTESIAN_POINT ( 'NONE',  ( -57.26722424190899829, 2.083881049937859054, 1.598295151127536062 ) ) ;
#27224 = CARTESIAN_POINT ( 'NONE',  ( -29.57263912082353130, 58.75010695900488855, -1.524000000000004906 ) ) ;
#27225 = CARTESIAN_POINT ( 'NONE',  ( -57.07867440696631434, 2.606095844753547830, 1.988717289889800677 ) ) ;
#27226 = CARTESIAN_POINT ( 'NONE',  ( -58.27639478309521337, 0.4645451433633250860, 1.037811933420001997 ) ) ;
#27227 = CARTESIAN_POINT ( 'NONE',  ( -4.496509515934371315, 118.1299520530536569, 0.5225237042064447834 ) ) ;
#27228 = CARTESIAN_POINT ( 'NONE',  ( 2.934006498407145447, 107.6241103294071451, -4.446763787522097999 ) ) ;
#27229 = ORIENTED_EDGE ( 'NONE', *, *, #18869, .F. ) ;
#27230 = CARTESIAN_POINT ( 'NONE',  ( -46.42538233320968288, 20.85422009098716956, 4.815137874471020041 ) ) ;
#27231 = CARTESIAN_POINT ( 'NONE',  ( -8.281850670998682773, 120.0774609856632225, -1.450002526945398218 ) ) ;
#27232 = CARTESIAN_POINT ( 'NONE',  ( -7.669269000495163802, 124.9344662015457317, -0.1532502464757266591 ) ) ;
#27233 = CARTESIAN_POINT ( 'NONE',  ( 4.481705483751912134, 118.1291794842778273, 0.6917936338195805890 ) ) ;
#27234 = CARTESIAN_POINT ( 'NONE',  ( -4.540840819607181444, 155.9125706774115940, -0.9348598387858669811 ) ) ;
#27235 = CARTESIAN_POINT ( 'NONE',  ( -1.405640664959715513, 115.7027605823517717, -1.735603269989020703 ) ) ;
#27236 = AXIS2_PLACEMENT_3D ( 'NONE', #21877, #21249, #38306 ) ;
#27237 = CARTESIAN_POINT ( 'NONE',  ( 4.018990735853727791, 117.3993838140831230, -1.158690488846763955 ) ) ;
#27238 = CARTESIAN_POINT ( 'NONE',  ( 5.287753629968712232, 116.2229785614576798, -0.9666386099593877734 ) ) ;
#27239 = CARTESIAN_POINT ( 'NONE',  ( -10.33865867007045125, 123.8962982355681817, -1.239266749756491093 ) ) ;
#27240 = CARTESIAN_POINT ( 'NONE',  ( -46.96000079187150078, 20.35382130790558364, 5.064780906957706996 ) ) ;
#27241 = CARTESIAN_POINT ( 'NONE',  ( 8.618292403345778396, 118.6571538964698931, -0.8118115907002622089 ) ) ;
#27242 = CARTESIAN_POINT ( 'NONE',  ( -15.38532232246978282, 147.8388113238944186, -0.1074854512288092867 ) ) ;
#27243 = CARTESIAN_POINT ( 'NONE',  ( -6.318938770521976167, 64.36956080246774548, 1.270000000000005347 ) ) ;
#27244 = CARTESIAN_POINT ( 'NONE',  ( 9.590549175011847893, 118.2964180356302961, 0.8317573021886300877 ) ) ;
#27245 = CARTESIAN_POINT ( 'NONE',  ( 5.305748947172213015, 53.58606249999999704, -5.247078976224250013 ) ) ;
#27246 = CARTESIAN_POINT ( 'NONE',  ( 3.113553847179573175, -14.91884098843750195, 3.610284256090800170 ) ) ;
#27247 = AXIS2_PLACEMENT_3D ( 'NONE', #4295, #39431, #26426 ) ;
#27248 = CARTESIAN_POINT ( 'NONE',  ( -18.37664568872251181, 148.6295804641074483, 1.698537578660717973 ) ) ;
#27249 = CARTESIAN_POINT ( 'NONE',  ( -0.7773729966126706747, -2.891840825076433585, -0.5888577047253038543 ) ) ;
#27250 = CARTESIAN_POINT ( 'NONE',  ( -2.849674052733137231, 116.8186761214209213, -0.3958730627374473232 ) ) ;
#27251 = CARTESIAN_POINT ( 'NONE',  ( 0.8739363859948088287, 22.79536383596403226, -0.4369566804381688208 ) ) ;
#27252 = EDGE_LOOP ( 'NONE', ( #24300, #3471, #15982, #20225 ) ) ;
#27253 = CARTESIAN_POINT ( 'NONE',  ( -50.84949806483947299, 11.71728973011885344, 0.3797569051948097019 ) ) ;
#27254 = CARTESIAN_POINT ( 'NONE',  ( 5.752478121743081374, 118.4424948052634647, 0.6632437998952304126 ) ) ;
#27255 = APPLICATION_PROTOCOL_DEFINITION ( 'draft international standard', 'automotive_design', 1998, #33067 ) ;
#27256 = CARTESIAN_POINT ( 'NONE',  ( -13.50624371993754558, 134.2048320552371763, 0.5584564168634340575 ) ) ;
#27257 = CARTESIAN_POINT ( 'NONE',  ( 3.288375567735513094, -14.78372392556953585, 5.458595067156710279 ) ) ;
#27258 = CARTESIAN_POINT ( 'NONE',  ( 1.430496892223362293, 119.9358631726476574, -0.4886406555826710019 ) ) ;
#27259 = ORIENTED_EDGE ( 'NONE', *, *, #4058, .T. ) ;
#27260 = CARTESIAN_POINT ( 'NONE',  ( 3.897805094888262989, 104.6144662015456817, 2.864625572161799916 ) ) ;
#27261 = AXIS2_PLACEMENT_3D ( 'NONE', #36461, #26650, #17274 ) ;
#27262 = CARTESIAN_POINT ( 'NONE',  ( 3.282182858002726356, -14.11059071864860570, 3.604430013830858037 ) ) ;
#27263 = CARTESIAN_POINT ( 'NONE',  ( -4.908372319998136390, 117.6281534842222669, -0.9701036486395447911 ) ) ;
#27264 = CARTESIAN_POINT ( 'NONE',  ( 9.188648150231653489, 124.1858035287836231, 0.09819667026458973880 ) ) ;
#27265 = ORIENTED_EDGE ( 'NONE', *, *, #30250, .T. ) ;
#27266 = CARTESIAN_POINT ( 'NONE',  ( 4.954158841009532743, 118.5534682650580862, 1.066189120819955427 ) ) ;
#27268 = EDGE_CURVE ( 'NONE', #29626, #25154, #6211, .T. ) ;
#27267 = CARTESIAN_POINT ( 'NONE',  ( 3.276466505201106827, 108.4907294079988418, 4.202205409544957249 ) ) ;
#27269 = CARTESIAN_POINT ( 'NONE',  ( 13.46199999999999797, 12.17394877578616708, 0.000000000000000000 ) ) ;
#27270 = AXIS2_PLACEMENT_3D ( 'NONE', #34804, #12839, #16230 ) ;
#27271 = EDGE_CURVE ( 'NONE', #12580, #28646, #28826, .T. ) ;
#27272 = CARTESIAN_POINT ( 'NONE',  ( 0.01133159106138491301, 159.5297144918048673, -0.5670791535570575137 ) ) ;
#27273 = CARTESIAN_POINT ( 'NONE',  ( 23.41759249777140539, 146.8136392739129974, 0.2357739188755809401 ) ) ;
#27274 = CYLINDRICAL_SURFACE ( 'NONE', #11816, 3.175000000000001155 ) ;
#27275 = CIRCLE ( 'NONE', #32730, 5.080000000000006288 ) ;
#27276 = CARTESIAN_POINT ( 'NONE',  ( 1.921025692115251982, -15.60942222372031729, 5.455320770239441508 ) ) ;
#27277 = LINE ( 'NONE', #2356, #3164 ) ;
#27278 = CARTESIAN_POINT ( 'NONE',  ( -4.969430860872935618, 117.5911946925397871, -0.8218521176953593743 ) ) ;
#27279 = CARTESIAN_POINT ( 'NONE',  ( 20.53125589898976244, 145.6130255286810495, 2.451886524809591350 ) ) ;
#27280 = ORIENTED_EDGE ( 'NONE', *, *, #25909, .T. ) ;
#27281 = CARTESIAN_POINT ( 'NONE',  ( -7.794209556482943668, 13.03656553185805222, 3.210957146378262461 ) ) ;
#27282 = CARTESIAN_POINT ( 'NONE',  ( 2.482649978626910059, 117.4442030770385941, -0.6349463395262938681 ) ) ;
#27283 = CARTESIAN_POINT ( 'NONE',  ( -2.302803873444659644, 118.9955205646042344, -0.7292456921539737236 ) ) ;
#27284 = CARTESIAN_POINT ( 'NONE',  ( -17.14500000000466784, 71.11999999999886768, -1.524000000000000909 ) ) ;
#27285 = CARTESIAN_POINT ( 'NONE',  ( -6.350000000000054712, 86.35999999999998522, 7.776507174585692163E-16 ) ) ;
#27286 = CARTESIAN_POINT ( 'NONE',  ( -0.01180776361650071223, 120.3637084677655764, 0.5909087754570012674 ) ) ;
#27287 = CARTESIAN_POINT ( 'NONE',  ( 4.076717266748975277, 8.489475128091552136, -2.202413229635628689 ) ) ;
#27288 = CARTESIAN_POINT ( 'NONE',  ( -8.095114962461808616, 74.19100168833409725, 1.270000000000002460 ) ) ;
#27289 = CARTESIAN_POINT ( 'NONE',  ( -4.765964266679635131, 118.5264896598256854, 0.8411723569164160086 ) ) ;
#27290 = CARTESIAN_POINT ( 'NONE',  ( 3.260250311156894121, -12.89034478651954174, 1.323980178024680043 ) ) ;
#27291 = CARTESIAN_POINT ( 'NONE',  ( 0.9873284109326271318, 106.8474934270474392, -4.901623504225490535 ) ) ;
#27292 = CARTESIAN_POINT ( 'NONE',  ( 1.952296795662580298, 38.90900249396371180, 1.348506300408716552 ) ) ;
#27293 = CARTESIAN_POINT ( 'NONE',  ( -7.868930244179279221, 69.75330307926518003, -1.523999999999995802 ) ) ;
#27294 = EDGE_LOOP ( 'NONE', ( #38695, #27774, #717, #3944 ) ) ;
#27295 = CARTESIAN_POINT ( 'NONE',  ( -3.054491883998568191, 105.1240845014440453, -4.374327510956630860 ) ) ;
#27296 = CARTESIAN_POINT ( 'NONE',  ( 3.739721301978734314, -15.76301488427489517, 4.305968564470687987 ) ) ;
#27297 = CARTESIAN_POINT ( 'NONE',  ( -19.50591060256589415, 149.0830822498907082, 1.724197071773047707 ) ) ;
#27298 = CIRCLE ( 'NONE', #37508, 6.349999999999999645 ) ;
#27299 = CARTESIAN_POINT ( 'NONE',  ( 1.104432469574216480, -9.427232690354344413, -4.492858291722996888 ) ) ;
#27300 = ORIENTED_EDGE ( 'NONE', *, *, #7804, .F. ) ;
#27301 = ORIENTED_EDGE ( 'NONE', *, *, #5270, .T. ) ;
#27302 = FACE_OUTER_BOUND ( 'NONE', #14895, .T. ) ;
#27303 = CARTESIAN_POINT ( 'NONE',  ( 2.988627099740976512, 122.7580772961051707, 0.2146329844597062719 ) ) ;
#27304 = B_SPLINE_SURFACE_WITH_KNOTS ( 'NONE', 3, 1, ( 
 ( #22638, #36098 ),
 ( #3940, #740 ),
 ( #36511, #32682 ),
 ( #23274, #29266 ) ),
 .UNSPECIFIED., .F., .F., .F.,
 ( 4, 4 ),
 ( 2, 2 ),
 ( 0.000000000000000000, 0.6118630412642114269 ),
 ( 0.000000000000000000, 1.000000000000000000 ),
 .UNSPECIFIED. ) ;
#27305 = CARTESIAN_POINT ( 'NONE',  ( -14.53352838467451313, 150.4300676932417389, 1.118949361739814519 ) ) ;
#27306 = DIRECTION ( 'NONE',  ( -4.017660918040594346E-17, 1.000000000000000000, 2.376309959284834438E-19 ) ) ;
#27307 = CARTESIAN_POINT ( 'NONE',  ( 0.5348915910373366334, 119.5442839488369628, -0.5285302399602642698 ) ) ;
#27308 = AXIS2_PLACEMENT_3D ( 'NONE', #15885, #12909, #13124 ) ;
#27309 = CARTESIAN_POINT ( 'NONE',  ( -20.67294874948574801, 147.9587796579421308, -2.444796510662507139 ) ) ;
#27310 = CYLINDRICAL_SURFACE ( 'NONE', #9313, 0.2540000000000035008 ) ;
#27311 = CARTESIAN_POINT ( 'NONE',  ( 4.287347022130586716, 118.2136450426441598, -0.3572067982262181474 ) ) ;
#27312 = CARTESIAN_POINT ( 'NONE',  ( 5.231962949222344506, 121.1607713875043117, -0.2380388119251649337 ) ) ;
#27313 = ORIENTED_EDGE ( 'NONE', *, *, #40749, .F. ) ;
#27314 = CARTESIAN_POINT ( 'NONE',  ( 2.931439949929583122, -14.82325452411255640, 4.117531814738872420 ) ) ;
#27315 = CIRCLE ( 'NONE', #13726, 2.540000000000000480 ) ;
#27316 = DIRECTION ( 'NONE',  ( -9.627370216492862708E-17, -1.000000000000000000, 0.000000000000000000 ) ) ;
#27317 = CARTESIAN_POINT ( 'NONE',  ( -58.31893842775810555, -0.1844529990621818216, 0.2851935484600691129 ) ) ;
#27318 = EDGE_CURVE ( 'NONE', #10591, #32067, #5994, .T. ) ;
#27319 = CARTESIAN_POINT ( 'NONE',  ( 4.135298993362768627, -14.76517611359900961, -2.065434832541708676 ) ) ;
#27320 = CARTESIAN_POINT ( 'NONE',  ( 13.16414530391289617, 152.2904283036577908, 1.902647459344306791 ) ) ;
#27321 = CARTESIAN_POINT ( 'NONE',  ( 2.928799644063047936, 38.81416391459460158, 1.351591292951386469 ) ) ;
#27322 = CARTESIAN_POINT ( 'NONE',  ( -5.936300781872430932, 120.8604418758245487, 0.1421746502253222466 ) ) ;
#27323 = AXIS2_PLACEMENT_3D ( 'NONE', #34719, #21280, #41330 ) ;
#27324 = AXIS2_PLACEMENT_3D ( 'NONE', #7128, #20084, #3938 ) ;
#27325 = CARTESIAN_POINT ( 'NONE',  ( -0.5093740622119584671, 14.76157059199007016, 4.595130897425484306 ) ) ;
#27326 = CARTESIAN_POINT ( 'NONE',  ( 15.72560005962091800, 146.8994026175788008, 0.4425663129111797600 ) ) ;
#27327 = DIRECTION ( 'NONE',  ( -0.8745520943968240202, 0.4849315768086553402, -6.829619984160650158E-16 ) ) ;
#27328 = CARTESIAN_POINT ( 'NONE',  ( -51.67551711146813176, 11.54346324480936481, -1.411685438026464290 ) ) ;
#27329 = CARTESIAN_POINT ( 'NONE',  ( 2.179771977182863640, 116.2367762333986718, -0.09915394068943080008 ) ) ;
#27330 = CARTESIAN_POINT ( 'NONE',  ( 0.003708075274061980488, 123.1683257372384901, -0.1855672496570262564 ) ) ;
#27331 = DIRECTION ( 'NONE',  ( -0.8745520943968240202, 0.4849315768086553402, -6.829619984160650158E-16 ) ) ;
#27332 = DIRECTION ( 'NONE',  ( -0.8745520943968240202, 0.4849315768086551737, -5.361993529360572958E-16 ) ) ;
#27333 = CARTESIAN_POINT ( 'NONE',  ( -29.79391970823417068, 57.88946435433149418, -1.524000000000004240 ) ) ;
#27334 = CARTESIAN_POINT ( 'NONE',  ( -2.337594367139880003, 4.813278044257511823, 8.129740476481943645 ) ) ;
#27335 = CARTESIAN_POINT ( 'NONE',  ( -4.781529118576368198, 56.51499999999999346, 4.872211946655436776 ) ) ;
#27336 = DIRECTION ( 'NONE',  ( 5.188838149069472160E-16, -1.699382548006136559E-16, -1.000000000000000000 ) ) ;
#27337 = CARTESIAN_POINT ( 'NONE',  ( -57.90853684698413417, 2.514838786807874094, 0.1030880274588810847 ) ) ;
#27338 = CARTESIAN_POINT ( 'NONE',  ( 0.005099097579422138225, 122.5569158606516993, -0.2551796940111168976 ) ) ;
#27339 = CARTESIAN_POINT ( 'NONE',  ( -5.826550815406482009, 117.0573985505404693, 0.1859578237674348045 ) ) ;
#27340 = EDGE_LOOP ( 'NONE', ( #22094, #6276, #40561, #41316 ) ) ;
#27341 = CARTESIAN_POINT ( 'NONE',  ( -58.08922378330620973, 1.909136410080003454, -0.4248916911265372964 ) ) ;
#27342 = VERTEX_POINT ( 'NONE', #15818 ) ;
#27343 = CARTESIAN_POINT ( 'NONE',  ( -45.89458612274419380, 20.88821703127394969, -4.453918368557551410 ) ) ;
#27344 = CARTESIAN_POINT ( 'NONE',  ( -7.546549060383340723, 122.4259254537243464, -0.1108676762560423107 ) ) ;
#27345 = CARTESIAN_POINT ( 'NONE',  ( 5.611968257679588845, -14.69514533571547688, 3.041973840610588287 ) ) ;
#27346 = CARTESIAN_POINT ( 'NONE',  ( -20.57754816582981405, 149.5144255282053223, 1.563875036196712642 ) ) ;
#27347 = CARTESIAN_POINT ( 'NONE',  ( 23.13850227319423780, 149.2833505036244048, 1.057685438456114957 ) ) ;
#27348 = CARTESIAN_POINT ( 'NONE',  ( 5.427513099616278147, 158.9671755112622122, -0.8485680044740093741 ) ) ;
#27349 = CARTESIAN_POINT ( 'NONE',  ( -32.60270662228668925, 51.47373954847018496, 1.269999999999993356 ) ) ;
#27350 = CARTESIAN_POINT ( 'NONE',  ( -20.28976221201026320, 128.9598305440861452, -0.6839793015867964288 ) ) ;
#27351 = CARTESIAN_POINT ( 'NONE',  ( -48.71949277200916129, 18.24443030291588386, -5.160461098695489746 ) ) ;
#27352 = ORIENTED_EDGE ( 'NONE', *, *, #3872, .T. ) ;
#27353 = CARTESIAN_POINT ( 'NONE',  ( 5.556916953519710489, 116.7209935381689974, 0.2595115648362693594 ) ) ;
#27354 = CARTESIAN_POINT ( 'NONE',  ( -15.71777585039863645, 134.9797526104055123, 1.508943449597504705 ) ) ;
#27355 = CARTESIAN_POINT ( 'NONE',  ( -57.84176729718492993, 0.8471481974509047497, -1.053121747471209346 ) ) ;
#27356 = EDGE_CURVE ( 'NONE', #2001, #19344, #35420, .T. ) ;
#27357 = CARTESIAN_POINT ( 'NONE',  ( 8.434619947227306014, 156.6436466068687423, -1.738452918000226388 ) ) ;
#27358 = CARTESIAN_POINT ( 'NONE',  ( 0.5763570944828283471, -5.266575483494631449, -0.7860673829877594665 ) ) ;
#27359 = CARTESIAN_POINT ( 'NONE',  ( -21.10167996235837862, 141.7209635633906259, -2.240609589767335041 ) ) ;
#27360 = CARTESIAN_POINT ( 'NONE',  ( -46.42538233320968288, 20.85422009098716956, -4.815137874471035140 ) ) ;
#27361 = TOROIDAL_SURFACE ( 'NONE', #32808, 0.3809999999999999498, 0.2540000000000000036 ) ;
#27362 = EDGE_CURVE ( 'NONE', #2187, #4024, #25893, .T. ) ;
#27363 = CARTESIAN_POINT ( 'NONE',  ( 16.60605961459992130, 147.5857818452174115, -1.108006280952564815 ) ) ;
#27364 = DIRECTION ( 'NONE',  ( 1.000000000000000000, 0.000000000000000000, -1.224646799147351728E-16 ) ) ;
#27365 = ORIENTED_EDGE ( 'NONE', *, *, #13555, .F. ) ;
#27366 = CARTESIAN_POINT ( 'NONE',  ( -18.34612162485809606, 147.3262642721504960, -2.396769171045068703 ) ) ;
#27367 = CARTESIAN_POINT ( 'NONE',  ( 4.856922264871083250, -15.58127974107270575, 2.741789226191331252 ) ) ;
#27368 = CARTESIAN_POINT ( 'NONE',  ( -19.04204117267709506, 56.84332656279845963, -1.269999999999999130 ) ) ;
#27369 = CARTESIAN_POINT ( 'NONE',  ( -4.303161701476582834, 118.2117301101246341, -0.4941263280093639021 ) ) ;
#27370 = ADVANCED_FACE ( 'NONE', ( #9436 ), #29307, .T. ) ;
#27371 = CARTESIAN_POINT ( 'NONE',  ( -53.17586183559576085, 10.67386474145934372, -4.017225210190888518 ) ) ;
#27372 = AXIS2_PLACEMENT_3D ( 'NONE', #31616, #15834, #9867 ) ;
#27373 = CARTESIAN_POINT ( 'NONE',  ( 4.106383402388294357, 118.2429491485453354, 0.3519430347307819229 ) ) ;
#27374 = CARTESIAN_POINT ( 'NONE',  ( 18.09674421129283672, 146.7121067869193496, 2.346545542165937803 ) ) ;
#27375 = CARTESIAN_POINT ( 'NONE',  ( 23.36121599382897074, 148.8756354988261990, 0.4668126921608657942 ) ) ;
#27376 = CARTESIAN_POINT ( 'NONE',  ( -0.9514613986627886710, 10.21077804425927305, -8.405459466743828045 ) ) ;
#27377 = CARTESIAN_POINT ( 'NONE',  ( 15.32065199451904647, 143.5038931315047535, 0.7650733020788533789 ) ) ;
#27378 = EDGE_CURVE ( 'NONE', #3540, #41261, #22519, .T. ) ;
#27379 = CARTESIAN_POINT ( 'NONE',  ( 10.39199171643957698, 157.8614378686282862, -0.7539791864280579459 ) ) ;
#27380 = CARTESIAN_POINT ( 'NONE',  ( 5.332935397695205637, 105.1224662015457199, 0.1065647409268305201 ) ) ;
#27381 = CARTESIAN_POINT ( 'NONE',  ( 3.999888396376028332, 115.6909491485452435, 1.587082580931593379 ) ) ;
#27382 = AXIS2_PLACEMENT_3D ( 'NONE', #10101, #29275, #17118 ) ;
#27383 = CARTESIAN_POINT ( 'NONE',  ( -57.94149553976682654, 0.5275954726333825784, 0.3053296928521371800 ) ) ;
#27384 = CARTESIAN_POINT ( 'NONE',  ( -21.90557141593814094, 151.4352167165723415, -0.3614719721193417334 ) ) ;
#27385 = EDGE_LOOP ( 'NONE', ( #35260, #7835, #6488, #29149 ) ) ;
#27386 = CARTESIAN_POINT ( 'NONE',  ( -46.60530155212504155, 26.17382724835477248, -0.2116666666666759400 ) ) ;
#27387 = CARTESIAN_POINT ( 'NONE',  ( -5.800372561083844580, 121.2106355307726346, -0.4875482425884115623 ) ) ;
#27388 = FACE_OUTER_BOUND ( 'NONE', #10007, .T. ) ;
#27389 = CARTESIAN_POINT ( 'NONE',  ( 0.4392373074537823663, 115.6909491485452719, -1.750094695205981044 ) ) ;
#27390 = CARTESIAN_POINT ( 'NONE',  ( -13.62587875280891581, 150.2122286517991085, -0.5925390977946540794 ) ) ;
#27391 = CARTESIAN_POINT ( 'NONE',  ( 4.721845526343314781, -13.23797770169883670, 3.222865150663026590 ) ) ;
#27392 = CARTESIAN_POINT ( 'NONE',  ( -14.19262213114356896, 155.9232964860746620, 1.164639009528573022 ) ) ;
#27393 = CARTESIAN_POINT ( 'NONE',  ( -6.073982626572030696, 78.87340550758391089, -4.346604155593818852 ) ) ;
#27394 = CARTESIAN_POINT ( 'NONE',  ( 23.27880353394119339, 149.3453998935430604, 0.6192278183506786382 ) ) ;
#27395 = CARTESIAN_POINT ( 'NONE',  ( 10.39478676155560244, 153.1349730030725595, 0.2678714069608246762 ) ) ;
#27396 = ORIENTED_EDGE ( 'NONE', *, *, #14466, .T. ) ;
#27397 = CARTESIAN_POINT ( 'NONE',  ( 0.9280917288853990366, 18.63875360461660335, -0.3060232888646727822 ) ) ;
#27398 = EDGE_CURVE ( 'NONE', #40763, #39372, #21832, .T. ) ;
#27399 = CARTESIAN_POINT ( 'NONE',  ( -10.82992898448790520, 157.9016520041087688, -0.2364045824791623507 ) ) ;
#27400 = CARTESIAN_POINT ( 'NONE',  ( -42.82337701166415656, 22.05454930919483303, -2.000910692578694583 ) ) ;
#27401 = CIRCLE ( 'NONE', #30795, 3.683000000000001162 ) ;
#27402 = DIRECTION ( 'NONE',  ( -5.188838149069471174E-16, 1.699382548006136313E-16, 1.000000000000000000 ) ) ;
#27403 = ORIENTED_EDGE ( 'NONE', *, *, #3466, .F. ) ;
#27404 = CARTESIAN_POINT ( 'NONE',  ( 5.609552972221978351, 119.8608102258102690, 1.095074600700395306 ) ) ;
#27405 = CARTESIAN_POINT ( 'NONE',  ( 4.587442282481145384, -5.694351208059624803, -0.5507456681084095251 ) ) ;
#27406 = CARTESIAN_POINT ( 'NONE',  ( 10.97563396989510132, 119.3804150619309468, 1.219877759958876595 ) ) ;
#27407 = CARTESIAN_POINT ( 'NONE',  ( -58.73303099469992361, -0.3138845496180736605, -0.2515151591905351314 ) ) ;
#27408 = CARTESIAN_POINT ( 'NONE',  ( 6.797121414357278901, 118.7881172115286148, -0.9472104157431980864 ) ) ;
#27409 = CARTESIAN_POINT ( 'NONE',  ( 3.573240411403531436, -4.819783300376494495, -2.961220487682876268 ) ) ;
#27410 = CARTESIAN_POINT ( 'NONE',  ( -19.15327062675862280, 128.6826163344482268, -1.506695251711823058 ) ) ;
#27411 = EDGE_CURVE ( 'NONE', #11774, #10192, #26628, .T. ) ;
#27412 = ORIENTED_EDGE ( 'NONE', *, *, #39678, .F. ) ;
#27413 = CARTESIAN_POINT ( 'NONE',  ( -6.023029630345043905, 155.3544091381320982, 0.1360875627331028515 ) ) ;
#27414 = CARTESIAN_POINT ( 'NONE',  ( 2.468517452056580463, -15.43523125850157562, 5.870468177969554446 ) ) ;
#27415 = CARTESIAN_POINT ( 'NONE',  ( 5.167420783512489457, 115.6909491485453145, 1.238004321684439191 ) ) ;
#27416 = AXIS2_PLACEMENT_3D ( 'NONE', #13253, #9842, #33069 ) ;
#27417 = CARTESIAN_POINT ( 'NONE',  ( -0.5456937337276765998, 117.3993834314855462, -1.492633053494221596 ) ) ;
#27418 = VERTEX_POINT ( 'NONE', #35859 ) ;
#27419 = CARTESIAN_POINT ( 'NONE',  ( 5.003445044761828164, 119.2220797256985350, 1.100019038710256414 ) ) ;
#27420 = CARTESIAN_POINT ( 'NONE',  ( -5.684927786827005392, 65.51297084251929448, -1.523999999999993804 ) ) ;
#27421 = CARTESIAN_POINT ( 'NONE',  ( -29.30640055155810941, 61.36565346392652742, -1.270000000000005791 ) ) ;
#27422 = AXIS2_PLACEMENT_3D ( 'NONE', #18035, #28480, #21850 ) ;
#27423 = CARTESIAN_POINT ( 'NONE',  ( -5.863496024706905452, 117.4684171610355747, 0.5179920176435335311 ) ) ;
#27424 = CARTESIAN_POINT ( 'NONE',  ( -8.197529660144020625, 8.984976746712527884, 2.078235512056660017 ) ) ;
#27425 = CARTESIAN_POINT ( 'NONE',  ( 15.16020740373466325, 148.9716719698033387, 1.401450122450045521 ) ) ;
#27426 = LINE ( 'NONE', #11231, #32176 ) ;
#27427 = EDGE_CURVE ( 'NONE', #32767, #21511, #38851, .T. ) ;
#27428 = CARTESIAN_POINT ( 'NONE',  ( 23.06568927493560750, 148.7220611141358404, -0.3950670065760722438 ) ) ;
#27429 = CARTESIAN_POINT ( 'NONE',  ( -6.194847070882102180, 64.72978607931611350, 1.524000000000005350 ) ) ;
#27430 = CARTESIAN_POINT ( 'NONE',  ( -57.31459482202865985, 1.982415423992395453, 1.558968780848406954 ) ) ;
#27431 = CARTESIAN_POINT ( 'NONE',  ( -58.40597088826705630, 0.2738206778524349128, 0.9753506901443759203 ) ) ;
#27432 = CARTESIAN_POINT ( 'NONE',  ( -58.64969807691807091, -0.3154622663803800520, 0.3299468374515310276 ) ) ;
#27433 = CARTESIAN_POINT ( 'NONE',  ( -4.120329755912500502, 118.2429491485453354, 0.1840211939346729775 ) ) ;
#27434 = CARTESIAN_POINT ( 'NONE',  ( 3.444129741522558685, 108.1634925278479500, -4.064689422066845026 ) ) ;
#27435 = ORIENTED_EDGE ( 'NONE', *, *, #22462, .T. ) ;
#27436 = EDGE_CURVE ( 'NONE', #24265, #19534, #2133, .T. ) ;
#27437 = CARTESIAN_POINT ( 'NONE',  ( -50.36516092884956208, 15.79195539882771726, 4.916963016749596349 ) ) ;
#27438 = CARTESIAN_POINT ( 'NONE',  ( 6.316787761850397587, 119.8961530332412195, -0.9708787764513430174 ) ) ;
#27439 = CARTESIAN_POINT ( 'NONE',  ( -6.329649118423223086, 120.0627515544778134, -0.4542292512502629220 ) ) ;
#27440 = AXIS2_PLACEMENT_3D ( 'NONE', #12556, #38548, #35349 ) ;
#27441 = CARTESIAN_POINT ( 'NONE',  ( 4.392636428124883530, 118.1805772463083599, 0.5719164910104670430 ) ) ;
#27442 = CARTESIAN_POINT ( 'NONE',  ( -16.11589901136889935, 145.8839827664328368, -1.295141180005177528 ) ) ;
#27443 = CARTESIAN_POINT ( 'NONE',  ( -0.9954745042087072004, 115.7029401122920973, -1.748196735769753873 ) ) ;
#27444 = CARTESIAN_POINT ( 'NONE',  ( 2.732111087507031133, 116.5293111276780849, 0.05459408159141355271 ) ) ;
#27445 = ORIENTED_EDGE ( 'NONE', *, *, #26308, .T. ) ;
#27446 = CARTESIAN_POINT ( 'NONE',  ( 1.581412096509125842, 106.2431249238853894, -5.111785082781967304 ) ) ;
#27447 = CARTESIAN_POINT ( 'NONE',  ( -4.409042980950640178, 120.6578283891288379, -0.6218799582752131405 ) ) ;
#27448 = B_SPLINE_CURVE_WITH_KNOTS ( 'NONE', 3,
 ( #30673, #34309, #15101, #1521, #40496, #11291 ),
 .UNSPECIFIED., .F., .F.,
 ( 4, 2, 4 ),
 ( 0.000000000000000000, 0.5000000000000000000, 1.000000000000000000 ),
 .UNSPECIFIED. ) ;
#27449 = CARTESIAN_POINT ( 'NONE',  ( -41.05192305526439611, 23.09448250258611068, -1.270000000023978615 ) ) ;
#27450 = CARTESIAN_POINT ( 'NONE',  ( -44.28332145682819743, 21.53821517059777335, 3.041508016571806028 ) ) ;
#27451 = CARTESIAN_POINT ( 'NONE',  ( 10.19284229789036900, 16.51000000000000156, 4.908176479697702099 ) ) ;
#27452 = CARTESIAN_POINT ( 'NONE',  ( -9.059071224495744090, 124.2128079895686170, -0.04632541238150574697 ) ) ;
#27453 = ADVANCED_FACE ( 'NONE', ( #28614 ), #12432, .T. ) ;
#27454 = DIRECTION ( 'NONE',  ( -5.188838149069472160E-16, 1.699382548006136559E-16, 1.000000000000000000 ) ) ;
#27455 = CARTESIAN_POINT ( 'NONE',  ( 22.93196816944033856, 148.6798292920915117, 1.431318312106270474 ) ) ;
#27456 = CARTESIAN_POINT ( 'NONE',  ( 5.871452009091314039, 65.30181249999998272, -5.016499999999999737 ) ) ;
#27458 = CARTESIAN_POINT ( 'NONE',  ( 21.68796372492886704, 149.3076860495818323, -1.274097349589627282 ) ) ;
#27457 = CARTESIAN_POINT ( 'NONE',  ( 2.770264620702337588, -13.86593384134129892, 0.2159450460461957433 ) ) ;
#27459 = CARTESIAN_POINT ( 'NONE',  ( -0.03212616895158381530, 157.6269964811067155, 1.607724863813389415 ) ) ;
#27460 = CARTESIAN_POINT ( 'NONE',  ( 0.9235644399502331847, -7.204839741120207641, 0.3177745608231433705 ) ) ;
#27461 = CARTESIAN_POINT ( 'NONE',  ( -3.829241263245407367, 116.9593488885201538, -0.4901781634895738260 ) ) ;
#27462 = AXIS2_PLACEMENT_3D ( 'NONE', #27105, #3923, #4346 ) ;
#27463 = EDGE_CURVE ( 'NONE', #27491, #1397, #13478, .T. ) ;
#27464 = CARTESIAN_POINT ( 'NONE',  ( -0.7014129483091587902, 16.11884676413550466, -0.6771123631929140130 ) ) ;
#27465 = ORIENTED_EDGE ( 'NONE', *, *, #39123, .F. ) ;
#27466 = B_SPLINE_CURVE_WITH_KNOTS ( 'NONE', 3,
 ( #2348, #14885, #31289, #41318, #28095, #8930, #28522, #41530, #9146, #25323, #37693, #22104, #35132 ),
 .UNSPECIFIED., .F., .F.,
 ( 4, 1, 1, 1, 1, 1, 1, 1, 1, 1, 4 ),
 ( 0.000000000000000000, 0.1249999999999999167, 0.1767086109055020227, 0.2499999999999998335, 0.3750000000000003886, 0.5000000000000003331, 0.5890287030183404271, 0.6249999999999998890, 0.7499999999999995559, 0.8749999999999997780, 1.000000000000000000 ),
 .UNSPECIFIED. ) ;
#27467 = CARTESIAN_POINT ( 'NONE',  ( -51.67551711146813176, 11.54346324480936481, 1.411685438026446526 ) ) ;
#27468 = CARTESIAN_POINT ( 'NONE',  ( -8.914966108837955261, 123.2307073318660855, 0.3922733289213622410 ) ) ;
#27469 = CARTESIAN_POINT ( 'NONE',  ( 2.370890509137566937, -15.02769382788871155, 5.804473790077508077 ) ) ;
#27470 = CARTESIAN_POINT ( 'NONE',  ( 4.378102236263064384, 120.3584862571861436, -0.5730137456143137298 ) ) ;
#27471 = AXIS2_PLACEMENT_3D ( 'NONE', #23417, #20435, #16404 ) ;
#27472 = ORIENTED_EDGE ( 'NONE', *, *, #8400, .T. ) ;
#27473 = DIRECTION ( 'NONE',  ( 1.011795553208986377E-16, 1.000000000000000000, -0.000000000000000000 ) ) ;
#27474 = CARTESIAN_POINT ( 'NONE',  ( 3.202083396006969895, -13.65749169606385394, 1.964591208077046902 ) ) ;
#27475 = CARTESIAN_POINT ( 'NONE',  ( -5.212520885064538589, 31.45212241211192605, -0.4657032193360506334 ) ) ;
#27476 = CARTESIAN_POINT ( 'NONE',  ( 8.794423163103090246, 123.6850765633735421, 0.1423839433359068429 ) ) ;
#27477 = VERTEX_POINT ( 'NONE', #36066 ) ;
#27478 = CARTESIAN_POINT ( 'NONE',  ( 6.734570810858505396, 118.9580315507705706, 1.247721039026444600 ) ) ;
#27479 = CARTESIAN_POINT ( 'NONE',  ( 1.187367250949410868, 106.3000011757731187, 5.151998247764457695 ) ) ;
#27480 = PLANE ( 'NONE',  #14333 ) ;
#27481 = DIRECTION ( 'NONE',  ( -5.188838149069472160E-16, 1.699382548006136559E-16, 1.000000000000000000 ) ) ;
#27482 = VECTOR ( 'NONE', #1934, 1000.000000000000000 ) ;
#27483 = CARTESIAN_POINT ( 'NONE',  ( 0.002426349801083684584, 116.5266044092193880, -0.1214244658147704270 ) ) ;
#27484 = CYLINDRICAL_SURFACE ( 'NONE', #32239, 0.6349999999999984546 ) ;
#27485 = AXIS2_PLACEMENT_3D ( 'NONE', #30962, #34177, #12429 ) ;
#27486 = CARTESIAN_POINT ( 'NONE',  ( 1.844779171034190757, -15.45366112431178962, 5.998838294486427358 ) ) ;
#27487 = DIRECTION ( 'NONE',  ( 5.188838149069472160E-16, -1.699382548006136559E-16, -1.000000000000000000 ) ) ;
#27488 = DIRECTION ( 'NONE',  ( 0.4849315768086534528, 0.8745520943968250194, 1.030032898892974942E-16 ) ) ;
#27489 = EDGE_CURVE ( 'NONE', #11121, #5326, #25237, .T. ) ;
#27490 = CARTESIAN_POINT ( 'NONE',  ( -4.744868711034945896, 117.8975728021022604, 0.7672496759666370680 ) ) ;
#27491 = VERTEX_POINT ( 'NONE', #506 ) ;
#27492 = CARTESIAN_POINT ( 'NONE',  ( -6.929632415086860675, 11.50928017261270497, -4.815005168835179816 ) ) ;
#27493 = B_SPLINE_CURVE_WITH_KNOTS ( 'NONE', 3,
 ( #16979, #36596, #10172, #17192, #23359, #27001, #26791, #36808, #39583, #40012, #29979, #13374, #7625, #20584, #4443, #17401, #405, #36178, #30396, #6997, #1245, #14202, #27208, #11017 ),
 .UNSPECIFIED., .F., .F.,
 ( 4, 2, 2, 2, 2, 2, 2, 2, 2, 2, 2, 4 ),
 ( 0.000000000000000000, 0.001112600682894235998, 0.001668901024341350962, 0.002225201365788466359, 0.003337802048682695852, 0.004450402731576926646, 0.005563003414471156573, 0.006675604097365384765, 0.007231904438812500162, 0.007788204780259614692, 0.008344505121706728354, 0.008900805463153842884 ),
 .UNSPECIFIED. ) ;
#27494 = CARTESIAN_POINT ( 'NONE',  ( -8.398419497799205047, 119.5137114544897088, -1.401694671710796314 ) ) ;
#27495 = CARTESIAN_POINT ( 'NONE',  ( -3.099458292115011115, 117.0475107411037641, -1.222660999933594450 ) ) ;
#27497 = CARTESIAN_POINT ( 'NONE',  ( 4.726358237794381800, 117.7280284874452860, 1.096895477954969556 ) ) ;
#27496 = VECTOR ( 'NONE', #9756, 1000.000000000000000 ) ;
#27498 = CYLINDRICAL_SURFACE ( 'NONE', #33841, 2.540000000000000480 ) ;
#27499 = CARTESIAN_POINT ( 'NONE',  ( -0.01635612297686582159, 119.2343925067225427, 0.8185272769044252827 ) ) ;
#27500 = CARTESIAN_POINT ( 'NONE',  ( 1.068493265602401987, 5.690783753869971484, 4.496582723949734017 ) ) ;
#27501 = FACE_OUTER_BOUND ( 'NONE', #18460, .T. ) ;
#27502 = CARTESIAN_POINT ( 'NONE',  ( -5.252607328145010079, 115.6909491485453003, 0.9237163795073232153 ) ) ;
#27503 = CARTESIAN_POINT ( 'NONE',  ( 3.201139452527619333, -14.28037012539873274, 4.574913560108570643 ) ) ;
#27504 = CARTESIAN_POINT ( 'NONE',  ( 4.107119205180127963, 117.8719421043398370, -0.6926522829710090035 ) ) ;
#27505 = CARTESIAN_POINT ( 'NONE',  ( -4.456559794634359584, 27.80638087737987973, 0.5384073243751467119 ) ) ;
#27506 = CARTESIAN_POINT ( 'NONE',  ( -1.423643091077623879, 115.7027630026304337, 1.681650016434340422 ) ) ;
#27507 = ORIENTED_EDGE ( 'NONE', *, *, #7319, .T. ) ;
#27508 = CARTESIAN_POINT ( 'NONE',  ( -5.183055225334214811, 105.1221871011891125, -1.273223601473996158 ) ) ;
#27509 = AXIS2_PLACEMENT_3D ( 'NONE', #13652, #32408, #26432 ) ;
#27510 = CARTESIAN_POINT ( 'NONE',  ( 5.161689517976459030, -15.45231451347503437, 1.550260198497607877 ) ) ;
#27511 = CARTESIAN_POINT ( 'NONE',  ( -19.17595810167867398, 140.9752145814059645, 1.751973952106584020 ) ) ;
#27512 = EDGE_CURVE ( 'NONE', #22599, #4427, #26465, .T. ) ;
#27513 = CARTESIAN_POINT ( 'NONE',  ( -0.9636992805836054332, 23.18535052081312386, 0.1494942155713751553 ) ) ;
#27514 = ORIENTED_EDGE ( 'NONE', *, *, #33425, .T. ) ;
#27515 = EDGE_LOOP ( 'NONE', ( #29058, #2852, #17557, #8902, #16605, #23021, #772 ) ) ;
#27516 = CARTESIAN_POINT ( 'NONE',  ( -4.230865311087580238, 31.47871655110595768, -0.6839938589234777488 ) ) ;
#27517 = CARTESIAN_POINT ( 'NONE',  ( 2.726848673931656197, 121.4869043954268903, 0.3408589522888662571 ) ) ;
#27518 = SURFACE_STYLE_FILL_AREA ( #20688 ) ;
#27519 = CARTESIAN_POINT ( 'NONE',  ( -3.575420174884087476, 120.5283240077024800, 0.4162329711438423341 ) ) ;
#27520 = CARTESIAN_POINT ( 'NONE',  ( -41.53952017147561548, 22.95708954751533781, 1.524002587545546294 ) ) ;
#27521 = CARTESIAN_POINT ( 'NONE',  ( 4.519236749211172466, 118.0837734081209192, -0.6171982530284805257 ) ) ;
#27522 = CARTESIAN_POINT ( 'NONE',  ( 1.377724515701647334, 119.5584937100158243, -0.5648184346096530861 ) ) ;
#27523 = CARTESIAN_POINT ( 'NONE',  ( -0.4261125263670469954, 118.2558431149878402, -0.5943921922486901099 ) ) ;
#27524 = CARTESIAN_POINT ( 'NONE',  ( 1.734723475976807094E-15, 17.14499999999999957, 0.000000000000000000 ) ) ;
#27525 = VERTEX_POINT ( 'NONE', #23244 ) ;
#27526 = CARTESIAN_POINT ( 'NONE',  ( 4.288979916322937846, 118.2138448364286347, -0.3554799478401594048 ) ) ;
#27527 = CARTESIAN_POINT ( 'NONE',  ( 5.903620821223727333, 121.4229528491920576, -0.1845582724821505927 ) ) ;
#27528 = ORIENTED_EDGE ( 'NONE', *, *, #26904, .F. ) ;
#27529 = CARTESIAN_POINT ( 'NONE',  ( 3.076715286590720133, -14.17522324541667444, 1.337940584860995319 ) ) ;
#27530 = CARTESIAN_POINT ( 'NONE',  ( 10.45888906141533603, 56.51500000000000057, -4.393716635382131308 ) ) ;
#27531 = CARTESIAN_POINT ( 'NONE',  ( -58.45963793110873041, -0.4469582673315134480, 0.3141006534902464620 ) ) ;
#27532 = CARTESIAN_POINT ( 'NONE',  ( -3.538659794179211726, -11.74154716455626257, -2.972011832598964176 ) ) ;
#27533 = CARTESIAN_POINT ( 'NONE',  ( 17.14717842969334072, 147.4900653055648547, 2.050122926623737740 ) ) ;
#27534 = CARTESIAN_POINT ( 'NONE',  ( 1.733480476724572172, 35.69352191795299944, 2.306000102516378991 ) ) ;
#27535 = CARTESIAN_POINT ( 'NONE',  ( -0.3401008104888438854, 105.9117620634264370, 5.317146732969808554 ) ) ;
#27536 = CARTESIAN_POINT ( 'NONE',  ( -1.544744425833544099, 4.816215111148435923, 4.377641278133862279 ) ) ;
#27537 = CARTESIAN_POINT ( 'NONE',  ( 9.075584820321502377, 124.0722828908287454, 0.2154388746608567884 ) ) ;
#27538 = CARTESIAN_POINT ( 'NONE',  ( -12.21488373879589062, 55.24499999999999034, 5.016499999999999737 ) ) ;
#27539 =( BOUNDED_SURFACE ( )  B_SPLINE_SURFACE ( 3, 2, ( 
 ( #8439, #25037, #21397 ),
 ( #20782, #34425, #14393 ),
 ( #37820, #8648, #18423 ),
 ( #40410, #2273, #15237 ) ),
 .UNSPECIFIED., .F., .F., .T. ) 
 B_SPLINE_SURFACE_WITH_KNOTS ( ( 4, 4 ),
 ( 3, 3 ),
 ( 5.204170427930421283E-18, 6.346505048318222639E-05 ),
 ( 0.000000000000000000, 1.000000000000000000 ),
 .UNSPECIFIED. ) 
 GEOMETRIC_REPRESENTATION_ITEM ( )  RATIONAL_B_SPLINE_SURFACE ( (
 ( 1.000000000000000000, 0.7071067811865614505, 1.000000000000000000),
 ( 1.000000000000000000, 0.7071067753522113364, 1.000000000000000000),
 ( 1.000000000000000000, 0.7071464246557911393, 1.000000000000000000),
 ( 1.000000000000000000, 0.7072256012392403868, 1.000000000000000000) ) ) 
 REPRESENTATION_ITEM ( '' )  SURFACE ( )  );
#27540 = CARTESIAN_POINT ( 'NONE',  ( -57.91458998086623922, 0.5482684225795314559, -0.1438514718893213751 ) ) ;
#27541 = CARTESIAN_POINT ( 'NONE',  ( -5.535853918629470627, 116.8115403336140474, -0.4677966508803286794 ) ) ;
#27542 = CARTESIAN_POINT ( 'NONE',  ( -10.18297664959815663, 77.66688486464208552, -1.269999999999998019 ) ) ;
#27543 = CYLINDRICAL_SURFACE ( 'NONE', #40425, 0.2539999999999937863 ) ;
#27544 = CARTESIAN_POINT ( 'NONE',  ( -0.3947539175594134142, 105.8842979884933726, 5.327223850753324719 ) ) ;
#27545 = DIRECTION ( 'NONE',  ( -0.8745520943968229099, 0.4849315768086570055, -5.361993529360569999E-16 ) ) ;
#27546 = CARTESIAN_POINT ( 'NONE',  ( -7.218840658378264052, 2.017470825009220370, -4.342437029863850384 ) ) ;
#27547 = CARTESIAN_POINT ( 'NONE',  ( -17.14499999999999957, 71.11999999999999034, 5.016499999999999737 ) ) ;
#27548 = CARTESIAN_POINT ( 'NONE',  ( -7.772068811996249771, 69.25462295839062676, 1.270000000000003570 ) ) ;
#27549 = CARTESIAN_POINT ( 'NONE',  ( 5.137966006445083167, 56.84472104120887082, -5.330653870689105567 ) ) ;
#27550 = CARTESIAN_POINT ( 'NONE',  ( 0.007670926888197925585, 121.5961256765098284, -0.3838845493045227597 ) ) ;
#27551 = CARTESIAN_POINT ( 'NONE',  ( -0.004355829920665829462, 116.7171338949676738, 0.2179835409713599403 ) ) ;
#27552 = ORIENTED_EDGE ( 'NONE', *, *, #11339, .T. ) ;
#27553 = DIRECTION ( 'NONE',  ( 5.188838149069472160E-16, -1.699382548006136559E-16, -1.000000000000000000 ) ) ;
#27554 = ORIENTED_EDGE ( 'NONE', *, *, #27271, .F. ) ;
#27555 = CARTESIAN_POINT ( 'NONE',  ( -47.59852559864132360, 19.66225068540624932, -5.176489187672372871 ) ) ;
#27556 = CARTESIAN_POINT ( 'NONE',  ( -1.561582345843753217, 156.2588034088681184, -0.03120413162939504950 ) ) ;
#27557 = CARTESIAN_POINT ( 'NONE',  ( 4.692294315076144251, -14.85586321182354119, 4.526698459197877611 ) ) ;
#27558 = CARTESIAN_POINT ( 'NONE',  ( -20.41374081727979473, 149.7738053052645171, 1.564883410832889510 ) ) ;
#27559 = CARTESIAN_POINT ( 'NONE',  ( 5.868821994818586241, 117.5931221156369730, -0.5844160582045566654 ) ) ;
#27560 = CARTESIAN_POINT ( 'NONE',  ( -4.374560056058969693, 13.03735028915297534, 1.504755201125916875 ) ) ;
#27561 = CARTESIAN_POINT ( 'NONE',  ( -22.58551839157542318, 137.2245694613254443, -0.7673259740012311481 ) ) ;
#27562 = CARTESIAN_POINT ( 'NONE',  ( -49.41583470348051321, 17.21070444274963762, -5.043540371747944562 ) ) ;
#27563 = CARTESIAN_POINT ( 'NONE',  ( 6.059261036834406866, 56.98375738874754859, 5.016500000000000625 ) ) ;
#27564 = CARTESIAN_POINT ( 'NONE',  ( -12.79346581414816697, 125.9836878220586556, 1.262672879670394321 ) ) ;
#27565 = CARTESIAN_POINT ( 'NONE',  ( -48.75754203680085652, 18.15534081570707414, -5.116688472081215799 ) ) ;
#27566 = CARTESIAN_POINT ( 'NONE',  ( 11.96109417309357958, 154.9039014673913073, -1.746238851223627764 ) ) ;
#27567 = CARTESIAN_POINT ( 'NONE',  ( -21.49578583461358150, 148.6087350971780836, -2.244132633923697107 ) ) ;
#27568 = CARTESIAN_POINT ( 'NONE',  ( -45.91718695868514288, 25.22619731686664224, -1.578102078770073469 ) ) ;
#27569 = CARTESIAN_POINT ( 'NONE',  ( 12.09414715658290085, 128.3964238929853252, -0.7197952935306336508 ) ) ;
#27570 = AXIS2_PLACEMENT_3D ( 'NONE', #22965, #35576, #13405 ) ;
#27571 = ORIENTED_EDGE ( 'NONE', *, *, #20655, .F. ) ;
#27572 = CARTESIAN_POINT ( 'NONE',  ( -9.271712722858243438, 121.5662863950884400, -1.459403803239323505 ) ) ;
#27573 = CARTESIAN_POINT ( 'NONE',  ( 1.925067723532086994, -15.61332249492565438, 5.452854070638914585 ) ) ;
#27574 = CARTESIAN_POINT ( 'NONE',  ( -4.495574403056286528, 118.0850938064217246, -0.7939362711117921023 ) ) ;
#27575 = CARTESIAN_POINT ( 'NONE',  ( -47.84356795211461844, 19.38525671449500010, -5.197506975155170572 ) ) ;
#27576 = CARTESIAN_POINT ( 'NONE',  ( -5.006118277528749161, 117.4009255802263283, 0.7893014723888780448 ) ) ;
#27577 = CARTESIAN_POINT ( 'NONE',  ( 18.07470265256048236, 147.5382818419693649, 2.342107984669389964 ) ) ;
#27578 = DIRECTION ( 'NONE',  ( -0.8745520943968235761, 0.4849315768086558398, 0.000000000000000000 ) ) ;
#27579 = CARTESIAN_POINT ( 'NONE',  ( 22.66443576792679693, 150.6395781703034231, 0.4273611094724397153 ) ) ;
#27580 = CARTESIAN_POINT ( 'NONE',  ( -3.946719713907086202, 4.502433826932805694, 7.497755479828382086 ) ) ;
#27581 = CARTESIAN_POINT ( 'NONE',  ( 14.42924251737974473, 139.0941462050048187, 0.8894241721302194037 ) ) ;
#27582 = CARTESIAN_POINT ( 'NONE',  ( -58.33777482027510786, 1.113448835244251756, -1.208045587469442017 ) ) ;
#27583 = CARTESIAN_POINT ( 'NONE',  ( -42.12253153191133492, 21.94389511927448311, -6.431429377749453771E-15 ) ) ;
#27584 = CARTESIAN_POINT ( 'NONE',  ( 4.522962677521610964, 110.7917694958216401, -2.894362350303244291 ) ) ;
#27585 = CARTESIAN_POINT ( 'NONE',  ( 4.336254965884680068, 118.7629491485453741, 1.056156474602399697 ) ) ;
#27586 = CARTESIAN_POINT ( 'NONE',  ( -57.34787435976332404, 1.552391619547691004, -9.959991576465148270E-15 ) ) ;
#27587 = CARTESIAN_POINT ( 'NONE',  ( -17.22554230343062542, 122.7389118244895769, -0.2345756144184561187 ) ) ;
#27588 = VERTEX_POINT ( 'NONE', #36906 ) ;
#27589 = CARTESIAN_POINT ( 'NONE',  ( -47.30609498763488574, 23.90227454495589399, -2.251708124038050762 ) ) ;
#27590 = CARTESIAN_POINT ( 'NONE',  ( 6.883184783311018684, 121.6011013064247379, -0.4353592733600721854 ) ) ;
#27591 = CARTESIAN_POINT ( 'NONE',  ( -8.330184522151240500, 120.0920323058250858, 1.118340454250549731 ) ) ;
#27592 = EDGE_LOOP ( 'NONE', ( #4420, #14411, #39200, #10052, #248, #23789, #20799, #24644 ) ) ;
#27593 = CARTESIAN_POINT ( 'NONE',  ( 0.2141205576264084698, 115.7030700283022782, -1.756908841275494293 ) ) ;
#27594 = CARTESIAN_POINT ( 'NONE',  ( -14.27613791431603119, 138.9852717218771261, -0.6171993629658318881 ) ) ;
#27595 = CARTESIAN_POINT ( 'NONE',  ( 4.648743876849892764, -12.57259931633604388, 2.147031799546866182 ) ) ;
#27596 = CARTESIAN_POINT ( 'NONE',  ( -9.838452836889556963, 157.5983698538113629, 1.280564089889915769 ) ) ;
#27597 = CARTESIAN_POINT ( 'NONE',  ( 5.632494751982964232, 78.90911215162449821, -5.063853515469283195 ) ) ;
#27598 = CARTESIAN_POINT ( 'NONE',  ( 15.65298122355231492, 120.8241032224722176, 0.4173319239378796008 ) ) ;
#27599 = CARTESIAN_POINT ( 'NONE',  ( 10.13917656308076864, 125.9557277354818012, 0.2514634351610266494 ) ) ;
#27600 = ORIENTED_EDGE ( 'NONE', *, *, #31869, .T. ) ;
#27601 = CARTESIAN_POINT ( 'NONE',  ( 0.9679928046509989059, 27.93285725408814812, -0.1178628334679577422 ) ) ;
#27602 = EDGE_CURVE ( 'NONE', #6891, #26236, #16084, .T. ) ;
#27603 = CARTESIAN_POINT ( 'NONE',  ( -8.216553068272286708, 117.5004391570743394, -0.1790601237764437026 ) ) ;
#27604 = CARTESIAN_POINT ( 'NONE',  ( -46.04356002888985699, 20.98312591567169605, -4.505114092170838802 ) ) ;
#27605 = ORIENTED_EDGE ( 'NONE', *, *, #6035, .T. ) ;
#27606 = CARTESIAN_POINT ( 'NONE',  ( -7.461250000000054783, 85.80437499999999318, 9.137395930138188390E-16 ) ) ;
#27607 = EDGE_LOOP ( 'NONE', ( #11401, #20586, #36412, #8259, #39507, #7419, #1386, #42031, #41959 ) ) ;
#27608 = CARTESIAN_POINT ( 'NONE',  ( -8.455225958726231283, 119.4764566065096005, 1.058818690914600458 ) ) ;
#27609 = CARTESIAN_POINT ( 'NONE',  ( -3.074427775304182209, -11.96646105551300465, -3.469969274305642060 ) ) ;
#27610 = CARTESIAN_POINT ( 'NONE',  ( 18.58655447097567404, 128.6297099747515347, 1.738804191113343833 ) ) ;
#27611 = CARTESIAN_POINT ( 'NONE',  ( -58.22800107109949153, 0.01111325675459684525, -0.5047451677696692673 ) ) ;
#27612 = CARTESIAN_POINT ( 'NONE',  ( 1.201082828432564087, 118.2527139659984101, -0.6198154079389066595 ) ) ;
#27613 = CARTESIAN_POINT ( 'NONE',  ( 7.984751813625430295, 22.47881364768745271, 2.830840501157275924 ) ) ;
#27614 = CARTESIAN_POINT ( 'NONE',  ( -21.78097984573151535, 150.5404744109896171, -1.730106343981699268 ) ) ;
#27615 = CARTESIAN_POINT ( 'NONE',  ( 4.852265073632695547, 117.6441343497408667, -0.9100757317102342592 ) ) ;
#27616 = VERTEX_POINT ( 'NONE', #3912 ) ;
#27617 = CARTESIAN_POINT ( 'NONE',  ( -0.001786757842276731579, 120.9379535345006076, 0.08941666878750659242 ) ) ;
#27618 = CARTESIAN_POINT ( 'NONE',  ( 4.283822907657564016, -15.48171044555848930, 4.591852530049981063 ) ) ;
#27619 = FACE_OUTER_BOUND ( 'NONE', #11797, .T. ) ;
#27620 = CARTESIAN_POINT ( 'NONE',  ( -0.5436877124052815757, 117.9496053982743149, -1.405509504246643004 ) ) ;
#27622 = ORIENTED_EDGE ( 'NONE', *, *, #16629, .F. ) ;
#27621 = AXIS2_PLACEMENT_3D ( 'NONE', #11315, #40100, #24302 ) ;
#27623 = CARTESIAN_POINT ( 'NONE',  ( 17.96932707993145328, 150.0321773811041339, 2.460285709456810466 ) ) ;
#27624 = DIRECTION ( 'NONE',  ( -5.206863593109713661E-17, 1.000000000000000000, -1.077750396879097183E-30 ) ) ;
#27625 = CARTESIAN_POINT ( 'NONE',  ( 4.752069321396074741, 117.6028811792687350, 1.174454948735748294 ) ) ;
#27626 = CARTESIAN_POINT ( 'NONE',  ( -1.272828668259226248, 111.9985432423065959, 2.911558293332169534 ) ) ;
#27628 = ADVANCED_FACE ( 'NONE', ( #4331 ), #39470, .F. ) ;
#27627 = CARTESIAN_POINT ( 'NONE',  ( 8.241158353334730791, 13.74789577914289929, -1.876134369653635448 ) ) ;
#27629 = CARTESIAN_POINT ( 'NONE',  ( 0.7026863962999440050, 156.4221767039705071, 0.7130674712139345450 ) ) ;
#27630 = CARTESIAN_POINT ( 'NONE',  ( -5.240514789080909175, 115.6909491485453003, -1.019557571888159098 ) ) ;
#27631 = CARTESIAN_POINT ( 'NONE',  ( 5.638719538426313349, 159.1014311945586712, -0.3820744581509933346 ) ) ;
#27632 = CARTESIAN_POINT ( 'NONE',  ( -12.21488373879589240, 12.96416000000000146, -4.381499999999999950 ) ) ;
#27633 = CARTESIAN_POINT ( 'NONE',  ( -53.65068779629728368, 9.511520785580891868, 3.604358613835281222 ) ) ;
#27634 = CARTESIAN_POINT ( 'NONE',  ( -50.92299000722575641, 14.78308106450686310, 4.710654750704142302 ) ) ;
#27635 = CARTESIAN_POINT ( 'NONE',  ( -7.961576494521615643, 72.55615504727386167, 1.270000000000003126 ) ) ;
#27636 = CARTESIAN_POINT ( 'NONE',  ( -4.252766745286226779, 118.2250244251308828, 0.3074143273816778987 ) ) ;
#27637 = CARTESIAN_POINT ( 'NONE',  ( 2.352955416729489713, 107.1115117626462450, -4.697798642113138357 ) ) ;
#27638 = ORIENTED_EDGE ( 'NONE', *, *, #26154, .F. ) ;
#27639 = CARTESIAN_POINT ( 'NONE',  ( -48.21404017327530767, 19.06235592689615288, 5.351320745402585288 ) ) ;
#27640 = CARTESIAN_POINT ( 'NONE',  ( 6.241659769608493669, 119.7361415367193587, -0.9904423240702238118 ) ) ;
#27641 = CARTESIAN_POINT ( 'NONE',  ( -5.402623002109140593, 117.1681999988027911, -0.9004238350613810171 ) ) ;
#27642 = CARTESIAN_POINT ( 'NONE',  ( 4.274869760779545835, 118.2142274725316753, 0.5231722506238379866 ) ) ;
#27643 = CARTESIAN_POINT ( 'NONE',  ( -1.656170893582116443, 156.3096136994911092, -0.5768031348127031777 ) ) ;
#27644 = DIRECTION ( 'NONE',  ( 1.224646799147353207E-16, -1.179012811983454535E-32, 1.000000000000000000 ) ) ;
#27645 = DIRECTION ( 'NONE',  ( -0.5149185422762211362, 0.8572391118119444542, 0.000000000000000000 ) ) ;
#27646 = AXIS2_PLACEMENT_3D ( 'NONE', #31059, #14650, #27654 ) ;
#27647 = EDGE_CURVE ( 'NONE', #27588, #17493, #10966, .T. ) ;
#27648 = VERTEX_POINT ( 'NONE', #17296 ) ;
#27649 = CARTESIAN_POINT ( 'NONE',  ( 1.580769961479467911, 28.79261460129497863, -4.363931058323818668 ) ) ;
#27650 = CARTESIAN_POINT ( 'NONE',  ( -0.5640265924887369886, 120.2131932824006526, -0.4111470527632632987 ) ) ;
#27651 = DIRECTION ( 'NONE',  ( -5.188838149069471174E-16, 1.699382548006136313E-16, 1.000000000000000000 ) ) ;
#27652 = CARTESIAN_POINT ( 'NONE',  ( -46.78477525497864775, 20.40172935490961237, 4.969468548369063932 ) ) ;
#27653 = AXIS2_PLACEMENT_3D ( 'NONE', #38495, #35299, #6127 ) ;
#27654 = DIRECTION ( 'NONE',  ( -1.000000000000000000, 0.000000000000000000, 0.000000000000000000 ) ) ;
#27655 = CARTESIAN_POINT ( 'NONE',  ( 6.997804181779785360, 121.9551933346753714, 0.1784859520612882000 ) ) ;
#27656 = DIRECTION ( 'NONE',  ( 0.9998004120163608288, 0.000000000000000000, 0.01997839162482760791 ) ) ;
#27657 = CARTESIAN_POINT ( 'NONE',  ( 21.41027608214055888, 151.3201912522522719, 1.490379992046950264 ) ) ;
#27658 = CARTESIAN_POINT ( 'NONE',  ( -6.650126595083637682, 78.47834120613788400, -1.523999999999996691 ) ) ;
#27660 = CARTESIAN_POINT ( 'NONE',  ( 7.920278096381447419, 118.7344292658239340, -0.9023208588851655554 ) ) ;
#27659 = CARTESIAN_POINT ( 'NONE',  ( 3.130567944924658175, -14.75736435017342707, 3.480214150758962788 ) ) ;
#27661 = CARTESIAN_POINT ( 'NONE',  ( -18.67487979129062481, 147.7499600834086948, 1.698815563122507921 ) ) ;
#27662 = CARTESIAN_POINT ( 'NONE',  ( -3.990024091077861268, 18.91925256873344807, 2.329872802929966902 ) ) ;
#27663 = CARTESIAN_POINT ( 'NONE',  ( -5.825324126169852512, 117.1711376449269721, -0.5405197603966793718 ) ) ;
#27664 = CARTESIAN_POINT ( 'NONE',  ( -0.4796499176084361160, 15.67505972103439049, -0.8497018901732851237 ) ) ;
#27665 = ORIENTED_EDGE ( 'NONE', *, *, #23477, .T. ) ;
#27666 = EDGE_CURVE ( 'NONE', #39243, #41261, #18433, .T. ) ;
#27667 = CARTESIAN_POINT ( 'NONE',  ( -52.76126113563441322, 10.11686208896574257, 1.835409310531171956 ) ) ;
#27668 = CARTESIAN_POINT ( 'NONE',  ( -9.597885446028771028, 124.1734284925964573, 0.3307417288639282194 ) ) ;
#27669 = CARTESIAN_POINT ( 'NONE',  ( 4.828046317437772572, -12.99562652935115636, 2.825559498992329832 ) ) ;
#27670 = CARTESIAN_POINT ( 'NONE',  ( 10.26617122093349543, 123.0849000269954701, -0.9769925898671677489 ) ) ;
#27671 = VERTEX_POINT ( 'NONE', #40104 ) ;
#27672 = CIRCLE ( 'NONE', #20176, 0.2539999999999997260 ) ;
#27673 = CARTESIAN_POINT ( 'NONE',  ( 2.395182152955315225, 115.7029496081253512, 1.700632368870516276 ) ) ;
#27674 = CARTESIAN_POINT ( 'NONE',  ( 3.191397606779386109, -14.26579101578730224, 3.890870127686782087 ) ) ;
#27675 = CARTESIAN_POINT ( 'NONE',  ( -4.698701480185317969, 117.8441750417280076, -1.023598512841458863 ) ) ;
#27676 = CARTESIAN_POINT ( 'NONE',  ( 11.90298433346883300, 130.3805625696445816, 0.1299774887382024458 ) ) ;
#27677 = ORIENTED_EDGE ( 'NONE', *, *, #16295, .F. ) ;
#27678 = CARTESIAN_POINT ( 'NONE',  ( 0.4261125263669181540, 118.2558431149878402, 0.5943921922486902210 ) ) ;
#27679 = CARTESIAN_POINT ( 'NONE',  ( -5.305748947172282293, 57.14999999999999147, 5.247078976224250013 ) ) ;
#27680 = AXIS2_PLACEMENT_3D ( 'NONE', #26796, #21421, #15469 ) ;
#27681 = CARTESIAN_POINT ( 'NONE',  ( -15.47023807670837314, 120.6682698389898434, -0.3091321738930619678 ) ) ;
#27682 = EDGE_CURVE ( 'NONE', #11667, #6467, #34417, .T. ) ;
#27683 = CARTESIAN_POINT ( 'NONE',  ( 0.01133107913638299775, 156.3792106723807649, -0.5670535347366656431 ) ) ;
#27684 = CIRCLE ( 'NONE', #20860, 0.5080000000000002292 ) ;
#27685 = CARTESIAN_POINT ( 'NONE',  ( 20.30088961563504313, 128.9598305440861452, 0.1271185223121274743 ) ) ;
#27686 = EDGE_CURVE ( 'NONE', #12622, #20165, #17138, .T. ) ;
#27687 = LINE ( 'NONE', #37278, #29531 ) ;
#27688 = EDGE_CURVE ( 'NONE', #18509, #31875, #27928, .T. ) ;
#27689 = CARTESIAN_POINT ( 'NONE',  ( 2.055526052377715462, -15.16505444338715769, 5.893956344503145317 ) ) ;
#27690 = CARTESIAN_POINT ( 'NONE',  ( 10.28897677580357950, 56.51500000000000057, 5.016500000000000625 ) ) ;
#27691 = CARTESIAN_POINT ( 'NONE',  ( -4.858498820925455597, 117.7576908667619620, -0.8801082217429874177 ) ) ;
#27692 = CARTESIAN_POINT ( 'NONE',  ( -4.798162323025271903, 117.8843545273942794, 0.6935535454817384204 ) ) ;
#27693 = ORIENTED_EDGE ( 'NONE', *, *, #35169, .F. ) ;
#27694 = LINE ( 'NONE', #12136, #37694 ) ;
#27695 = CARTESIAN_POINT ( 'NONE',  ( 2.899848536121923281, 118.0059886663794231, -0.7391867022396521048 ) ) ;
#27696 = CARTESIAN_POINT ( 'NONE',  ( -1.040151681621160229, 108.5039085404744981, -4.268591994808179635 ) ) ;
#27697 = CARTESIAN_POINT ( 'NONE',  ( 4.931585812799779589, 117.5375468106932431, 1.014273347241211320 ) ) ;
#27698 = CARTESIAN_POINT ( 'NONE',  ( -12.69999999999999574, 17.14499999999999957, 0.000000000000000000 ) ) ;
#27699 = CARTESIAN_POINT ( 'NONE',  ( -0.3790891741045420149, 120.5507043431651510, 0.5490176968301536675 ) ) ;
#27700 = AXIS2_PLACEMENT_3D ( 'NONE', #29287, #32279, #25253 ) ;
#27701 = CARTESIAN_POINT ( 'NONE',  ( 1.719524320724281852, 5.915668354077112667, 4.300554535892874064 ) ) ;
#27702 = CARTESIAN_POINT ( 'NONE',  ( 4.801216665947148243, 117.4032681888235459, -1.015537427445656782 ) ) ;
#27703 = CARTESIAN_POINT ( 'NONE',  ( -0.1690072757122455804, 105.7852416022782478, -5.338485453081204035 ) ) ;
#27704 = CARTESIAN_POINT ( 'NONE',  ( 1.858891552337619935, -15.10179129218686178, 5.555419934288654993 ) ) ;
#27705 = CARTESIAN_POINT ( 'NONE',  ( 5.239677827970672830, 116.1170857923940787, -1.027392938984838633 ) ) ;
#27706 = DIRECTION ( 'NONE',  ( -4.017660918040594346E-17, 1.000000000000000000, 2.376309959284834438E-19 ) ) ;
#27707 = CARTESIAN_POINT ( 'NONE',  ( -2.051794397732527475, 115.7029490351849006, 1.635858944951805061 ) ) ;
#27708 = CARTESIAN_POINT ( 'NONE',  ( -0.6244342276652131707, 19.93415720681881353, -4.586363120317934694 ) ) ;
#27709 = ORIENTED_EDGE ( 'NONE', *, *, #12647, .T. ) ;
#27710 = CARTESIAN_POINT ( 'NONE',  ( -4.305676042947723658, 104.6144662015411626, -3.167619746371888034 ) ) ;
#27711 = CARTESIAN_POINT ( 'NONE',  ( 4.538337246427208704, -15.41107556132688394, 0.6303774773485874006 ) ) ;
#27712 = CARTESIAN_POINT ( 'NONE',  ( -2.330377461923392346, 118.7486697826011977, 0.7097125967482104114 ) ) ;
#27713 = CARTESIAN_POINT ( 'NONE',  ( -0.7839530942921373313, 14.33508526448824760, 0.5845576647881698396 ) ) ;
#27714 = ORIENTED_EDGE ( 'NONE', *, *, #23309, .F. ) ;
#27715 = ORIENTED_EDGE ( 'NONE', *, *, #41253, .T. ) ;
#27716 = AXIS2_PLACEMENT_3D ( 'NONE', #37709, #21288, #1735 ) ;
#27717 = CARTESIAN_POINT ( 'NONE',  ( 4.014846287426770743, 122.0441497943765370, 0.2789485273175661972 ) ) ;
#27718 = CARTESIAN_POINT ( 'NONE',  ( -0.5902664527120891069, 120.3589971203204669, 0.3461335206401335851 ) ) ;
#27719 = CYLINDRICAL_SURFACE ( 'NONE', #41601, 0.2540000000000012248 ) ;
#27720 = CARTESIAN_POINT ( 'NONE',  ( 4.638991104174423619, 118.0227226582861420, -0.6551358822890929190 ) ) ;
#27721 = CARTESIAN_POINT ( 'NONE',  ( 0.01051219832175660264, 119.4384375980492194, -0.5260733902271049756 ) ) ;
#27722 = CARTESIAN_POINT ( 'NONE',  ( -19.76635024033938137, 141.2215177107240436, -2.477633452034130990 ) ) ;
#27723 = DIRECTION ( 'NONE',  ( 0.1715592850456333085, 0.1224830539174543292, 0.9775302108976914317 ) ) ;
#27724 = CARTESIAN_POINT ( 'NONE',  ( 4.282392886588548997, 118.2128385315536860, -0.3623839240741059675 ) ) ;
#27725 = CARTESIAN_POINT ( 'NONE',  ( 15.52187087609520688, 147.8629129908177049, -0.2796426011346633822 ) ) ;
#27726 = EDGE_CURVE ( 'NONE', #700, #18659, #17095, .T. ) ;
#27727 = VERTEX_POINT ( 'NONE', #31127 ) ;
#27728 = CARTESIAN_POINT ( 'NONE',  ( 2.769760999665409340, -14.92388480464812872, 4.423285184949336646 ) ) ;
#27729 = CARTESIAN_POINT ( 'NONE',  ( -4.922306677375791750, 117.4109580117980016, 0.9480543157666212473 ) ) ;
#27730 = CIRCLE ( 'NONE', #29097, 0.6350000000000014522 ) ;
#27731 = CARTESIAN_POINT ( 'NONE',  ( -48.16232371144223379, 19.02200717994684354, 5.227009030889012031 ) ) ;
#27732 = CARTESIAN_POINT ( 'NONE',  ( -2.329872802932658082, -2.670747431267189498, -3.990024091085845548 ) ) ;
#27733 = CARTESIAN_POINT ( 'NONE',  ( 10.24488040547488943, 123.7737839053064022, 1.229789271442949694 ) ) ;
#27734 = CARTESIAN_POINT ( 'NONE',  ( -3.732951360862769352, 28.31137488888144915, 1.178986259223461230 ) ) ;
#27735 = CARTESIAN_POINT ( 'NONE',  ( -3.706399805698186167, 113.7286232773062125, 2.153009399082070452 ) ) ;
#27736 = EDGE_CURVE ( 'NONE', #13530, #39307, #27954, .T. ) ;
#27737 = CARTESIAN_POINT ( 'NONE',  ( -2.424025297795170619, -5.104216246930970868, 3.935102955759355758 ) ) ;
#27738 = CARTESIAN_POINT ( 'NONE',  ( 15.52804360843196463, 147.5314071815517138, 0.4383331365498630561 ) ) ;
#27739 = ADVANCED_FACE ( 'NONE', ( #21516 ), #27719, .T. ) ;
#27740 = CARTESIAN_POINT ( 'NONE',  ( 1.329249052905784323, 1.652534479431654546, 8.327223686629459110 ) ) ;
#27741 = CARTESIAN_POINT ( 'NONE',  ( -57.47393550255003447, 1.325481720219581661, -1.020368242535414227E-14 ) ) ;
#27742 = CARTESIAN_POINT ( 'NONE',  ( -8.759430686813598044, 117.8325680729238343, -0.5873362267662896041 ) ) ;
#27743 = DIRECTION ( 'NONE',  ( 1.000000000000000000, 0.000000000000000000, 0.000000000000000000 ) ) ;
#27744 = FACE_OUTER_BOUND ( 'NONE', #24482, .T. ) ;
#27745 = CARTESIAN_POINT ( 'NONE',  ( 2.047221892555402434, -15.65848914036231676, 5.808978358897259220 ) ) ;
#27746 = DIRECTION ( 'NONE',  ( -5.188838149069472160E-16, 1.699382548006136559E-16, 1.000000000000000000 ) ) ;
#27747 = CARTESIAN_POINT ( 'NONE',  ( 7.690436415270363923, 8.290658626076512050, -3.468142284020285793 ) ) ;
#27748 = FACE_OUTER_BOUND ( 'NONE', #9176, .T. ) ;
#27749 = CARTESIAN_POINT ( 'NONE',  ( -14.73199999999999754, 61.59499999999999886, 5.016499999999999737 ) ) ;
#27750 = CARTESIAN_POINT ( 'NONE',  ( -46.60530155212505576, 26.17382724835474406, -1.270000000000008233 ) ) ;
#27751 = CARTESIAN_POINT ( 'NONE',  ( 0.1065646865914870178, 105.8844662015456919, -5.332932678536313809 ) ) ;
#27752 = CARTESIAN_POINT ( 'NONE',  ( -6.918545264603769063, 117.3320596397172721, 0.2494728033470791639 ) ) ;
#27753 = VERTEX_POINT ( 'NONE', #4954 ) ;
#27754 = CARTESIAN_POINT ( 'NONE',  ( -41.09670346151854403, 23.04688172093030829, -1.270085369932534958 ) ) ;
#27755 = EDGE_LOOP ( 'NONE', ( #1511, #32509, #9026, #31320, #2547, #29834, #12238 ) ) ;
#27756 = CARTESIAN_POINT ( 'NONE',  ( -43.33782384754901074, 21.60941887712242959, -2.445739413454641742 ) ) ;
#27757 = CARTESIAN_POINT ( 'NONE',  ( -15.26262975079004569, 148.0175730704188481, -0.3049836654608575892 ) ) ;
#27758 = CARTESIAN_POINT ( 'NONE',  ( 5.218378134725943696, -15.03467804911627681, 3.623131781705042354 ) ) ;
#27759 = CARTESIAN_POINT ( 'NONE',  ( -1.179722549733782877, 118.0995038195805904, 0.6028833020595597558 ) ) ;
#27760 = MECHANICAL_DESIGN_GEOMETRIC_PRESENTATION_REPRESENTATION (  '', ( #4650 ), #18228 ) ;
#27761 = CARTESIAN_POINT ( 'NONE',  ( 14.41840636618835880, 121.0470547900126519, -0.7241072410554124650 ) ) ;
#27762 = CARTESIAN_POINT ( 'NONE',  ( -4.563195415240126174, 21.88328375387019165, -0.7336086519975816289 ) ) ;
#27763 = CARTESIAN_POINT ( 'NONE',  ( -13.50792085693146838, 119.6474162840860771, -0.5731308571144441144 ) ) ;
#27764 = CARTESIAN_POINT ( 'NONE',  ( -49.77363268278942598, 16.65469053158889068, -4.972382134799542719 ) ) ;
#27765 = VERTEX_POINT ( 'NONE', #20897 ) ;
#27766 = CARTESIAN_POINT ( 'NONE',  ( 2.183922297081623665, 116.1979336525763671, 0.06695608452006818201 ) ) ;
#27767 = CARTESIAN_POINT ( 'NONE',  ( 5.941785709847694719, 56.51500000000406487, 5.016499812911857425 ) ) ;
#27768 = CARTESIAN_POINT ( 'NONE',  ( -17.81417655509816456, 146.7645792007554633, 1.532459167469646610 ) ) ;
#27769 = CARTESIAN_POINT ( 'NONE',  ( -5.078986093043185157, 69.43546620154572224, -0.1014902294541231847 ) ) ;
#27770 = CARTESIAN_POINT ( 'NONE',  ( 0.01147819631899514234, 118.8623374019222894, -0.5744158801423951966 ) ) ;
#27771 = CARTESIAN_POINT ( 'NONE',  ( 0.01023305610364720099, 117.8848902025789158, -0.5121039721716186266 ) ) ;
#27772 = CARTESIAN_POINT ( 'NONE',  ( -51.54051843738712080, 14.84038450301108192, -4.692172599169433411 ) ) ;
#27773 = CARTESIAN_POINT ( 'NONE',  ( 3.602148172789689795, 120.6468399921648711, -0.3585086490597836906 ) ) ;
#27774 = ORIENTED_EDGE ( 'NONE', *, *, #14708, .T. ) ;
#27775 = CARTESIAN_POINT ( 'NONE',  ( -14.16178827078164026, 152.6618899727951089, -2.241469232429742942 ) ) ;
#27776 = CARTESIAN_POINT ( 'NONE',  ( 3.297442402085044133, -15.64565814434701352, 4.209479195861737466 ) ) ;
#27777 = CARTESIAN_POINT ( 'NONE',  ( -4.390462178403575777, 118.1641434913643138, -0.6590699376955369004 ) ) ;
#27778 = CARTESIAN_POINT ( 'NONE',  ( -57.66338803320029882, 2.692357263605615891, -1.869785753600856637 ) ) ;
#27779 = DIRECTION ( 'NONE',  ( -0.9998004120163608288, 0.000000000000000000, -0.01997839162482747608 ) ) ;
#27780 = CARTESIAN_POINT ( 'NONE',  ( 11.17842967653866459, 122.9575399027323073, 1.639653439019827408 ) ) ;
#27781 = DIRECTION ( 'NONE',  ( 4.017660918040594346E-17, -1.000000000000000000, -2.376309959284834438E-19 ) ) ;
#27782 = EDGE_CURVE ( 'NONE', #11710, #117, #34782, .T. ) ;
#27783 =( BOUNDED_SURFACE ( )  B_SPLINE_SURFACE ( 3, 2, ( 
 ( #30207, #14999, #33210 ),
 ( #835, #11392, #36613 ),
 ( #1047, #7432, #18190 ),
 ( #11814, #29791, #24378 ),
 ( #26808, #39816, #37385 ),
 ( #33415, #21172, #34203 ),
 ( #37590, #5029, #17986 ),
 ( #1825, #11600, #24584 ),
 ( #8417, #21376, #34402 ),
 ( #5236, #31409, #18401 ),
 ( #2671, #34828, #5661 ),
 ( #5866, #31624, #32258 ),
 ( #35045, #15212, #12863 ),
 ( #35454, #15630, #25647 ),
 ( #18618, #41221, #9051 ),
 ( #2462, #8838, #3087 ),
 ( #2250, #28633, #25447 ),
 ( #6073, #22220, #21800 ),
 ( #41646, #29049, #12239 ),
 ( #19035, #15425, #16046 ) ),
 .UNSPECIFIED., .F., .F., .F. ) 
 B_SPLINE_SURFACE_WITH_KNOTS ( ( 4, 2, 2, 2, 2, 2, 2, 2, 2, 4 ),
 ( 3, 3 ),
 ( -2.835792020584096599E-05, 0.001133685587513493529, 0.001714707341373160852, 0.002295729095232827959, 0.003457772602952162606, 0.003748283479881996377, 0.004038794356811830147, 0.004184049795276746815, 0.004329305233741663483, 0.004619816110671496820 ),
 ( 0.000000000000000000, 0.7006144518607101412 ),
 .UNSPECIFIED. ) 
 GEOMETRIC_REPRESENTATION_ITEM ( )  RATIONAL_B_SPLINE_SURFACE ( (
 ( 1.000000000000000000, 0.8321369569203693750, 0.8994884616705510760),
 ( 1.000000000000000000, 0.8321369569203693750, 0.8994884616705510760),
 ( 1.000000000000000000, 0.8321370030818711072, 0.8994884893107240043),
 ( 1.000000000000000000, 0.8321369330536090292, 0.8994884473798248070),
 ( 1.000000000000000000, 0.8321364034739958671, 0.8994881302828594549),
 ( 1.000000000000000000, 0.8321364926397946116, 0.8994881836727623980),
 ( 1.000000000000000000, 0.8321369244513672214, 0.8994884422290512216),
 ( 1.000000000000000000, 0.8321370276008952516, 0.8994885039920070824),
 ( 1.000000000000000000, 0.8321369665538331795, 0.8994884674387908507),
 ( 1.000000000000000000, 0.8321369547486586749, 0.8994884603701935877),
 ( 1.000000000000000000, 0.8321369676810204119, 0.8994884681137178539),
 ( 1.000000000000000000, 0.8321369492625183550, 0.8994884570852512695),
 ( 1.000000000000000000, 0.8321371141846684027, 0.8994885558358678423),
 ( 1.000000000000000000, 0.8321369149363557760, 0.8994884365317372676),
 ( 1.000000000000000000, 0.8321367296521178236, 0.8994883255888910245),
 ( 1.000000000000000000, 0.8321365983280889500, 0.8994882469558581617),
 ( 1.000000000000000000, 0.8321368728221703037, 0.8994884113149801408),
 ( 1.000000000000000000, 0.8321370919515077569, 0.8994885425232939102),
 ( 1.000000000000000000, 0.8321369569197746285, 0.8994884616701950275),
 ( 1.000000000000000000, 0.8321369569197746285, 0.8994884616701950275) ) ) 
 REPRESENTATION_ITEM ( '' )  SURFACE ( )  );
#27784 = EDGE_CURVE ( 'NONE', #28134, #40785, #4748, .T. ) ;
#27785 = CARTESIAN_POINT ( 'NONE',  ( -6.690270197923770645, -5.753818539685515709, 5.116497609988504891 ) ) ;
#27786 = CARTESIAN_POINT ( 'NONE',  ( 10.53234188159470897, 153.0603347025997323, 0.7465333597200856097 ) ) ;
#27787 = LINE ( 'NONE', #28424, #7242 ) ;
#27788 = TOROIDAL_SURFACE ( 'NONE', #34612, 8.794749999999998735, 0.2540000000000000036 ) ;
#27790 = ORIENTED_EDGE ( 'NONE', *, *, #5496, .F. ) ;
#27789 = CARTESIAN_POINT ( 'NONE',  ( -43.13073682054402269, 20.84535665847938546, -6.630667737810475277E-15 ) ) ;
#27791 = CARTESIAN_POINT ( 'NONE',  ( 0.6578851187915285559, 105.8204382098766700, -5.299257009308196764 ) ) ;
#27792 = AXIS2_PLACEMENT_3D ( 'NONE', #40817, #27809, #8219 ) ;
#27793 = CARTESIAN_POINT ( 'NONE',  ( -12.21488373879589240, 17.14500000000000313, 5.016499999999999737 ) ) ;
#27794 = CARTESIAN_POINT ( 'NONE',  ( -58.11144429832075531, 0.1746852717545294142, -1.039312118988176566E-14 ) ) ;
#27795 = CARTESIAN_POINT ( 'NONE',  ( -51.68405183998543606, 20.46365084016696301, -1.001587320847779132E-14 ) ) ;
#27796 = CARTESIAN_POINT ( 'NONE',  ( -18.61428830734555362, 154.1511370093759865, -0.1565858633853991211 ) ) ;
#27797 = EDGE_LOOP ( 'NONE', ( #37563, #14454, #6758, #40314 ) ) ;
#27798 = CARTESIAN_POINT ( 'NONE',  ( -49.15418727280429323, 24.05022843951647715, -1.025120094619365347E-14 ) ) ;
#27799 = CARTESIAN_POINT ( 'NONE',  ( -6.890691652417186397, 121.7969240507482169, -0.5388405038592991581 ) ) ;
#27800 = CARTESIAN_POINT ( 'NONE',  ( -7.862390625643993936, 122.3040693727414663, 0.4082539156324949126 ) ) ;
#27801 = ORIENTED_EDGE ( 'NONE', *, *, #852, .T. ) ;
#27802 = CARTESIAN_POINT ( 'NONE',  ( 2.015163235281668630, 118.7629491485439956, -1.152909370120437149 ) ) ;
#27803 = CARTESIAN_POINT ( 'NONE',  ( -2.801574634701766708, 120.9854572005495044, -0.1568784928360136832 ) ) ;
#27804 = CARTESIAN_POINT ( 'NONE',  ( 5.545296128261989033, -13.31524510490228508, 2.629257322947794684 ) ) ;
#27805 = CARTESIAN_POINT ( 'NONE',  ( -21.51971352461183074, 150.2128557559047692, 1.148904605754655694 ) ) ;
#27806 = CARTESIAN_POINT ( 'NONE',  ( 0.02983097946976470335, 117.3993836135854707, -1.492864285907033572 ) ) ;
#27807 = CARTESIAN_POINT ( 'NONE',  ( 5.738526254234393775, 159.1207877133979309, 0.2162537097210232850 ) ) ;
#27808 = CARTESIAN_POINT ( 'NONE',  ( 2.877599497300482145, 156.0997331449266028, 0.1009948612926021977 ) ) ;
#27809 = DIRECTION ( 'NONE',  ( 5.188838149069472160E-16, -1.699382548006136559E-16, -1.000000000000000000 ) ) ;
#27810 = CARTESIAN_POINT ( 'NONE',  ( 0.9303216910925710126, 27.28174836166085981, 0.2932329443217298603 ) ) ;
#27811 = CARTESIAN_POINT ( 'NONE',  ( -9.803363283900923264, 117.9968303279965340, -0.2884128246907767257 ) ) ;
#27812 = CARTESIAN_POINT ( 'NONE',  ( -8.519412162535125788, 69.40335734044577976, -1.269999999999996021 ) ) ;
#27813 = ORIENTED_EDGE ( 'NONE', *, *, #27222, .T. ) ;
#27814 = CARTESIAN_POINT ( 'NONE',  ( -23.75997692595333177, 82.67351089148900201, -1.524000000000006239 ) ) ;
#27815 = ORIENTED_EDGE ( 'NONE', *, *, #1205, .F. ) ;
#27816 = CARTESIAN_POINT ( 'NONE',  ( 8.405933479366224148, 119.4776037158581801, 1.396206739680378339 ) ) ;
#27817 = FACE_OUTER_BOUND ( 'NONE', #40461, .T. ) ;
#27818 = CARTESIAN_POINT ( 'NONE',  ( 19.25714749039842388, 152.1947311750261065, 2.059892502987373142 ) ) ;
#27819 = CARTESIAN_POINT ( 'NONE',  ( -58.31060438690772685, -0.1666892599193892099, -0.3090539641404843052 ) ) ;
#27820 = CARTESIAN_POINT ( 'NONE',  ( 14.40310572532104594, 154.4775811199918110, -1.681202589455180085 ) ) ;
#27821 = CARTESIAN_POINT ( 'NONE',  ( -8.047487967707532164, 27.33737370333709649, -2.486188741727015206 ) ) ;
#27822 = CARTESIAN_POINT ( 'NONE',  ( -3.066799924081489159, 159.2904672602661549, -0.9578552656232321993 ) ) ;
#27823 = CARTESIAN_POINT ( 'NONE',  ( 4.936507465849099496, 117.6536220454318311, -0.7445373667808669049 ) ) ;
#27824 = B_SPLINE_CURVE_WITH_KNOTS ( 'NONE', 3,
 ( #5514, #20831, #4894, #37451, #2322, #15282, #40257 ),
 .UNSPECIFIED., .F., .F.,
 ( 4, 3, 4 ),
 ( -5.999999998588015393E-08, 2.316105715148477490E-21, 6.533385609066403601E-05 ),
 .UNSPECIFIED. ) ;
#27825 = ORIENTED_EDGE ( 'NONE', *, *, #41808, .T. ) ;
#27826 = CARTESIAN_POINT ( 'NONE',  ( -9.295404511957364946, 124.2653519604415067, -0.02360630055292697871 ) ) ;
#27827 = CARTESIAN_POINT ( 'NONE',  ( -19.13882315974093018, 148.9694856701144090, -2.502273048283856660 ) ) ;
#27829 = CARTESIAN_POINT ( 'NONE',  ( 3.223661160190148145, -15.48894043311785396, 5.519697737696615647 ) ) ;
#27828 = VECTOR ( 'NONE', #33737, 1000.000000000000000 ) ;
#27830 = CLOSED_SHELL ( 'NONE', ( #10090, #20132, #40282, #17510, #33005, #32951, #14315, #34517, #4541, #6152, #10967, #32221, #10549, #31035, #2678, #16134, #7692 ) ) ;
#27831 = DIRECTION ( 'NONE',  ( 0.9454731675810359448, -0.3256999990547780333, 5.459396135145339171E-16 ) ) ;
#27832 = CARTESIAN_POINT ( 'NONE',  ( -2.554027823802438313, 117.3993834736394888, -1.425007985248354148 ) ) ;
#27833 = ORIENTED_EDGE ( 'NONE', *, *, #36079, .F. ) ;
#27834 = CARTESIAN_POINT ( 'NONE',  ( 13.13949684203664781, 123.8872625266795211, 1.904607404193280562 ) ) ;
#27835 = CARTESIAN_POINT ( 'NONE',  ( 4.886022116125724679, 117.7561648045584519, -0.7145573245312663024 ) ) ;
#27836 = CARTESIAN_POINT ( 'NONE',  ( -6.552964542248172189E-14, 78.83346620154574680, -6.511376220759049693E-18 ) ) ;
#27837 = CARTESIAN_POINT ( 'NONE',  ( -2.330098105383639595, 118.9955205646042344, 0.6366692849230545237 ) ) ;
#27838 = CARTESIAN_POINT ( 'NONE',  ( -8.048466033148526932, -0.5260294302935444311, 2.538140512261041426 ) ) ;
#27839 = CARTESIAN_POINT ( 'NONE',  ( 16.16038979459555236, 146.4165046419237228, 1.293905914731260598 ) ) ;
#27840 = CARTESIAN_POINT ( 'NONE',  ( -8.576171974424218192, 74.02775907367175989, -1.269999999999996909 ) ) ;
#27841 = ADVANCED_FACE ( 'NONE', ( #37110 ), #17701, .F. ) ;
#27842 = CARTESIAN_POINT ( 'NONE',  ( 22.82237111512518979, 142.4248215231809240, -0.5244786342524966338 ) ) ;
#27843 = PLANE ( 'NONE',  #19237 ) ;
#27844 = CARTESIAN_POINT ( 'NONE',  ( -58.36876032087972987, -0.2894071526118170423, 0.03821653909995503112 ) ) ;
#27845 = CARTESIAN_POINT ( 'NONE',  ( -29.12312633940434381, 66.61190372955218209, -1.524000000000006017 ) ) ;
#27846 = CARTESIAN_POINT ( 'NONE',  ( -25.77058783747419213, 72.83664265955201245, 1.269999999999993801 ) ) ;
#27847 = CARTESIAN_POINT ( 'NONE',  ( -4.416343619678607446, 118.1792209726063874, 0.3907444955660914210 ) ) ;
#27848 = CARTESIAN_POINT ( 'NONE',  ( -16.18905205736058051, 121.2598130428683447, -0.3234957879086919341 ) ) ;
#27849 = ORIENTED_EDGE ( 'NONE', *, *, #26331, .F. ) ;
#27850 = CARTESIAN_POINT ( 'NONE',  ( -52.97391985390434144, 12.30611266682019789, 4.247241762254901687 ) ) ;
#27851 = AXIS2_PLACEMENT_3D ( 'NONE', #37615, #8440, #37821 ) ;
#27852 = CARTESIAN_POINT ( 'NONE',  ( -6.259582159009869251, 119.8770361027300027, -1.223887577771844537 ) ) ;
#27853 = LINE ( 'NONE', #15272, #25117 ) ;
#27854 = CARTESIAN_POINT ( 'NONE',  ( 4.160022638901372360, 118.2392538408114717, 0.3840984172949051811 ) ) ;
#27855 = CARTESIAN_POINT ( 'NONE',  ( -12.50622671840202393, 130.7145975665201831, -1.030918987520083485 ) ) ;
#27856 = DIRECTION ( 'NONE',  ( -0.6559537821943227653, 0.7548010569845297058, -3.677505126197116308E-15 ) ) ;
#27857 = DIRECTION ( 'NONE',  ( -9.627370216492862708E-17, -1.000000000000000000, 0.000000000000000000 ) ) ;
#27858 = EDGE_LOOP ( 'NONE', ( #18603, #14055 ) ) ;
#27859 = CARTESIAN_POINT ( 'NONE',  ( 3.655561289726139140, 27.93047918286777076, -2.829280713513928180 ) ) ;
#27860 = CARTESIAN_POINT ( 'NONE',  ( -8.727673846237186339, 154.8283212766472445, -1.585547369736019840 ) ) ;
#27861 = CARTESIAN_POINT ( 'NONE',  ( -29.82321757229076908, 71.17901112636586447, 1.269999999999992690 ) ) ;
#27862 = CARTESIAN_POINT ( 'NONE',  ( -41.28107547821696954, 23.22158991241120063, 1.523999999999993138 ) ) ;
#27863 = CARTESIAN_POINT ( 'NONE',  ( -47.85244527695896011, 19.39403540832957518, 5.219971639306693056 ) ) ;
#27864 = CARTESIAN_POINT ( 'NONE',  ( -7.791833174368864690, 122.6039448250109132, -0.04536756530948493626 ) ) ;
#27865 = CARTESIAN_POINT ( 'NONE',  ( 4.626035402534343532, 22.79242798913371360, 0.3558936578225105341 ) ) ;
#27866 = CARTESIAN_POINT ( 'NONE',  ( 11.27775095430294350, 119.0414093155750379, 0.9684783378491815808 ) ) ;
#27867 = DIRECTION ( 'NONE',  ( 5.188838149069472160E-16, -1.699382548006136559E-16, -1.000000000000000000 ) ) ;
#27869 = CARTESIAN_POINT ( 'NONE',  ( 20.94193450296696923, 149.6610172957225586, -1.461262285038966047 ) ) ;
#27868 = CARTESIAN_POINT ( 'NONE',  ( 2.831922340016455042, -13.93067033233365315, 0.4309514144534042912 ) ) ;
#27870 = CARTESIAN_POINT ( 'NONE',  ( -12.07275429247933829, 123.1955650103826798, 1.290935347410189449 ) ) ;
#27871 = CARTESIAN_POINT ( 'NONE',  ( -2.961220487682185709, 16.77021669962341477, -3.573240411402743621 ) ) ;
#27872 = CARTESIAN_POINT ( 'NONE',  ( -22.68171885890644290, 150.0520759213295889, -1.302983692151378214 ) ) ;
#27873 = CARTESIAN_POINT ( 'NONE',  ( 0.7602462924416659718, 13.52415170902173891, -0.6087277422976011820 ) ) ;
#27874 = VERTEX_POINT ( 'NONE', #21309 ) ;
#27875 = CARTESIAN_POINT ( 'NONE',  ( -53.01551111795199489, 8.729259440421063942, -8.823202585156807211E-15 ) ) ;
#27876 = CARTESIAN_POINT ( 'NONE',  ( -4.503927054024219778, 120.9948550335633115, 0.2290337153283758254 ) ) ;
#27877 = CARTESIAN_POINT ( 'NONE',  ( 2.291753010757021869, -15.38865404460348962, 5.937071240476925027 ) ) ;
#27878 = CARTESIAN_POINT ( 'NONE',  ( 10.90507628433457832, 123.7747955097422476, -1.016219593014793920 ) ) ;
#27879 = ORIENTED_EDGE ( 'NONE', *, *, #40635, .F. ) ;
#27880 = CARTESIAN_POINT ( 'NONE',  ( 0.9953799440056341208, 115.7029401158592492, 1.748199640645290209 ) ) ;
#27881 = CARTESIAN_POINT ( 'NONE',  ( 3.243601939617143159, -13.81697766888033385, 2.329280267808830907 ) ) ;
#27882 = CARTESIAN_POINT ( 'NONE',  ( -4.764346593062310120, 117.8854850664883998, -0.8882920174160988669 ) ) ;
#27883 = ADVANCED_FACE ( 'NONE', ( #14927 ), #24308, .T. ) ;
#27884 = CARTESIAN_POINT ( 'NONE',  ( 10.21313493804724715, 125.9885856776569426, 0.1666469060040939310 ) ) ;
#27885 = EDGE_LOOP ( 'NONE', ( #6362, #23967, #18617, #22341 ) ) ;
#27886 = CARTESIAN_POINT ( 'NONE',  ( 18.81387422072291216, 135.8679125664981484, 2.390408806419126009 ) ) ;
#27887 = CARTESIAN_POINT ( 'NONE',  ( -3.174366308152013705, 104.6144662015457243, -0.06343139340882732180 ) ) ;
#27888 = CARTESIAN_POINT ( 'NONE',  ( 6.059261036834405978, 56.51500000000000057, 4.381499999999999950 ) ) ;
#27889 = EDGE_CURVE ( 'NONE', #28485, #4128, #28667, .T. ) ;
#27890 = CARTESIAN_POINT ( 'NONE',  ( -8.816700480405424756, 73.94613776634058411, 1.270000000000002460 ) ) ;
#27891 = CARTESIAN_POINT ( 'NONE',  ( 22.47159541194093180, 150.7739627601066275, -0.0002021107738995970768 ) ) ;
#27892 = CARTESIAN_POINT ( 'NONE',  ( -5.224239059777524119, 56.51499999999391122, -5.327449085208022517 ) ) ;
#27893 = CARTESIAN_POINT ( 'NONE',  ( 1.912458138725795065, -15.07098942588634749, 5.790420633640319892 ) ) ;
#27894 = CARTESIAN_POINT ( 'NONE',  ( -41.18107378286554621, 22.95619949144852967, 1.523999999999987143 ) ) ;
#27895 = CARTESIAN_POINT ( 'NONE',  ( 5.332935397695204749, 51.14746620154573264, 0.1065647409268304785 ) ) ;
#27896 = EDGE_CURVE ( 'NONE', #17488, #23143, #10293, .T. ) ;
#27897 = CARTESIAN_POINT ( 'NONE',  ( -4.685403574366763912, 117.8875460371219788, 0.8142817779486657415 ) ) ;
#27898 = VERTEX_POINT ( 'NONE', #24509 ) ;
#27899 = CARTESIAN_POINT ( 'NONE',  ( -0.4158538715318880197, 118.7629491485454025, 1.264086991023878115 ) ) ;
#27900 = CARTESIAN_POINT ( 'NONE',  ( 2.971243059491443184, 118.0891348236419844, -0.7498842069557943857 ) ) ;
#27901 = CARTESIAN_POINT ( 'NONE',  ( -4.012272795662658709, 117.4230540797109938, -0.9751040681224720785 ) ) ;
#27903 = CARTESIAN_POINT ( 'NONE',  ( 4.914877656105587356, 117.6230825708500305, 0.9484198851692730026 ) ) ;
#27902 = CIRCLE ( 'NONE', #36771, 0.3810000000000000053 ) ;
#27904 = CARTESIAN_POINT ( 'NONE',  ( -11.58677707360137354, 55.24499999999998323, -4.474811398758258285 ) ) ;
#27905 = CARTESIAN_POINT ( 'NONE',  ( -0.3981704103450558474, 123.4679809879532542, 0.1459118279324087830 ) ) ;
#27906 = CARTESIAN_POINT ( 'NONE',  ( 3.064284189169764971, -3.155149710853871525, 3.465721614369133174 ) ) ;
#27907 = CARTESIAN_POINT ( 'NONE',  ( -51.09183723991096571, 15.73968240350219538, 4.743875354842988834 ) ) ;
#27908 = DIRECTION ( 'NONE',  ( -0.01997839162482749342, -1.040247600000944484E-18, 0.9998004120163608288 ) ) ;
#27909 = CARTESIAN_POINT ( 'NONE',  ( 2.265044067826554652, -14.95788512594138631, 5.210342366881125287 ) ) ;
#27910 = CARTESIAN_POINT ( 'NONE',  ( 6.479951895127638473, 122.5560431351108974, 0.01853871597398580595 ) ) ;
#27911 = CARTESIAN_POINT ( 'NONE',  ( -6.989407220697516188, 121.9513345406523399, -0.1628094617627758867 ) ) ;
#27912 = FACE_OUTER_BOUND ( 'NONE', #8242, .T. ) ;
#27913 = EDGE_CURVE ( 'NONE', #4497, #24583, #27298, .T. ) ;
#27914 = CARTESIAN_POINT ( 'NONE',  ( -1.574722418245668942, 115.7027552838863045, 1.670860613881942847 ) ) ;
#27915 = CARTESIAN_POINT ( 'NONE',  ( 4.523211737919912601, 7.414965188139293062, 0.9565071382433592007 ) ) ;
#27916 = EDGE_LOOP ( 'NONE', ( #39252, #10699, #40970, #41101 ) ) ;
#27917 = CARTESIAN_POINT ( 'NONE',  ( 4.429703416477502209, 104.6144662015456817, -1.943618747302600092 ) ) ;
#27918 = CARTESIAN_POINT ( 'NONE',  ( 2.004873297308811253, -15.47002699807756265, 5.272742632645636363 ) ) ;
#27919 = CARTESIAN_POINT ( 'NONE',  ( -12.07139305262857043, 121.8643784861682065, 1.276542069712922611 ) ) ;
#27920 = CARTESIAN_POINT ( 'NONE',  ( -0.9630862182390291792, 27.11985920190685917, 0.1463314843619143713 ) ) ;
#27921 = CARTESIAN_POINT ( 'NONE',  ( 0.8728101606606677443, 18.85996454746999618, -0.4358653558870161926 ) ) ;
#27922 = EDGE_CURVE ( 'NONE', #24940, #18746, #5167, .T. ) ;
#27923 = ORIENTED_EDGE ( 'NONE', *, *, #4066, .T. ) ;
#27924 = ORIENTED_EDGE ( 'NONE', *, *, #22738, .F. ) ;
#27925 = DIRECTION ( 'NONE',  ( -5.188838149069472160E-16, 1.699382548006136066E-16, 1.000000000000000000 ) ) ;
#27926 = CARTESIAN_POINT ( 'NONE',  ( 2.170296427606156708, 116.5145642697238344, 1.453337335755149784 ) ) ;
#27927 = CARTESIAN_POINT ( 'NONE',  ( -7.932268303791008890, 121.8456834504061845, 0.6952039612942496616 ) ) ;
#27928 = LINE ( 'NONE', #5375, #11655 ) ;
#27929 = CARTESIAN_POINT ( 'NONE',  ( 3.391857759029038633, -13.93828481737184610, 3.530066096054821134 ) ) ;
#27930 = CARTESIAN_POINT ( 'NONE',  ( 5.874384117068456312, 120.0568572605186546, -0.8667843538975028572 ) ) ;
#27931 = CARTESIAN_POINT ( 'NONE',  ( -6.532233579562855219, 157.6773268839678508, -1.915660460402585530 ) ) ;
#27932 = CARTESIAN_POINT ( 'NONE',  ( 4.741393556337476944, 117.7888895289213878, -0.8991427661700817087 ) ) ;
#27933 = VECTOR ( 'NONE', #12051, 1000.000000000000227 ) ;
#27934 = ADVANCED_FACE ( 'NONE', ( #30918 ), #39563, .F. ) ;
#27935 = CARTESIAN_POINT ( 'NONE',  ( 4.122343337852331757, 118.2429491485453497, -0.1816822259850767451 ) ) ;
#27936 = CARTESIAN_POINT ( 'NONE',  ( 5.257554009420233321, 121.2670714900434206, -0.1164621724739933611 ) ) ;
#27937 = ORIENTED_EDGE ( 'NONE', *, *, #37873, .F. ) ;
#27938 = CARTESIAN_POINT ( 'NONE',  ( 2.856221160286674277, -14.96258862872340600, 4.237710179968991575 ) ) ;
#27939 = VECTOR ( 'NONE', #10865, 1000.000000000000000 ) ;
#27940 = CARTESIAN_POINT ( 'NONE',  ( -3.932819197772147390, 27.98301002373794333, 0.4898618918306563708 ) ) ;
#27941 = CARTESIAN_POINT ( 'NONE',  ( -58.49146960918517379, -0.5079027975612510071, 0.2843517202610890138 ) ) ;
#27942 = CARTESIAN_POINT ( 'NONE',  ( 1.818839793882075728, -13.69063247836898611, -4.255424433905749204 ) ) ;
#27943 = CARTESIAN_POINT ( 'NONE',  ( 16.79675997928894304, 147.6865045845431723, 1.918872074639297098 ) ) ;
#27944 = CARTESIAN_POINT ( 'NONE',  ( -2.630585380139099705, 29.80773254623414914, 2.003937124266777836 ) ) ;
#27945 = CARTESIAN_POINT ( 'NONE',  ( -3.905206024139432408, 115.3331674797404247, 1.578293011005953650 ) ) ;
#27946 = CARTESIAN_POINT ( 'NONE',  ( 3.064284189169764971, -3.155149710853871525, 3.465721614369133174 ) ) ;
#27947 = CARTESIAN_POINT ( 'NONE',  ( -1.114473875789821378, 36.31367722304657519, -0.2353634988756885538 ) ) ;
#27948 = CARTESIAN_POINT ( 'NONE',  ( -4.887076909682236625, -2.444604220856811505, -6.895871986673536291 ) ) ;
#27949 = CARTESIAN_POINT ( 'NONE',  ( -57.26476250566310711, 1.946856395439316989, -1.045107959733444281 ) ) ;
#27950 = CARTESIAN_POINT ( 'NONE',  ( 5.545678171451279503, 116.8412816117532742, -0.2872682508620105768 ) ) ;
#27951 = DIRECTION ( 'NONE',  ( 0.000000000000000000, 0.000000000000000000, 1.000000000000000000 ) ) ;
#27952 = DIRECTION ( 'NONE',  ( -9.627370216492862708E-17, -1.000000000000000000, 0.000000000000000000 ) ) ;
#27953 = CARTESIAN_POINT ( 'NONE',  ( -6.346781410994640993, 30.04503731349425166, 1.591420273447384348 ) ) ;
#27954 = CIRCLE ( 'NONE', #36158, 3.175000000000001155 ) ;
#27955 = CARTESIAN_POINT ( 'NONE',  ( 0.2927481059715184020, -9.205330264445118260, -8.420370646799414160 ) ) ;
#27956 = CARTESIAN_POINT ( 'NONE',  ( 0.3872878167242116976, 117.3993820581147389, 1.495215202982832947 ) ) ;
#27957 = CARTESIAN_POINT ( 'NONE',  ( -24.26619908708080686, 81.70586579672512073, -1.524000000000006239 ) ) ;
#27958 = DIRECTION ( 'NONE',  ( 4.017660918040594346E-17, -1.000000000000000000, -2.376309959284834438E-19 ) ) ;
#27959 = CARTESIAN_POINT ( 'NONE',  ( 0.7718547489770499759, 119.9044272045951374, -0.6164056859965564295 ) ) ;
#27960 = CARTESIAN_POINT ( 'NONE',  ( -0.006534887713674904404, 159.5822087645323393, 0.3270325034788581497 ) ) ;
#27961 = EDGE_CURVE ( 'NONE', #31875, #27131, #12998, .T. ) ;
#27962 = ORIENTED_EDGE ( 'NONE', *, *, #6096, .F. ) ;
#27963 = CARTESIAN_POINT ( 'NONE',  ( -58.33482727260577860, 1.278009831242016281, -0.06942977984277290404 ) ) ;
#27964 = EDGE_CURVE ( 'NONE', #22515, #8970, #6234, .T. ) ;
#27965 = VERTEX_POINT ( 'NONE', #12584 ) ;
#27966 = CARTESIAN_POINT ( 'NONE',  ( -47.33874550351251997, 19.91900851598762046, -5.121984950663424740 ) ) ;
#27967 = CARTESIAN_POINT ( 'NONE',  ( -14.67500508075667298, 148.8517222230099719, -0.2932415260845991356 ) ) ;
#27968 = CARTESIAN_POINT ( 'NONE',  ( 5.598737995799250911, -15.07077801197512201, 2.339151774602123979 ) ) ;
#27969 = CARTESIAN_POINT ( 'NONE',  ( -19.85075266274223083, 150.7280352275851101, 1.521773064777484308 ) ) ;
#27970 = CARTESIAN_POINT ( 'NONE',  ( 21.20416308100189440, 151.2337125027825095, -0.8636963275675616503 ) ) ;
#27971 = CARTESIAN_POINT ( 'NONE',  ( -2.614655561276646889, 23.60746518810343986, 3.812863311767609620 ) ) ;
#27972 = CARTESIAN_POINT ( 'NONE',  ( -7.991309159113160199, 158.6817341734954425, -0.4848270063548277276 ) ) ;
#27973 = CARTESIAN_POINT ( 'NONE',  ( -49.51384108118372751, 17.06003269541576017, -5.024714039402652155 ) ) ;
#27974 = VERTEX_POINT ( 'NONE', #41574 ) ;
#27975 = CARTESIAN_POINT ( 'NONE',  ( 2.185361284265998183, 116.2036773648440402, 0.07441525802958044722 ) ) ;
#27976 = DIRECTION ( 'NONE',  ( -0.8745520943968240202, 0.4849315768086551737, -5.361993529360572958E-16 ) ) ;
#27977 = CARTESIAN_POINT ( 'NONE',  ( -9.055011062052066961, 121.9018297702777858, 0.9711463333382076568 ) ) ;
#27978 = CARTESIAN_POINT ( 'NONE',  ( -48.81575351190421941, 18.06815554827317882, -5.105115732439140963 ) ) ;
#27979 = EDGE_CURVE ( 'NONE', #14494, #40718, #9188, .T. ) ;
#27980 = CARTESIAN_POINT ( 'NONE',  ( 0.4903093677401612061, 118.8635629087341954, -0.5952627799645435758 ) ) ;
#27981 = CARTESIAN_POINT ( 'NONE',  ( -20.82206258336681159, 149.3152741295656369, -2.348048710389011529 ) ) ;
#27982 = CARTESIAN_POINT ( 'NONE',  ( -51.34009458250667279, 14.66650723912346699, -4.800162786360146150 ) ) ;
#27983 = EDGE_CURVE ( 'NONE', #4082, #15081, #23881, .T. ) ;
#27984 = CARTESIAN_POINT ( 'NONE',  ( 9.105332701317813360, 123.1184971541203055, -0.5608273726695747197 ) ) ;
#27985 = ORIENTED_EDGE ( 'NONE', *, *, #26631, .T. ) ;
#27986 = CARTESIAN_POINT ( 'NONE',  ( -15.87222905729445266, 135.0473088626721392, -2.190551936964585167 ) ) ;
#27987 = CARTESIAN_POINT ( 'NONE',  ( 2.909835405328949687, -15.65209430229147536, 4.668939894544173796 ) ) ;
#27988 = CARTESIAN_POINT ( 'NONE',  ( -4.502791693421113628, 118.1162640722260164, -0.7113048364058234263 ) ) ;
#27989 = TOROIDAL_SURFACE ( 'NONE', #9624, 0.3810000000000005604, 0.2540000000000000036 ) ;
#27990 = CARTESIAN_POINT ( 'NONE',  ( -57.00508801794419611, 2.691366720778187727, -1.977812201481553567 ) ) ;
#27991 = CARTESIAN_POINT ( 'NONE',  ( -4.995814232853128090, 117.4677515080094707, 0.7870683612790911887 ) ) ;
#27992 = CARTESIAN_POINT ( 'NONE',  ( 10.71652553037521827, 154.3566586077636487, 1.965850361453045814 ) ) ;
#27993 = DIRECTION ( 'NONE',  ( -5.188838149069472160E-16, 1.699382548006136559E-16, 1.000000000000000000 ) ) ;
#27994 = CARTESIAN_POINT ( 'NONE',  ( -6.252972126910993467, 3.963778981710710969, 5.644239715445565686 ) ) ;
#27995 = CARTESIAN_POINT ( 'NONE',  ( 2.970866406646140767, 156.0959049650892041, 0.4589190987796911703 ) ) ;
#27996 = LINE ( 'NONE', #25013, #39186 ) ;
#27998 = VERTEX_POINT ( 'NONE', #9389 ) ;
#27997 = CARTESIAN_POINT ( 'NONE',  ( -41.05189575270519242, 23.09451173561983239, -5.978253955787443857E-15 ) ) ;
#27999 = CARTESIAN_POINT ( 'NONE',  ( 4.027359296022574142, 109.3894120745859055, -3.506257160670660067 ) ) ;
#28000 = CARTESIAN_POINT ( 'NONE',  ( -7.799329138056211974, 122.5403491326864298, -0.4385002940562175433 ) ) ;
#28001 = CARTESIAN_POINT ( 'NONE',  ( -57.56998337575458891, 1.440017903778734176, 1.358936928125925814 ) ) ;
#28002 = CARTESIAN_POINT ( 'NONE',  ( -51.34394198884087501, 20.23131347170496142, 0.7795225783603342284 ) ) ;
#28003 = CARTESIAN_POINT ( 'NONE',  ( -15.85175717768499659, 121.0146182718019645, -0.1572851932169302969 ) ) ;
#28004 = ORIENTED_EDGE ( 'NONE', *, *, #30849, .T. ) ;
#28005 = CARTESIAN_POINT ( 'NONE',  ( -47.59569394876871229, 21.45978420380969354, -4.300550031832348630 ) ) ;
#28006 = CARTESIAN_POINT ( 'NONE',  ( 5.812554992953963051, 121.1879478854047392, -0.2779057282218665992 ) ) ;
#28007 = CARTESIAN_POINT ( 'NONE',  ( -8.022816897867325991, 121.5631586913658140, 0.8332660241015908964 ) ) ;
#28008 = ORIENTED_EDGE ( 'NONE', *, *, #32332, .F. ) ;
#28009 = CARTESIAN_POINT ( 'NONE',  ( 0.1384230549150444467, 115.7030668735399246, -1.759162436720742795 ) ) ;
#28010 = CARTESIAN_POINT ( 'NONE',  ( -6.485149764178151699, 121.7431354732680973, -0.3115821950655745520 ) ) ;
#28011 = CARTESIAN_POINT ( 'NONE',  ( 4.549387865739121573, -13.93190642666217194, 4.188617477609191120 ) ) ;
#28012 = CARTESIAN_POINT ( 'NONE',  ( -12.49407882476853082, 156.7420262770442037, 1.161473977901223753 ) ) ;
#28013 = CARTESIAN_POINT ( 'NONE',  ( 17.14499999999999957, 71.11999999999999034, -1.904999999999999583 ) ) ;
#28014 = AXIS2_PLACEMENT_3D ( 'NONE', #29691, #16262, #19459 ) ;
#28015 = CARTESIAN_POINT ( 'NONE',  ( 5.792301705315622939, 116.9567987913546006, 0.2385690759321334731 ) ) ;
#28016 = CARTESIAN_POINT ( 'NONE',  ( 15.26262975078991779, 148.0175730704188481, 0.3049836654608578113 ) ) ;
#28017 = CARTESIAN_POINT ( 'NONE',  ( 16.60960244842765832, -1.599067919197793490E-15, 2.034089647357696937E-15 ) ) ;
#28018 = CARTESIAN_POINT ( 'NONE',  ( 0.3817720443006957232, 19.93710050853265869, -0.8978640518339636722 ) ) ;
#28019 = CARTESIAN_POINT ( 'NONE',  ( -8.215520591712516918, 117.5015518944296247, -0.2087872862963602583 ) ) ;
#28020 = CARTESIAN_POINT ( 'NONE',  ( 5.008289758173663841, 117.3984635900009295, -0.7758770640922041384 ) ) ;
#28021 = CARTESIAN_POINT ( 'NONE',  ( 5.177913976931207252, 64.41499993257285439, -5.372100000000002318 ) ) ;
#28022 = ORIENTED_EDGE ( 'NONE', *, *, #39384, .T. ) ;
#28023 = CARTESIAN_POINT ( 'NONE',  ( -5.802623703142025136, 118.2257019569944987, 0.8941158778616000724 ) ) ;
#28024 = CARTESIAN_POINT ( 'NONE',  ( -5.334232279151433609, 105.1224713109533155, 0.08197798277522774790 ) ) ;
#28025 = CARTESIAN_POINT ( 'NONE',  ( 1.070729637574014737, 117.4935207075373569, 0.5386181289574429876 ) ) ;
#28026 = CARTESIAN_POINT ( 'NONE',  ( -58.43492521371434378, -0.3997831091937082415, -0.3282367010173031230 ) ) ;
#28027 = CARTESIAN_POINT ( 'NONE',  ( 20.59420924110313678, 148.8605967840894095, -1.615102827552612252 ) ) ;
#28028 = CARTESIAN_POINT ( 'NONE',  ( 8.421720897435127640, 23.01747231734997357, -0.09500337383513672573 ) ) ;
#28029 = CARTESIAN_POINT ( 'NONE',  ( -12.77893255256123339, 120.0678233105195716, -1.216039656670922176 ) ) ;
#28030 = CARTESIAN_POINT ( 'NONE',  ( 4.896450774471631462, 117.7232630146785368, -0.7635348429027170036 ) ) ;
#28031 = EDGE_CURVE ( 'NONE', #36618, #41397, #32980, .T. ) ;
#28032 = CARTESIAN_POINT ( 'NONE',  ( 6.689329653978076884, 121.2318545172250737, 0.3418430003135980444 ) ) ;
#28033 = ORIENTED_EDGE ( 'NONE', *, *, #34877, .T. ) ;
#28034 = CARTESIAN_POINT ( 'NONE',  ( -11.11302231477190361, 128.0707465396788507, -0.1214933242792290563 ) ) ;
#28035 = CARTESIAN_POINT ( 'NONE',  ( -11.88178580215919133, 154.9039014673913073, -2.222676336029907773 ) ) ;
#28036 = AXIS2_PLACEMENT_3D ( 'NONE', #8156, #15586, #21126 ) ;
#28037 = CARTESIAN_POINT ( 'NONE',  ( 4.717164877559400615, -15.39354034361711854, 4.072675418279473547 ) ) ;
#28038 =( BOUNDED_CURVE ( )  B_SPLINE_CURVE ( 3, ( #36027, #22997, #20649, #7268 ),
 .UNSPECIFIED., .F., .F. ) 
 B_SPLINE_CURVE_WITH_KNOTS ( ( 4, 4 ),
 ( 4.712388980384690562, 6.283185307179586232 ),
 .UNSPECIFIED. ) 
 CURVE ( )  GEOMETRIC_REPRESENTATION_ITEM ( )  RATIONAL_B_SPLINE_CURVE ( ( 1.000000000000000000, 0.8047378541243652705, 0.8047378541243652705, 1.000000000000000000 ) ) 
 REPRESENTATION_ITEM ( '' )  );
#28039 = CARTESIAN_POINT ( 'NONE',  ( 4.880630303840320039, 56.51998046905275430, 4.886936331184463356 ) ) ;
#28040 = ORIENTED_EDGE ( 'NONE', *, *, #30525, .F. ) ;
#28041 = CARTESIAN_POINT ( 'NONE',  ( 17.41382892593903620, 149.8167423968465073, 2.401583459992671976 ) ) ;
#28042 = CARTESIAN_POINT ( 'NONE',  ( -3.831877602099685198, 71.07198261757335445, -1.269999999999993801 ) ) ;
#28043 = CARTESIAN_POINT ( 'NONE',  ( -26.51793118801306548, 72.98537704160715123, -1.270000000000006013 ) ) ;
#28044 = AXIS2_PLACEMENT_3D ( 'NONE', #15381, #24975, #41393 ) ;
#28045 = CARTESIAN_POINT ( 'NONE',  ( -1.803835135052293870, 120.9773948236336878, 0.3431470217397348255 ) ) ;
#28046 = CARTESIAN_POINT ( 'NONE',  ( -1.690137127919513649, -8.491432666745847513, 8.270632449787910900 ) ) ;
#28047 = CARTESIAN_POINT ( 'NONE',  ( 1.517991627498671114, 120.5919059741422217, 0.3392643659851173332 ) ) ;
#28048 = CARTESIAN_POINT ( 'NONE',  ( -46.60530155212503445, 26.17382724835477958, -1.524000000000008459 ) ) ;
#28049 = CARTESIAN_POINT ( 'NONE',  ( 22.39781672572311422, 150.5530013069706285, -0.3987920954333211698 ) ) ;
#28050 = CARTESIAN_POINT ( 'NONE',  ( 5.941750550382240093, 57.15000000000122071, -5.016499999999999737 ) ) ;
#28051 = CARTESIAN_POINT ( 'NONE',  ( -57.98432510407339180, 0.5385510273032687589, 0.8796703754388934815 ) ) ;
#28052 = CARTESIAN_POINT ( 'NONE',  ( -29.91360363449003756, 70.04874496952835727, -1.524000000000007349 ) ) ;
#28053 = CARTESIAN_POINT ( 'NONE',  ( -18.01920641645600796, 83.84822824455467583, -1.524000000000003352 ) ) ;
#28054 = CARTESIAN_POINT ( 'NONE',  ( -4.172699785897756364, 118.2392038860674290, 0.2169064230006704508 ) ) ;
#28055 = CIRCLE ( 'NONE', #14465, 3.683000000000001162 ) ;
#28056 = VERTEX_POINT ( 'NONE', #12383 ) ;
#28057 = CARTESIAN_POINT ( 'NONE',  ( -53.75224695799815322, 9.373383622779334345, 3.688627211158417296 ) ) ;
#28058 = CARTESIAN_POINT ( 'NONE',  ( 4.053501715161472951, 119.1603328138294984, -0.7634023787871468958 ) ) ;
#28059 = CARTESIAN_POINT ( 'NONE',  ( -0.1506890447697080415, 104.6144662015457527, 6.108955356427616223 ) ) ;
#28060 = CARTESIAN_POINT ( 'NONE',  ( 4.418034652924236916, 118.1647599079729360, 0.6322107996853220113 ) ) ;
#28061 = CARTESIAN_POINT ( 'NONE',  ( -11.72694347678957705, 128.3321206738457647, -0.9702521317530997669 ) ) ;
#28062 = B_SPLINE_CURVE_WITH_KNOTS ( 'NONE', 3,
 ( #2209, #24339, #27549, #18782, #34785, #1787 ),
 .UNSPECIFIED., .F., .F.,
 ( 4, 2, 4 ),
 ( 0.000000000000000000, 0.4601069123252314874, 0.9202138246504629748 ),
 .UNSPECIFIED. ) ;
#28063 = DIRECTION ( 'NONE',  ( -0.1906721105965186736, 0.9816537812491066273, 0.000000000000000000 ) ) ;
#28064 = CARTESIAN_POINT ( 'NONE',  ( 15.56076557482319700, 120.7233670659379214, 0.3109411287488705877 ) ) ;
#28065 = ORIENTED_EDGE ( 'NONE', *, *, #35598, .F. ) ;
#28066 = CARTESIAN_POINT ( 'NONE',  ( -4.191205975170537279, 21.45845178295031630, -1.961646697876042511 ) ) ;
#28067 = CARTESIAN_POINT ( 'NONE',  ( -29.22020851855505441, 63.09400180734589014, 1.524000000000856669 ) ) ;
#28068 = CARTESIAN_POINT ( 'NONE',  ( -6.194847070882102180, 64.72978607931611350, -1.523999999999994026 ) ) ;
#28069 = CARTESIAN_POINT ( 'NONE',  ( -22.95370498042275642, 82.54569470718179502, -1.270000000000005791 ) ) ;
#28070 = CARTESIAN_POINT ( 'NONE',  ( -48.16751460313091115, 19.56873862626650507, 5.361827705663260168 ) ) ;
#28071 = CARTESIAN_POINT ( 'NONE',  ( -6.086536517656333523, 121.3448157377453214, 0.2330812820862587509 ) ) ;
#28072 = CARTESIAN_POINT ( 'NONE',  ( -4.384008014420753163, 17.61986127277741332, -1.463615122064717111 ) ) ;
#28073 = CARTESIAN_POINT ( 'NONE',  ( 6.882329627759393276, 117.5897289630162987, 0.7523600398187280103 ) ) ;
#28074 = CARTESIAN_POINT ( 'NONE',  ( -3.485531464485784880, 104.6144662015454685, -3.352429072091678286 ) ) ;
#28076 = CARTESIAN_POINT ( 'NONE',  ( 1.132512924677445243, 117.7697124030934077, -0.5521475598058975809 ) ) ;
#28075 = CARTESIAN_POINT ( 'NONE',  ( 3.131015516031846690, -14.62848841321586946, 3.524024012273756501 ) ) ;
#28077 = CARTESIAN_POINT ( 'NONE',  ( -17.21863486588935288, 149.7102054596878702, 1.666570748255499224 ) ) ;
#28078 = CARTESIAN_POINT ( 'NONE',  ( -4.487480840803009130, 27.34045677879159442, -1.100063755011520872 ) ) ;
#28079 = CARTESIAN_POINT ( 'NONE',  ( -14.21090189159867023, 120.4756499382577886, -1.027290292067533306 ) ) ;
#28080 = AXIS2_PLACEMENT_3D ( 'NONE', #25196, #28395, #38200 ) ;
#28081 = CARTESIAN_POINT ( 'NONE',  ( -0.5888577047260095121, 18.69815917492401880, 0.7773729966010974879 ) ) ;
#28082 = ORIENTED_EDGE ( 'NONE', *, *, #4704, .T. ) ;
#28083 = CARTESIAN_POINT ( 'NONE',  ( -56.91016477577836952, 2.896953902749091370, 2.060321699028983211 ) ) ;
#28084 = CARTESIAN_POINT ( 'NONE',  ( -0.6885929357778710624, 156.3445873232922736, 0.4144571531603685188 ) ) ;
#28085 = CARTESIAN_POINT ( 'NONE',  ( 3.754230566796173285, -14.80532124960526374, 5.272564796848507207 ) ) ;
#28086 = CARTESIAN_POINT ( 'NONE',  ( 9.865641862003126761, 123.3250567171901082, -0.7964883383408414286 ) ) ;
#28087 = ORIENTED_EDGE ( 'NONE', *, *, #12698, .T. ) ;
#28088 = ADVANCED_FACE ( 'NONE', ( #15769 ), #38162, .F. ) ;
#28089 = CARTESIAN_POINT ( 'NONE',  ( 1.187391129625792630, 115.7029482326351086, 1.742295690021671062 ) ) ;
#28090 = AXIS2_PLACEMENT_3D ( 'NONE', #26968, #36981, #23327 ) ;
#28091 = CARTESIAN_POINT ( 'NONE',  ( -4.731399709915055318, 117.6315807060625929, -1.144721263631117703 ) ) ;
#28092 = CARTESIAN_POINT ( 'NONE',  ( 15.38626016046108447, 147.8278496344100859, 0.1795882337043284427 ) ) ;
#28093 = ORIENTED_EDGE ( 'NONE', *, *, #39691, .F. ) ;
#28094 = CARTESIAN_POINT ( 'NONE',  ( 13.31282764718921818, 122.3357896625302459, 1.791091420989350480 ) ) ;
#28095 = CARTESIAN_POINT ( 'NONE',  ( 4.218275339060157059, 155.8585684991085714, 0.08429118021179421438 ) ) ;
#28096 = DIRECTION ( 'NONE',  ( 0.9849462604886048966, -0.000000000000000000, 0.1728608224830406881 ) ) ;
#28097 = CARTESIAN_POINT ( 'NONE',  ( 0.01645572339161321951, 159.4324016994384010, -0.8235116888278192215 ) ) ;
#28098 = CARTESIAN_POINT ( 'NONE',  ( 1.860994725975919639, 116.5907236856068181, -0.1449800026146564336 ) ) ;
#28099 = CARTESIAN_POINT ( 'NONE',  ( -15.77830307927088249, 80.39606975582424297, -1.270000000000001572 ) ) ;
#28100 = AXIS2_PLACEMENT_3D ( 'NONE', #14852, #27856, #15490 ) ;
#28101 = CARTESIAN_POINT ( 'NONE',  ( 1.755413149268191475, -15.27739615427885234, 5.432748241580562798 ) ) ;
#28102 = CARTESIAN_POINT ( 'NONE',  ( -2.872265077263356226, 44.28946620154572855, -5.646510212151727437 ) ) ;
#28103 = CARTESIAN_POINT ( 'NONE',  ( -14.42383115828894447, 69.61113539875873357, -1.523999999999998911 ) ) ;
#28104 = CIRCLE ( 'NONE', #21316, 6.985000000000000320 ) ;
#28105 = CARTESIAN_POINT ( 'NONE',  ( -4.725628595103277263, 117.9692962743044120, 0.6259887252853451045 ) ) ;
#28106 = VERTEX_POINT ( 'NONE', #15350 ) ;
#28107 = ORIENTED_EDGE ( 'NONE', *, *, #7690, .F. ) ;
#28108 = DIRECTION ( 'NONE',  ( -5.188838149069471174E-16, 1.699382548006136313E-16, 1.000000000000000000 ) ) ;
#28109 = CARTESIAN_POINT ( 'NONE',  ( 5.625948711771986410, 118.2002780182136235, -0.9209370785259048953 ) ) ;
#28110 = CARTESIAN_POINT ( 'NONE',  ( -4.310423192639097678, 113.1344509532474376, -2.465321907391796241 ) ) ;
#28111 = CARTESIAN_POINT ( 'NONE',  ( 4.894219456065178164, 117.5445796760222521, 1.081411616995204161 ) ) ;
#28112 = CARTESIAN_POINT ( 'NONE',  ( -4.641629919619552957, 117.8847811183079841, -1.004318260171652266 ) ) ;
#28113 = CARTESIAN_POINT ( 'NONE',  ( -0.3848090724908974636, 122.5569158606515003, 0.2475921850528965407 ) ) ;
#28114 = AXIS2_PLACEMENT_3D ( 'NONE', #39171, #9978, #32784 ) ;
#28115 = CARTESIAN_POINT ( 'NONE',  ( -4.515506726787251068, -6.291224493951820484, 1.111903093310195212 ) ) ;
#28116 = DIRECTION ( 'NONE',  ( -9.627370216492862708E-17, -1.000000000000000000, 0.000000000000000000 ) ) ;
#28117 = DIRECTION ( 'NONE',  ( 0.000000000000000000, -0.000000000000000000, 1.000000000000000000 ) ) ;
#28118 = CARTESIAN_POINT ( 'NONE',  ( 3.463597221183738917, -14.01103841792809845, 4.185469790819682068 ) ) ;
#28119 = CARTESIAN_POINT ( 'NONE',  ( 4.642736441617618226, 114.7252160460498516, -1.690332539979629400 ) ) ;
#28120 = CARTESIAN_POINT ( 'NONE',  ( -11.08617792162982063, 123.6647009725989648, -1.535475951868171984 ) ) ;
#28121 = CARTESIAN_POINT ( 'NONE',  ( 5.125711319336574867, 116.9834589889111385, -0.2401983985477860184 ) ) ;
#28122 = CARTESIAN_POINT ( 'NONE',  ( -6.024379985667599691, 30.10344933946137402, 2.517894167085569457 ) ) ;
#28123 = CARTESIAN_POINT ( 'NONE',  ( -1.330810070361397646, 115.7029491485453576, 1.688173640172494272 ) ) ;
#28124 = CARTESIAN_POINT ( 'NONE',  ( -4.636761822055341042, 12.60011390031314349, 0.2095705037016724059 ) ) ;
#28126 = ORIENTED_EDGE ( 'NONE', *, *, #22168, .T. ) ;
#28125 = CARTESIAN_POINT ( 'NONE',  ( 20.06391502460626697, 128.8637844977697569, 0.9116527748870054682 ) ) ;
#28127 = CARTESIAN_POINT ( 'NONE',  ( 2.874780220322234126, 104.6144662015304476, -4.506434701495114048 ) ) ;
#28128 = CARTESIAN_POINT ( 'NONE',  ( 4.348370292662268710, -15.56902811939260545, 2.317716755344581880 ) ) ;
#28129 = CARTESIAN_POINT ( 'NONE',  ( -12.27894764211880485, 122.3148578561100948, 1.306772475271723799 ) ) ;
#28130 = CARTESIAN_POINT ( 'NONE',  ( 0.7509867122348852231, -11.68634165275979342, 0.6197512838553165260 ) ) ;
#28131 = CARTESIAN_POINT ( 'NONE',  ( 0.1081409728947390902, 20.38375149489202443, -0.9727671068919315767 ) ) ;
#28132 = EDGE_CURVE ( 'NONE', #8806, #39680, #38496, .T. ) ;
#28133 = ADVANCED_FACE ( 'NONE', ( #6993 ), #19962, .T. ) ;
#28134 = VERTEX_POINT ( 'NONE', #25161 ) ;
#28135 = VERTEX_POINT ( 'NONE', #15973 ) ;
#28136 = LINE ( 'NONE', #15559, #2470 ) ;
#28137 = CARTESIAN_POINT ( 'NONE',  ( 0.8148005656457013579, 107.7619142660649203, 4.566897024910153924 ) ) ;
#28138 = CARTESIAN_POINT ( 'NONE',  ( -11.28744401931967545, 153.2158294759273360, 1.114070445992416003 ) ) ;
#28139 = DIRECTION ( 'NONE',  ( -0.9998004120163609398, 0.000000000000000000, -0.01997839162482749689 ) ) ;
#28140 = CARTESIAN_POINT ( 'NONE',  ( 2.317735183313462066, -14.86924938851764999, 5.343245562499194357 ) ) ;
#28141 = CARTESIAN_POINT ( 'NONE',  ( 3.856066505249522880, 156.9018388488748883, -1.546468145409083839 ) ) ;
#28142 = AXIS2_PLACEMENT_3D ( 'NONE', #21602, #34630, #40607 ) ;
#28143 = CARTESIAN_POINT ( 'NONE',  ( -20.09316625820300573, 147.7236477000422497, -2.507557202006583719 ) ) ;
#28144 = DIRECTION ( 'NONE',  ( 0.9998004120163609398, 0.000000000000000000, 0.01997839162482749689 ) ) ;
#28145 = CARTESIAN_POINT ( 'NONE',  ( -4.998096739426165946, 117.4661840451863100, 0.7739782158464477702 ) ) ;
#28146 = CARTESIAN_POINT ( 'NONE',  ( 4.119320774684384290, 118.2429491485453354, -0.1851223333593593479 ) ) ;
#28147 = CARTESIAN_POINT ( 'NONE',  ( 5.910930898603123929, 121.4708175001875077, -0.1161132702817543050 ) ) ;
#28148 = CIRCLE ( 'NONE', #5730, 0.6350000000000006750 ) ;
#28149 = VERTEX_POINT ( 'NONE', #29565 ) ;
#28150 = CARTESIAN_POINT ( 'NONE',  ( 3.151249207183300260, -14.28495848352401332, 1.742053583190615207 ) ) ;
#28151 = CARTESIAN_POINT ( 'NONE',  ( -16.02764313970816090, 80.34763903973272647, 1.269999999999997353 ) ) ;
#28152 = CARTESIAN_POINT ( 'NONE',  ( 4.956296842134184644, 117.5943721824530286, 0.8964810703344230358 ) ) ;
#28153 = CIRCLE ( 'NONE', #40428, 12.69999999999999751 ) ;
#28154 = CARTESIAN_POINT ( 'NONE',  ( -54.28468382810394388, 8.706709151474493424, 3.613316249070154473 ) ) ;
#28155 = CARTESIAN_POINT ( 'NONE',  ( -4.227217475240903077, -11.31673468295422147, -1.889206449475258509 ) ) ;
#28156 = CARTESIAN_POINT ( 'NONE',  ( 8.650892266477013592, 122.3401343867201945, 1.081441824013609443 ) ) ;
#28157 = CARTESIAN_POINT ( 'NONE',  ( -3.635086774663250697, 28.08801940460646307, 0.4607281247925576473 ) ) ;
#28158 = CARTESIAN_POINT ( 'NONE',  ( -0.8750585742504035647, 105.9515744484354371, 5.278707647178442208 ) ) ;
#28159 = AXIS2_PLACEMENT_3D ( 'NONE', #33314, #10302, #23270 ) ;
#28160 = AXIS2_PLACEMENT_3D ( 'NONE', #36228, #17658, #30659 ) ;
#28161 = CARTESIAN_POINT ( 'NONE',  ( 3.895047602890354010, -2.730319773039217690, 2.488009491782988469 ) ) ;
#28162 = CARTESIAN_POINT ( 'NONE',  ( 1.617373050801646839, 120.9968702744464366, 0.03231896268895497609 ) ) ;
#28163 = EDGE_CURVE ( 'NONE', #28739, #26298, #401, .T. ) ;
#28164 = CARTESIAN_POINT ( 'NONE',  ( -1.148743315670426535, 1.199490873200159013, 8.378133985588048560 ) ) ;
#28165 = CARTESIAN_POINT ( 'NONE',  ( -57.25386126824266597, 1.903786294961781866, -0.7664973485411553655 ) ) ;
#28166 = CARTESIAN_POINT ( 'NONE',  ( 8.767697749502918469, 117.8781695899573094, -0.2943500221663000183 ) ) ;
#28167 = CARTESIAN_POINT ( 'NONE',  ( -0.3702369378895170593, 122.2435587914033022, -0.3018087652966766066 ) ) ;
#28168 = CIRCLE ( 'NONE', #6413, 0.5080000000000002292 ) ;
#28169 = DIRECTION ( 'NONE',  ( 0.03102909223834449809, -0.9876883405951377704, -0.1533262446135272294 ) ) ;
#28170 = DIRECTION ( 'NONE',  ( 0.8745520943968235761, -0.4849315768086558398, 0.000000000000000000 ) ) ;
#28171 = CARTESIAN_POINT ( 'NONE',  ( 2.951631207686332470, -3.807527625098089175, 7.891363245966695139 ) ) ;
#28172 = CARTESIAN_POINT ( 'NONE',  ( 0.9880450978810132456, 117.9394488772434357, 1.394221648772276501 ) ) ;
#28173 = FACE_BOUND ( 'NONE', #10807, .T. ) ;
#28174 = CARTESIAN_POINT ( 'NONE',  ( 10.86251533436112737, 78.45482716897194564, -1.904999999999999583 ) ) ;
#28175 = CARTESIAN_POINT ( 'NONE',  ( 0.3884485718551349831, 122.8649044353670803, -0.2114733659581321257 ) ) ;
#28176 = CARTESIAN_POINT ( 'NONE',  ( -21.71781664064065609, 151.4054434770023363, 0.2817300504337352240 ) ) ;
#28177 = VERTEX_POINT ( 'NONE', #8976 ) ;
#28178 = CARTESIAN_POINT ( 'NONE',  ( -58.62011547798931588, 0.4741971735572336755, -0.2911429440373615174 ) ) ;
#28179 = ORIENTED_EDGE ( 'NONE', *, *, #24554, .T. ) ;
#28180 = CARTESIAN_POINT ( 'NONE',  ( -20.59944062528794362, 79.83666051618703818, 1.269999999999995133 ) ) ;
#28181 = CARTESIAN_POINT ( 'NONE',  ( -7.045182791479643214, 122.0730096167837075, -0.1019486566929637128 ) ) ;
#28182 = CARTESIAN_POINT ( 'NONE',  ( 6.174787192795118784, -14.39888150296345160, 1.159817306988995211 ) ) ;
#28183 = CARTESIAN_POINT ( 'NONE',  ( -20.47035330145914145, 150.0074677946399504, 1.517022030030165114 ) ) ;
#28184 = CARTESIAN_POINT ( 'NONE',  ( 21.96051921721462463, 150.3855106993079005, -0.8576051660729390180 ) ) ;
#28185 = CARTESIAN_POINT ( 'NONE',  ( 4.585487687326599726, 17.13547844546973309, 0.5842699607688729424 ) ) ;
#28186 = ADVANCED_FACE ( 'NONE', ( #21943 ), #24572, .T. ) ;
#28187 = CARTESIAN_POINT ( 'NONE',  ( -5.814470848032789796, 117.0573985505404693, -0.4185731406947917899 ) ) ;
#28188 = CARTESIAN_POINT ( 'NONE',  ( -58.49576617200561657, -0.01047455392627871275, -0.6956555549625097479 ) ) ;
#28189 = ORIENTED_EDGE ( 'NONE', *, *, #26963, .F. ) ;
#28190 = CARTESIAN_POINT ( 'NONE',  ( -8.798546888910362185, 117.6874511587486580, -0.1190107558871881799 ) ) ;
#28191 = DIRECTION ( 'NONE',  ( -5.188838149069472160E-16, 1.699382548006136559E-16, 1.000000000000000000 ) ) ;
#28192 = CARTESIAN_POINT ( 'NONE',  ( -17.62053193735426859, 147.9903219242534078, 1.529691019407825259 ) ) ;
#28193 = CARTESIAN_POINT ( 'NONE',  ( -48.71914655128158245, 18.21236406733019209, -5.124034746316241673 ) ) ;
#28194 = CARTESIAN_POINT ( 'NONE',  ( 19.30447918735891477, 147.3692480224366079, -1.738561774106543556 ) ) ;
#28195 = CARTESIAN_POINT ( 'NONE',  ( -16.25125256408151131, 125.3309463260932830, -1.843050201054562187 ) ) ;
#28196 = CARTESIAN_POINT ( 'NONE',  ( -50.58884987432006852, 15.93229845861179861, -5.010371253631922706 ) ) ;
#28197 = EDGE_CURVE ( 'NONE', #25412, #20165, #34972, .T. ) ;
#28198 = CARTESIAN_POINT ( 'NONE',  ( 14.11809548624345645, 150.3034377993741657, -0.8008162161465683937 ) ) ;
#28199 = VERTEX_POINT ( 'NONE', #34460 ) ;
#28200 = CARTESIAN_POINT ( 'NONE',  ( -17.90704175211121552, 146.6345634702618952, -2.297399834898016469 ) ) ;
#28201 = CARTESIAN_POINT ( 'NONE',  ( 4.493636945811098293, -15.48460478268967577, 1.406059860741644574 ) ) ;
#28202 = CARTESIAN_POINT ( 'NONE',  ( -4.225035204153935631, 118.2240506214291997, -0.4891602333557787952 ) ) ;
#28203 = CARTESIAN_POINT ( 'NONE',  ( -57.52317756609133426, 3.014644041894651405, -1.981665235817958948 ) ) ;
#28204 = FACE_OUTER_BOUND ( 'NONE', #34614, .T. ) ;
#28205 = CARTESIAN_POINT ( 'NONE',  ( 6.563805965709463841, 120.5225452898634728, 1.124017915699712100 ) ) ;
#28206 = EDGE_CURVE ( 'NONE', #30025, #32851, #25263, .T. ) ;
#28207 = DIRECTION ( 'NONE',  ( -0.8745520943968225769, 0.4849315768086578382, -5.691349986800571545E-16 ) ) ;
#28208 = CARTESIAN_POINT ( 'NONE',  ( -8.092465427151658730, -6.292564624861634037, 2.510960718618908238 ) ) ;
#28209 = CARTESIAN_POINT ( 'NONE',  ( -0.002455802209282870532, 120.8958299794632438, 0.1228983847502211901 ) ) ;
#28210 = DIRECTION ( 'NONE',  ( 0.7770581983690836303, -0.6294287539884032556, 5.101669463485833779E-16 ) ) ;
#28211 = EDGE_CURVE ( 'NONE', #19344, #30808, #8052, .T. ) ;
#28213 = ORIENTED_EDGE ( 'NONE', *, *, #34715, .T. ) ;
#28212 = CARTESIAN_POINT ( 'NONE',  ( -41.35393432493753352, 22.77111593294431913, -0.9171044195162123547 ) ) ;
#28214 = FACE_OUTER_BOUND ( 'NONE', #4463, .T. ) ;
#28215 = CARTESIAN_POINT ( 'NONE',  ( -58.73801720703743001, -0.4998429216807459552, 0.2437502737749395465 ) ) ;
#28216 = CARTESIAN_POINT ( 'NONE',  ( -7.849349869104243815, 122.2537424897477365, -0.7623017139119617758 ) ) ;
#28217 = EDGE_CURVE ( 'NONE', #37727, #21265, #2835, .T. ) ;
#28218 = CARTESIAN_POINT ( 'NONE',  ( -5.871452009091403745, 77.01756249999996840, -5.016499999999999737 ) ) ;
#28219 = CARTESIAN_POINT ( 'NONE',  ( -53.04800011033383811, 17.61732480341419915, 0.3294858417196632749 ) ) ;
#28220 = CARTESIAN_POINT ( 'NONE',  ( -14.80501208800833801, 120.3086691715681695, -0.1403833142216708296 ) ) ;
#28221 = ORIENTED_EDGE ( 'NONE', *, *, #27782, .T. ) ;
#28222 = CARTESIAN_POINT ( 'NONE',  ( -49.72500615219620101, 20.62299186128851858, -2.281585690523513232 ) ) ;
#28223 = CARTESIAN_POINT ( 'NONE',  ( -6.904663929053937999, 121.8518053346438847, -0.4690476237073744614 ) ) ;
#28224 = CARTESIAN_POINT ( 'NONE',  ( -7.880211965457519341, 122.2234151243416989, 0.4724049390182800678 ) ) ;
#28225 = ORIENTED_EDGE ( 'NONE', *, *, #34923, .F. ) ;
#28226 = CARTESIAN_POINT ( 'NONE',  ( 0.8471914301801410918, 115.7028160007855746, -1.722473985426866472 ) ) ;
#28227 = CARTESIAN_POINT ( 'NONE',  ( -5.920896852643748431, 121.5237468798633955, -0.2406035128457658101 ) ) ;
#28228 = CARTESIAN_POINT ( 'NONE',  ( 4.204793715662772158, -14.23101105591234550, 4.663061278791505337 ) ) ;
#28229 = CARTESIAN_POINT ( 'NONE',  ( -21.87558878470086299, 148.2155681941778482, 1.275940291167070306 ) ) ;
#28230 = DIRECTION ( 'NONE',  ( -1.000000000000000000, 0.000000000000000000, 0.000000000000000000 ) ) ;
#28231 = CARTESIAN_POINT ( 'NONE',  ( -0.001838942458919137161, 116.4858755864912183, 0.09202820039585839218 ) ) ;
#28232 = CARTESIAN_POINT ( 'NONE',  ( 0.6412933796112577634, 156.3034662015457741, 0.01281456791805622199 ) ) ;
#28233 = CYLINDRICAL_SURFACE ( 'NONE', #14868, 2.540000000000000480 ) ;
#28234 = CARTESIAN_POINT ( 'NONE',  ( -0.6053885369530382921, 31.17761759867932980, -0.7634260365338448873 ) ) ;
#28235 = CARTESIAN_POINT ( 'NONE',  ( -18.62929286701957565, 154.1293031355326946, -0.4449488992651825514 ) ) ;
#28236 = CARTESIAN_POINT ( 'NONE',  ( -6.654617103318593247E-14, 104.6144662015457243, 1.534725424433578570E-31 ) ) ;
#28237 = FACE_OUTER_BOUND ( 'NONE', #9649, .T. ) ;
#28238 = EDGE_CURVE ( 'NONE', #276, #3703, #8996, .T. ) ;
#28239 = ORIENTED_EDGE ( 'NONE', *, *, #27964, .F. ) ;
#28240 = CIRCLE ( 'NONE', #33030, 0.3810000000000015041 ) ;
#28241 = CARTESIAN_POINT ( 'NONE',  ( -3.476201915147119959, 117.7824304111185825, 0.7268633819961063391 ) ) ;
#28242 = CARTESIAN_POINT ( 'NONE',  ( -5.314278422745059238, 105.1224610256965235, 0.4583187270701644667 ) ) ;
#28243 = CARTESIAN_POINT ( 'NONE',  ( 21.70872022418674163, 149.0176745010074342, 2.143008773150906876 ) ) ;
#28244 = CARTESIAN_POINT ( 'NONE',  ( 13.46871114105383072, 122.4565580348552913, -1.263039180185647314 ) ) ;
#28245 = CARTESIAN_POINT ( 'NONE',  ( 0.5082173563136543892, -13.24086043563247728, -4.610200172643777350 ) ) ;
#28246 = CARTESIAN_POINT ( 'NONE',  ( -12.63141193514832494, 156.8164516032445306, -1.520932111850479274 ) ) ;
#28247 = CARTESIAN_POINT ( 'NONE',  ( 4.909174002396540004, 117.7132343993233690, -0.7287170198434957946 ) ) ;
#28248 = CARTESIAN_POINT ( 'NONE',  ( 5.310592030460657753, 116.9519127983885340, 0.9557578278138696426 ) ) ;
#28249 = CARTESIAN_POINT ( 'NONE',  ( -2.914310908016815471, 156.0868537499222839, 0.09385809996612910766 ) ) ;
#28250 = CARTESIAN_POINT ( 'NONE',  ( -8.504430935371939171, 120.5511696877957775, -1.462663580662433072 ) ) ;
#28251 = CARTESIAN_POINT ( 'NONE',  ( 5.341109902925343711, -14.98078892696824660, 3.412803344283087181 ) ) ;
#28252 = CARTESIAN_POINT ( 'NONE',  ( 4.791633145718989795, 115.6909491485453145, 1.475629664436550526 ) ) ;
#28253 = ADVANCED_FACE ( 'NONE', ( #24640 ), #40954, .F. ) ;
#28254 = CARTESIAN_POINT ( 'NONE',  ( -41.05189575270516400, 23.09451173561986081, -1.524000000000003130 ) ) ;
#28255 = EDGE_CURVE ( 'NONE', #1003, #24894, #4878, .T. ) ;
#28256 = ORIENTED_EDGE ( 'NONE', *, *, #12059, .T. ) ;
#28257 = CARTESIAN_POINT ( 'NONE',  ( 18.63140056563934266, 147.4429432625130119, 2.446051816127022160 ) ) ;
#28258 = CARTESIAN_POINT ( 'NONE',  ( 5.152689472752729039, 116.8412042436348912, 0.1029629964107459106 ) ) ;
#28259 = CARTESIAN_POINT ( 'NONE',  ( -4.794753315118858161, 118.7629491485453599, 0.7450739223749697215 ) ) ;
#28260 = CARTESIAN_POINT ( 'NONE',  ( -0.1833862045737031932, 106.0860833631645193, 5.249533627824055415 ) ) ;
#28261 = CARTESIAN_POINT ( 'NONE',  ( 5.057098040335121780, -7.207523253290371024, 6.778223571298113370 ) ) ;
#28262 = CARTESIAN_POINT ( 'NONE',  ( 14.94204527009761385, 148.8997249754567349, 1.137790122619589450 ) ) ;
#28263 = CARTESIAN_POINT ( 'NONE',  ( -23.43300365160792964, 82.12916405548841681, -1.524000000000006017 ) ) ;
#28264 = AXIS2_PLACEMENT_3D ( 'NONE', #29335, #6140, #41711 ) ;
#28265 = CARTESIAN_POINT ( 'NONE',  ( 4.829765040637122198, 117.0737178285515654, -0.3500672345979854994 ) ) ;
#28266 = CARTESIAN_POINT ( 'NONE',  ( 5.256643466096790895, 56.51500000000020663, -5.296410793414215945 ) ) ;
#28267 = CARTESIAN_POINT ( 'NONE',  ( -58.05509315856782848, 0.3850302431961226679, 0.7835795507822739259 ) ) ;
#28268 = DIRECTION ( 'NONE',  ( -6.353134868986658533E-16, 1.000000000000000000, 0.000000000000000000 ) ) ;
#28269 = EDGE_CURVE ( 'NONE', #30709, #27616, #17140, .T. ) ;
#28270 = DIRECTION ( 'NONE',  ( -0.1906721105965039909, 0.9816537812491094028, -2.657572025465702696E-16 ) ) ;
#28271 = CARTESIAN_POINT ( 'NONE',  ( -4.284176567086307230, 118.2131471502228237, 0.3606148463560187034 ) ) ;
#28272 = CARTESIAN_POINT ( 'NONE',  ( 5.278445427832044068, 115.7725906505842062, -0.7833317346122758984 ) ) ;
#28273 = ADVANCED_FACE ( 'NONE', ( #8890 ), #2089, .T. ) ;
#28274 = EDGE_LOOP ( 'NONE', ( #16129, #25544, #23136, #34721 ) ) ;
#28275 = CARTESIAN_POINT ( 'NONE',  ( -49.01671973967521012, 18.67808020721676954, 5.174630477995038724 ) ) ;
#28276 = CARTESIAN_POINT ( 'NONE',  ( -4.340105779944698483, 119.4684907284004964, -0.9269682760289738033 ) ) ;
#28277 = CARTESIAN_POINT ( 'NONE',  ( 0.09004192032669379453, 116.0444662015457169, -6.160295767268807232 ) ) ;
#28278 = CARTESIAN_POINT ( 'NONE',  ( -4.473455768776904762, 120.9326014760084007, -0.4576173489010090245 ) ) ;
#28279 = DIRECTION ( 'NONE',  ( 4.017660918040594346E-17, -1.000000000000000000, -2.376309959284834438E-19 ) ) ;
#28280 = CARTESIAN_POINT ( 'NONE',  ( -5.684927786827003615, 65.51297084251929448, -1.523999999999993804 ) ) ;
#28281 = ORIENTED_EDGE ( 'NONE', *, *, #18506, .F. ) ;
#28282 = CARTESIAN_POINT ( 'NONE',  ( -2.768688662514669385, 30.30441277318858795, -3.700580903672975541 ) ) ;
#28283 = CARTESIAN_POINT ( 'NONE',  ( -29.91360363449003401, 70.04874496952835727, 1.523999999999991806 ) ) ;
#28284 = DIRECTION ( 'NONE',  ( 0.000000000000000000, 0.000000000000000000, -1.000000000000000000 ) ) ;
#28285 = CARTESIAN_POINT ( 'NONE',  ( -41.77909418349046433, 22.73884196981243377, 1.565812447105980887 ) ) ;
#28286 = CARTESIAN_POINT ( 'NONE',  ( -3.628388194583719468E-14, 57.78499999999999659, 1.904999999999999805 ) ) ;
#28287 = CARTESIAN_POINT ( 'NONE',  ( -6.993568332462578141, 121.9043679937891795, 0.08578656617081802105 ) ) ;
#28288 =( BOUNDED_SURFACE ( )  B_SPLINE_SURFACE ( 3, 2, ( 
 ( #39750, #10338, #7571 ),
 ( #4395, #10547, #10750 ),
 ( #4597, #39532, #23516 ),
 ( #36544, #36750, #20118 ),
 ( #33562, #32930, #33141 ),
 ( #7362, #13538, #13948 ),
 ( #20320, #33347, #3760 ),
 ( #3970, #4177, #40164 ),
 ( #30340, #17141, #1188 ),
 ( #30142, #14149, #10957 ),
 ( #982, #23945, #26945 ),
 ( #39958, #23731, #12613 ),
 ( #25804, #16636, #29212 ),
 ( #55, #32842, #6856 ),
 ( #13455, #13022, #36041 ),
 ( #32418, #32212, #23013 ),
 ( #3248, #3045, #9623 ),
 ( #26442, #29644, #26015 ),
 ( #39446, #6233, #3672 ),
 ( #7075, #38810, #9832 ),
 ( #10249, #481, #29002 ),
 ( #19204, #25600, #35623 ),
 ( #22591, #28802, #16423 ),
 ( #16208, #22799, #39024 ),
 ( #19826, #3460, #20038 ),
 ( #6437, #42019, #23221 ),
 ( #16003, #36253, #26227 ),
 ( #35834, #12816, #32627 ),
 ( #19411, #6650, #19614 ),
 ( #29428, #269, #13243 ),
 ( #39231, #33057, #10040 ),
 ( #3887, #41819, #38608 ),
 ( #9414, #22380, #35406 ),
 ( #4099, #36463, #33692 ),
 ( #17058, #37092, #11093 ),
 ( #30061, #26653, #39874 ),
 ( #7910, #40506, #17681 ),
 ( #39660, #10670, #29852 ),
 ( #8109, #898, #4516 ),
 ( #30475, #14073, #10881 ),
 ( #23651, #4311, #4729 ),
 ( #36673, #13873, #14486 ) ),
 .UNSPECIFIED., .F., .F., .T. ) 
 B_SPLINE_SURFACE_WITH_KNOTS ( ( 4, 2, 2, 2, 2, 2, 2, 2, 2, 2, 2, 2, 2, 2, 2, 2, 2, 2, 2, 2, 4 ),
 ( 3, 3 ),
 ( 0.01508659279077888271, 0.01602950484020540523, 0.01697241688963192774, 0.01744387291434518900, 0.01791532893905845025, 0.01885824098848497624, 0.01980115303791150222, 0.02027260906262476348, 0.02074406508733802473, 0.02168697713676454725, 0.02262988918619106976, 0.02357280123561759227, 0.02451571328504411826, 0.02498716930975738298, 0.02545862533447064424, 0.02640153738389716676, 0.02734444943332368927, 0.02828736148275021178, 0.02875881750746347304, 0.02923027353217673430, 0.03017318558160326028 ),
 ( 0.000000000000000000, 1.000000000000000000 ),
 .UNSPECIFIED. ) 
 GEOMETRIC_REPRESENTATION_ITEM ( )  RATIONAL_B_SPLINE_SURFACE ( (
 ( 1.000000000000000000, 0.7071072175333618093, 1.000000000000000000),
 ( 1.000000000000000000, 0.7071125701626851390, 1.000000000000000000),
 ( 1.000000000000000000, 0.7070885819517980231, 1.000000000000000000),
 ( 1.000000000000000000, 0.7071155700417062206, 1.000000000000000000),
 ( 1.000000000000000000, 0.7072884777352917984, 1.000000000000000000),
 ( 1.000000000000000000, 0.7075382887060654991, 1.000000000000000000),
 ( 1.000000000000000000, 0.7076187781276516153, 1.000000000000000000),
 ( 1.000000000000000000, 0.7077331820335120982, 1.000000000000000000),
 ( 1.000000000000000000, 0.7077675007750334757, 1.000000000000000000),
 ( 1.000000000000000000, 0.7077686675487847578, 1.000000000000000000),
 ( 1.000000000000000000, 0.7076263510399570800, 1.000000000000000000),
 ( 1.000000000000000000, 0.7070463795844047494, 1.000000000000000000),
 ( 1.000000000000000000, 0.7066053812610246787, 1.000000000000000000),
 ( 1.000000000000000000, 0.7061250891750091574, 1.000000000000000000),
 ( 1.000000000000000000, 0.7059929351571929690, 1.000000000000000000),
 ( 1.000000000000000000, 0.7058117510952008899, 1.000000000000000000),
 ( 1.000000000000000000, 0.7057630826365799415, 1.000000000000000000),
 ( 1.000000000000000000, 0.7057465095916261033, 1.000000000000000000),
 ( 1.000000000000000000, 0.7059103451324751921, 1.000000000000000000),
 ( 1.000000000000000000, 0.7063930724344579248, 1.000000000000000000),
 ( 1.000000000000000000, 0.7067109810593208419, 1.000000000000000000),
 ( 1.000000000000000000, 0.7071150251610267556, 1.000000000000000000),
 ( 1.000000000000000000, 0.7071578580764347199, 1.000000000000000000),
 ( 1.000000000000000000, 0.7068314760137596187, 1.000000000000000000),
 ( 1.000000000000000000, 0.7065268676894724820, 1.000000000000000000),
 ( 1.000000000000000000, 0.7061479767406342312, 1.000000000000000000),
 ( 1.000000000000000000, 0.7060332234545864116, 1.000000000000000000),
 ( 1.000000000000000000, 0.7058611809846090379, 1.000000000000000000),
 ( 1.000000000000000000, 0.7058040174201852812, 1.000000000000000000),
 ( 1.000000000000000000, 0.7057564474746290673, 1.000000000000000000),
 ( 1.000000000000000000, 0.7058984215012326091, 1.000000000000000000),
 ( 1.000000000000000000, 0.7064705227655466713, 1.000000000000000000),
 ( 1.000000000000000000, 0.7069135182905013082, 1.000000000000000000),
 ( 1.000000000000000000, 0.7075440222900022391, 1.000000000000000000),
 ( 1.000000000000000000, 0.7077280451744416556, 1.000000000000000000),
 ( 1.000000000000000000, 0.7077773545919098241, 1.000000000000000000),
 ( 1.000000000000000000, 0.7077573002275580061, 1.000000000000000000),
 ( 1.000000000000000000, 0.7076645137286782239, 1.000000000000000000),
 ( 1.000000000000000000, 0.7075922911518204295, 1.000000000000000000),
 ( 1.000000000000000000, 0.7073505092953880080, 1.000000000000000000),
 ( 1.000000000000000000, 0.7071543910050398507, 1.000000000000000000),
 ( 1.000000000000000000, 0.7071103834195795468, 1.000000000000000000) ) ) 
 REPRESENTATION_ITEM ( '' )  SURFACE ( )  );
#28289 = CARTESIAN_POINT ( 'NONE',  ( 14.73199999999999577, 61.59499999999999886, 1.904999999999990479 ) ) ;
#28290 = CARTESIAN_POINT ( 'NONE',  ( 17.76144578550747966, 125.1550653296939970, 1.296339218450673014 ) ) ;
#28291 = CARTESIAN_POINT ( 'NONE',  ( 3.865556019884660799, 104.6144662015457243, -2.894260390300009256 ) ) ;
#28293 = CARTESIAN_POINT ( 'NONE',  ( 2.888962495634898708, 158.8946464937287999, -1.317949658345221708 ) ) ;
#28292 = CARTESIAN_POINT ( 'NONE',  ( 3.187143392547471255, -14.52651900126690876, 3.212499789951002604 ) ) ;
#28294 = CARTESIAN_POINT ( 'NONE',  ( -18.13417818756210664, 144.6555253171603397, 1.679261103697791135 ) ) ;
#28295 = CARTESIAN_POINT ( 'NONE',  ( 3.287934792154566299, 21.71798121574904172, 3.254339964430349230 ) ) ;
#28296 = CARTESIAN_POINT ( 'NONE',  ( -15.38106892591223662, 121.3506620944898060, -1.079669858139658212 ) ) ;
#28297 = CARTESIAN_POINT ( 'NONE',  ( 0.8366737682863060188, 2.078006455476229419, 0.4978880095337852585 ) ) ;
#28298 = ORIENTED_EDGE ( 'NONE', *, *, #34244, .F. ) ;
#28299 = CARTESIAN_POINT ( 'NONE',  ( -57.23135758994266098, 1.814875683430833275, 0.2588789259697444889 ) ) ;
#28300 = AXIS2_PLACEMENT_3D ( 'NONE', #41986, #24941, #6202 ) ;
#28301 = CARTESIAN_POINT ( 'NONE',  ( -15.92039698932596892, 146.6311637152522565, 0.2762755564230132133 ) ) ;
#28302 = CARTESIAN_POINT ( 'NONE',  ( 5.392686582494618186, -13.55334589181164695, 3.069518437182660264 ) ) ;
#28303 = CARTESIAN_POINT ( 'NONE',  ( 0.8098364334000902609, 156.6562795458349910, -1.088908734543432955 ) ) ;
#28304 = ORIENTED_EDGE ( 'NONE', *, *, #26623, .T. ) ;
#28305 = CARTESIAN_POINT ( 'NONE',  ( 2.661383351097782679, 115.7033367011135709, 1.688185195617331713 ) ) ;
#28306 = ORIENTED_EDGE ( 'NONE', *, *, #18066, .F. ) ;
#28307 = CARTESIAN_POINT ( 'NONE',  ( -4.772391204760736194, 117.7363031211461220, -1.071217607564205698 ) ) ;
#28308 = CARTESIAN_POINT ( 'NONE',  ( 7.552512487614144732, 122.4261604937442485, 0.1509171734833088807 ) ) ;
#28309 = ORIENTED_EDGE ( 'NONE', *, *, #24064, .T. ) ;
#28310 = CARTESIAN_POINT ( 'NONE',  ( 6.695514854630599366, 119.3011930948910759, 1.284729283498812658 ) ) ;
#28311 = CARTESIAN_POINT ( 'NONE',  ( 13.85159022459153810, 60.48513866567135722, -5.016500000000000625 ) ) ;
#28312 = CARTESIAN_POINT ( 'NONE',  ( 5.817775060672807363, 56.51500000000000057, 4.384522920466269014 ) ) ;
#28313 = CARTESIAN_POINT ( 'NONE',  ( 4.915642170617802620, 117.4785366793690571, -0.9402594631468037534 ) ) ;
#28314 = B_SPLINE_CURVE_WITH_KNOTS ( 'NONE', 3,
 ( #8670, #27625, #2509, #8245 ),
 .UNSPECIFIED., .F., .F.,
 ( 4, 4 ),
 ( 0.000000000000000000, 0.4003840206711454242 ),
 .UNSPECIFIED. ) ;
#28315 = CARTESIAN_POINT ( 'NONE',  ( 13.38634958471956438, 156.9592627042916604, -0.007429229355843724146 ) ) ;
#28316 = CARTESIAN_POINT ( 'NONE',  ( 0.04257260547685356306, 114.5099076536771321, -2.130507264987491212 ) ) ;
#28317 = CARTESIAN_POINT ( 'NONE',  ( 4.842662086898184448, 118.7629491485453030, 0.3780004892236683567 ) ) ;
#28318 = CARTESIAN_POINT ( 'NONE',  ( 1.664631964234967842, -15.26880034211669468, 5.559520488082625000 ) ) ;
#28319 = CARTESIAN_POINT ( 'NONE',  ( -46.30033180095409762, 21.65562830348028456, 4.292083522273594909 ) ) ;
#28320 = CARTESIAN_POINT ( 'NONE',  ( -10.86251533436120553, 78.45482716897194564, 1.904999999999999583 ) ) ;
#28321 = AXIS2_PLACEMENT_3D ( 'NONE', #491, #5568, #11511 ) ;
#28322 = CARTESIAN_POINT ( 'NONE',  ( -4.764223389954819865, 117.8480438172858840, 0.8126175582787710239 ) ) ;
#28323 = CIRCLE ( 'NONE', #14060, 16.60960244842765121 ) ;
#28324 = ORIENTED_EDGE ( 'NONE', *, *, #8732, .F. ) ;
#28325 = VERTEX_POINT ( 'NONE', #40448 ) ;
#28326 = CARTESIAN_POINT ( 'NONE',  ( -1.413722513147405824, 118.7629491485454025, 1.196428764754537299 ) ) ;
#28327 = CARTESIAN_POINT ( 'NONE',  ( -2.731950974749316252, 117.8398921135531481, -0.8256334691123825564 ) ) ;
#28328 = CARTESIAN_POINT ( 'NONE',  ( -6.931894935422283410, 124.3275308867733600, -0.1497658092569640054 ) ) ;
#28329 = CARTESIAN_POINT ( 'NONE',  ( 4.853897125124975176, 117.7484357747367198, 0.9336096688446040570 ) ) ;
#28330 = CARTESIAN_POINT ( 'NONE',  ( 3.116451998213339625, -14.00698646007624149, 1.619014592372306716 ) ) ;
#28331 = CARTESIAN_POINT ( 'NONE',  ( -0.8881552493051317887, 122.2453746293775652, 0.2465857446897833649 ) ) ;
#28332 = CARTESIAN_POINT ( 'NONE',  ( -3.594857975007920814, -7.703025367003809798, -2.923569511714296798 ) ) ;
#28333 = CARTESIAN_POINT ( 'NONE',  ( 4.921840205057578466, 117.4109437077822946, -0.9481957113721782848 ) ) ;
#28334 = CARTESIAN_POINT ( 'NONE',  ( -5.475330206976868119, 57.14999999999997016, -5.107412922131463695 ) ) ;
#28335 = CARTESIAN_POINT ( 'NONE',  ( 3.666546702136318725, -13.72720857325485078, 3.759896688191319836 ) ) ;
#28336 = CARTESIAN_POINT ( 'NONE',  ( 5.326805317745445301, 116.9650601603920279, -0.7421267338694929050 ) ) ;
#28337 = CARTESIAN_POINT ( 'NONE',  ( -3.428210029137864101, 119.9243055703230851, -0.7605957222121785266 ) ) ;
#28338 = DIRECTION ( 'NONE',  ( 0.01997839162482749689, 1.040247600000945640E-18, -0.9998004120163610509 ) ) ;
#28339 = CARTESIAN_POINT ( 'NONE',  ( -4.873850642958228008, 32.38564726215445688, 3.744354677719523572 ) ) ;
#28340 = CARTESIAN_POINT ( 'NONE',  ( -1.895780330261635394, 115.7029491485453434, 1.647506384871404217 ) ) ;
#28341 = CARTESIAN_POINT ( 'NONE',  ( -2.359559261509405204, 14.11188314818778444, 3.974389579228013503 ) ) ;
#28343 = ORIENTED_EDGE ( 'NONE', *, *, #42049, .F. ) ;
#28342 = CARTESIAN_POINT ( 'NONE',  ( 3.233108093638791924, 159.4494809562368971, 0.4325382840285663111 ) ) ;
#28344 = CARTESIAN_POINT ( 'NONE',  ( -1.150407940190810052, 104.6144662015545777, -5.220267424023966818 ) ) ;
#28345 = CARTESIAN_POINT ( 'NONE',  ( 4.136722333222721204, -15.50381924862055705, 2.038268645697551396 ) ) ;
#28346 = CARTESIAN_POINT ( 'NONE',  ( -19.58040708638642613, 147.7952244890416296, 1.737278836974155416 ) ) ;
#28347 = CARTESIAN_POINT ( 'NONE',  ( 0.6786060095046909657, 20.86726683125115756, 0.6988831909418605770 ) ) ;
#28348 = CARTESIAN_POINT ( 'NONE',  ( -0.9394305312890779414, 22.53537758578342931, -0.2615529312561373776 ) ) ;
#28349 = EDGE_LOOP ( 'NONE', ( #7855, #41999, #38886, #2981 ) ) ;
#28350 = ORIENTED_EDGE ( 'NONE', *, *, #28255, .T. ) ;
#28351 = CARTESIAN_POINT ( 'NONE',  ( -4.948517985667383101, 117.5250047935927995, -0.9665297271245709698 ) ) ;
#28352 = CARTESIAN_POINT ( 'NONE',  ( 0.4858112859842325659, 106.1608668108878817, 5.224277761219202176 ) ) ;
#28353 = DIRECTION ( 'NONE',  ( 1.000000000000000000, 0.000000000000000000, 0.000000000000000000 ) ) ;
#28354 = CARTESIAN_POINT ( 'NONE',  ( -15.90968206782444128, 148.0001117310855250, 0.7891277450764204726 ) ) ;
#28355 = DIRECTION ( 'NONE',  ( 0.01731298258488073519, -0.9998501190848635423, 1.788962107505278613E-16 ) ) ;
#28356 = CARTESIAN_POINT ( 'NONE',  ( 3.206936388013850614, -12.21552616865279006, 0.5380348851386724807 ) ) ;
#28357 = CARTESIAN_POINT ( 'NONE',  ( 10.76835564757999819, 122.7614441063800399, -1.139041423164458111 ) ) ;
#28358 = VECTOR ( 'NONE', #9966, 999.9999999999998863 ) ;
#28359 = CARTESIAN_POINT ( 'NONE',  ( -4.966515250750420662, 118.7197616721209670, -1.086191325688556697 ) ) ;
#28360 = CARTESIAN_POINT ( 'NONE',  ( 10.28897677580358305, 57.15000000000000568, -4.381499999999999950 ) ) ;
#28361 = CARTESIAN_POINT ( 'NONE',  ( 8.438889187357746735, 119.3200643466248465, 1.362719739275324526 ) ) ;
#28362 = CARTESIAN_POINT ( 'NONE',  ( 4.074910602682932925, 118.2429491485453354, -0.1454311599470142491 ) ) ;
#28363 = CARTESIAN_POINT ( 'NONE',  ( 1.578387894090330645, 120.8584627942791627, -0.1358179495115141855 ) ) ;
#28364 = AXIS2_PLACEMENT_3D ( 'NONE', #8368, #37339, #27545 ) ;
#28365 = ORIENTED_EDGE ( 'NONE', *, *, #16264, .T. ) ;
#28366 = CARTESIAN_POINT ( 'NONE',  ( -0.9489272475186022460, 106.1802426532330514, -5.207839528941200058 ) ) ;
#28367 = CYLINDRICAL_SURFACE ( 'NONE', #24470, 0.2539999999999973390 ) ;
#28368 = CARTESIAN_POINT ( 'NONE',  ( -1.879194370357706756, 31.42354579518680424, 3.981814511614890417 ) ) ;
#28369 = CARTESIAN_POINT ( 'NONE',  ( -58.63679809531443965, -0.7731007215655836262, -1.422417852365874970E-12 ) ) ;
#28370 = CARTESIAN_POINT ( 'NONE',  ( 4.581731014592691054, -15.30239759458089388, -0.5121113081912510578 ) ) ;
#28371 = CARTESIAN_POINT ( 'NONE',  ( 16.63795227869222515, 147.2809512400332608, 1.774228895505126413 ) ) ;
#28372 = CARTESIAN_POINT ( 'NONE',  ( -6.631541954483209765E-14, 98.39146620154573952, -1.863789202389766375E-18 ) ) ;
#28373 = CARTESIAN_POINT ( 'NONE',  ( 15.69674027099051195, 120.8333755831694702, 0.2629491152481264193 ) ) ;
#28374 = CARTESIAN_POINT ( 'NONE',  ( -7.614108603649571094, 124.2930771091975117, -0.1432033155151095360 ) ) ;
#28375 = AXIS2_PLACEMENT_3D ( 'NONE', #12887, #9693, #25671 ) ;
#28376 = CARTESIAN_POINT ( 'NONE',  ( 2.829288187452689396, 6.340478445469713620, 3.655570690059357197 ) ) ;
#28377 = CARTESIAN_POINT ( 'NONE',  ( 15.64207015331054862, 147.2204672151589193, 0.3125657877211908686 ) ) ;
#28378 = CARTESIAN_POINT ( 'NONE',  ( -6.568537450833661140, -2.023721358670699466, -5.272568914532883788 ) ) ;
#28379 = CARTESIAN_POINT ( 'NONE',  ( -57.41561397472474937, 1.705883423724310788, -1.231064337386920782 ) ) ;
#28380 = CARTESIAN_POINT ( 'NONE',  ( 8.760849894608837118, 117.9156266018594579, -0.3360442439942614157 ) ) ;
#28381 = AXIS2_PLACEMENT_3D ( 'NONE', #5911, #18872, #3341 ) ;
#28382 = CARTESIAN_POINT ( 'NONE',  ( -0.4066243552753486257, 124.0591982226670211, -0.1013866577921579831 ) ) ;
#28383 = CARTESIAN_POINT ( 'NONE',  ( 5.586884702347364673, 79.34146620154574236, 0.1116392523995368424 ) ) ;
#28384 = CARTESIAN_POINT ( 'NONE',  ( -17.08598887363762131, 83.79821757228496892, 1.269999999999996243 ) ) ;
#28385 = CARTESIAN_POINT ( 'NONE',  ( 2.163044864548389956, 28.58015952483584954, -4.087059112497700042 ) ) ;
#28386 = CARTESIAN_POINT ( 'NONE',  ( 2.756409082185796056, 117.3993815990797458, 1.414652500441052396 ) ) ;
#28387 = FACE_OUTER_BOUND ( 'NONE', #14877, .T. ) ;
#28388 = CARTESIAN_POINT ( 'NONE',  ( -58.83227707057485389, -0.08366279997994163775, -1.533110566128065488E-14 ) ) ;
#28389 = CARTESIAN_POINT ( 'NONE',  ( 0.3351388899280297595, 111.5577547982948801, -3.138814863473581518 ) ) ;
#28390 = CARTESIAN_POINT ( 'NONE',  ( -23.09108451844700838, 149.2510847660714148, 0.2673146292145804348 ) ) ;
#28391 = VECTOR ( 'NONE', #36265, 1000.000000000000114 ) ;
#28392 = EDGE_LOOP ( 'NONE', ( #3521, #20324, #39097, #16073, #10475, #15467 ) ) ;
#28393 = LINE ( 'NONE', #25194, #23633 ) ;
#28394 = ORIENTED_EDGE ( 'NONE', *, *, #870, .T. ) ;
#28395 = DIRECTION ( 'NONE',  ( -0.4849315768086535083, -0.8745520943968250194, -1.030032898892974695E-16 ) ) ;
#28396 = CARTESIAN_POINT ( 'NONE',  ( -13.59309109316558128, 150.2605162272564030, -0.1417888325812674266 ) ) ;
#28397 = CARTESIAN_POINT ( 'NONE',  ( 4.975685353906630581, -15.32372399918348371, 3.685287151418908724 ) ) ;
#28398 = CARTESIAN_POINT ( 'NONE',  ( -20.75411281516097262, 147.9587796579421308, 1.616985229673752800 ) ) ;
#28399 = CARTESIAN_POINT ( 'NONE',  ( 7.412489149516406250, 158.3992165788449711, -1.135539963648919848 ) ) ;
#28400 = CARTESIAN_POINT ( 'NONE',  ( -3.957843245660688680, 22.95775517496322848, 2.395914033147342970 ) ) ;
#28401 = CARTESIAN_POINT ( 'NONE',  ( -20.19069946793844039, 128.9119615565081176, -0.7900021088785404988 ) ) ;
#28402 = CARTESIAN_POINT ( 'NONE',  ( -57.58628444390482315, 1.951741080605158718, -1.744151961578425780 ) ) ;
#28403 = ORIENTED_EDGE ( 'NONE', *, *, #15276, .F. ) ;
#28404 = CARTESIAN_POINT ( 'NONE',  ( -0.001261869788360067647, 124.3520329708341876, 0.06314912420803703297 ) ) ;
#28405 = CARTESIAN_POINT ( 'NONE',  ( -5.816409885615420272, 28.29835777331257063, 0.3468669796613692569 ) ) ;
#28406 = CARTESIAN_POINT ( 'NONE',  ( -7.304865317682213366, 121.1388872696715282, 0.8066302172824781902 ) ) ;
#28407 = CARTESIAN_POINT ( 'NONE',  ( -50.96693996911965741, 14.52141170389602998, -4.551080797630170593 ) ) ;
#28408 = CARTESIAN_POINT ( 'NONE',  ( 6.663576545388588457, 119.9895581359321994, -0.9799952387295396417 ) ) ;
#28409 = CARTESIAN_POINT ( 'NONE',  ( -0.4013927055963539270, 117.8786474493541050, -0.5472391114537519252 ) ) ;
#28410 = CARTESIAN_POINT ( 'NONE',  ( -56.82628769568140115, 4.502340570254503405, -2.499646007873257414 ) ) ;
#28411 = CIRCLE ( 'NONE', #10030, 0.5079999999999946780 ) ;
#28412 = CARTESIAN_POINT ( 'NONE',  ( 5.884536728137893746, 121.1554468101848130, -0.4284271420130266184 ) ) ;
#28413 = EDGE_LOOP ( 'NONE', ( #37805, #14428 ) ) ;
#28414 = CARTESIAN_POINT ( 'NONE',  ( -17.82368987960366269, 147.7668373613703352, -2.290061161587756633 ) ) ;
#28415 = CARTESIAN_POINT ( 'NONE',  ( 3.437591410214265064, -15.71306207096091789, 4.322042152151218453 ) ) ;
#28416 = CARTESIAN_POINT ( 'NONE',  ( -4.065972646788793554, 118.2429491485452928, -0.3080848862740693250 ) ) ;
#28417 = CARTESIAN_POINT ( 'NONE',  ( -58.70413935429054675, 0.2332485698458008905, -0.6626129746612972049 ) ) ;
#28418 = CARTESIAN_POINT ( 'NONE',  ( -4.816142268852273034, 117.5417147180202022, 0.9796457938337586047 ) ) ;
#28419 = CARTESIAN_POINT ( 'NONE',  ( 12.73281086834426290, 125.9836878220586556, 1.772748636948829004 ) ) ;
#28420 = DIRECTION ( 'NONE',  ( -0.000000000000000000, -0.000000000000000000, -1.000000000000000000 ) ) ;
#28421 = EDGE_CURVE ( 'NONE', #24097, #28898, #17833, .T. ) ;
#28422 = CARTESIAN_POINT ( 'NONE',  ( -7.992722778381481596, -7.251515252772184894, -2.728257467986670903 ) ) ;
#28423 = CARTESIAN_POINT ( 'NONE',  ( 15.76594527475406338, 145.7191243368997675, 0.6468106390071733935 ) ) ;
#28424 = CARTESIAN_POINT ( 'NONE',  ( -17.58995245299101029, 75.15621874538170744, 1.523999999999997801 ) ) ;
#28425 = CARTESIAN_POINT ( 'NONE',  ( -41.05189575270517111, 23.09451173561986792, -0.08466666666667251040 ) ) ;
#28426 = DIRECTION ( 'NONE',  ( -5.188838149069472160E-16, 1.699382548006136559E-16, 1.000000000000000000 ) ) ;
#28427 = CARTESIAN_POINT ( 'NONE',  ( -57.67794393518098417, 1.927849678527493449, 1.763631237166035648 ) ) ;
#28428 = CARTESIAN_POINT ( 'NONE',  ( -51.14897750729640080, 14.40149654946681501, 4.652905086514556920 ) ) ;
#28429 = CARTESIAN_POINT ( 'NONE',  ( -10.18297664959815663, 77.66688486464208552, -1.523999999999998245 ) ) ;
#28430 = STYLED_ITEM ( 'NONE', ( #7303 ), #41738 ) ;
#28431 = CARTESIAN_POINT ( 'NONE',  ( 12.69999999999999929, 17.14499999999999957, 1.555301434917138235E-15 ) ) ;
#28432 = CARTESIAN_POINT ( 'NONE',  ( -52.14602366315243387, 18.74265329119796064, 0.7451446608535526872 ) ) ;
#28433 = EDGE_CURVE ( 'NONE', #19034, #5073, #143, .T. ) ;
#28434 = CARTESIAN_POINT ( 'NONE',  ( -5.742584425896393618, 159.1207877133979309, -0.01316620519284343246 ) ) ;
#28435 = ORIENTED_EDGE ( 'NONE', *, *, #18057, .T. ) ;
#28436 = CARTESIAN_POINT ( 'NONE',  ( -49.25189787529244967, 18.82624764011888630, -4.709232814563292457 ) ) ;
#28437 = CARTESIAN_POINT ( 'NONE',  ( 6.965125855778357078, 121.9452357174143913, 0.01188280683295246491 ) ) ;
#28438 = CARTESIAN_POINT ( 'NONE',  ( -8.323020013683432694, 120.1269634747937971, 1.118279847563952600 ) ) ;
#28439 = VERTEX_POINT ( 'NONE', #11239 ) ;
#28440 = CARTESIAN_POINT ( 'NONE',  ( 2.241029890824462356, 115.7026179593451616, -1.621430037521891077 ) ) ;
#28441 = CARTESIAN_POINT ( 'NONE',  ( -13.60737276370619675, 150.2179846313823930, -0.4949411041190264759 ) ) ;
#28442 = CARTESIAN_POINT ( 'NONE',  ( 4.326150682005948767, -14.13415638199089130, 4.511655897031580764 ) ) ;
#28443 = CARTESIAN_POINT ( 'NONE',  ( -0.02399864187742892577, 159.1630378086529731, 1.200990174154242585 ) ) ;
#28444 = CARTESIAN_POINT ( 'NONE',  ( 3.222064683888731018, 117.3993833697546449, -1.271138870486020478 ) ) ;
#28445 = PRESENTATION_LAYER_ASSIGNMENT (  '', '', ( #41382 ) ) ;
#28446 = CARTESIAN_POINT ( 'NONE',  ( 2.778732907383107520, 116.5968896900294709, 0.2040764120049697039 ) ) ;
#28447 = CARTESIAN_POINT ( 'NONE',  ( 15.63990901280855716, 147.2221586356311036, 0.4463020126745949057 ) ) ;
#28448 = DIRECTION ( 'NONE',  ( -5.188838149069472160E-16, 1.699382548006136559E-16, 1.000000000000000000 ) ) ;
#28449 = CARTESIAN_POINT ( 'NONE',  ( -0.3507176028818052571, 11.51684809748499028, -0.9106068057588879716 ) ) ;
#28450 = CARTESIAN_POINT ( 'NONE',  ( -16.85465591277215225, 155.2173118157008673, -0.4068649486066868715 ) ) ;
#28451 = CARTESIAN_POINT ( 'NONE',  ( 1.167505706004672243E-15, 11.53894877578617084, 0.000000000000000000 ) ) ;
#28452 = FACE_OUTER_BOUND ( 'NONE', #28392, .T. ) ;
#28453 = ORIENTED_EDGE ( 'NONE', *, *, #27489, .F. ) ;
#28454 = CARTESIAN_POINT ( 'NONE',  ( 8.360143117074091634, 119.6977532042923968, 1.428540289422721488 ) ) ;
#28455 = DIRECTION ( 'NONE',  ( -5.188838149069472160E-16, 1.699382548006136559E-16, 1.000000000000000000 ) ) ;
#28456 = CARTESIAN_POINT ( 'NONE',  ( 1.196040046930053613, 159.0162744061759099, 1.350631977726330701 ) ) ;
#28457 = CARTESIAN_POINT ( 'NONE',  ( 2.650128318467419586, 158.3255140430775043, -1.577873239259485638 ) ) ;
#28458 = CARTESIAN_POINT ( 'NONE',  ( -8.406874004389072397, 27.76653542065474056, -0.1818807619882521764 ) ) ;
#28459 = CARTESIAN_POINT ( 'NONE',  ( -14.69745991766254001, 121.6338672040446767, -1.430666218478179763 ) ) ;
#28460 = CARTESIAN_POINT ( 'NONE',  ( 4.797366694452281699, 117.7649354367249401, -0.8643881762267181523 ) ) ;
#28461 = CARTESIAN_POINT ( 'NONE',  ( 5.384759902136762477, 117.1811293437636721, 0.8990931802006212337 ) ) ;
#28462 = EDGE_CURVE ( 'NONE', #31901, #5241, #23906, .T. ) ;
#28463 = CARTESIAN_POINT ( 'NONE',  ( -7.821695933845212778, 154.6216606121152495, 0.03501689623823082270 ) ) ;
#28464 = CARTESIAN_POINT ( 'NONE',  ( -5.016192601342632784, 119.3892302351119810, -1.087184205914811352 ) ) ;
#28465 = EDGE_CURVE ( 'NONE', #15805, #15736, #40276, .T. ) ;
#28466 = CARTESIAN_POINT ( 'NONE',  ( 2.845652327410156612, -15.51977306057959716, 5.689769116265302351 ) ) ;
#28467 = DIRECTION ( 'NONE',  ( 0.000000000000000000, 1.000000000000000000, 0.000000000000000000 ) ) ;
#28468 = EDGE_CURVE ( 'NONE', #39579, #17268, #38224, .T. ) ;
#28469 = CARTESIAN_POINT ( 'NONE',  ( -43.93316818929329770, 24.49458088220322338, -1.524000000000007349 ) ) ;
#28470 = ORIENTED_EDGE ( 'NONE', *, *, #2814, .T. ) ;
#28471 = CARTESIAN_POINT ( 'NONE',  ( 18.57470247777319727, 148.7425187291823363, 2.467219961595396693 ) ) ;
#28472 = CARTESIAN_POINT ( 'NONE',  ( -28.60507221318228943, 76.72702915747851193, -1.524000000000007793 ) ) ;
#28473 = CIRCLE ( 'NONE', #10099, 0.2539999999999998925 ) ;
#28474 = CIRCLE ( 'NONE', #6055, 0.2540000000000000036 ) ;
#28475 = CYLINDRICAL_SURFACE ( 'NONE', #31373, 6.350000000000004974 ) ;
#28476 = CARTESIAN_POINT ( 'NONE',  ( -1.859996092182737426, 121.3688471916803451, 0.2894809034927953717 ) ) ;
#28477 = CARTESIAN_POINT ( 'NONE',  ( -8.165053131321412749, -1.372107735949496421, -2.092221094348168275 ) ) ;
#28478 = CARTESIAN_POINT ( 'NONE',  ( 9.461503173624029372, 123.8597080710187015, 0.7891915900027409725 ) ) ;
#28479 = CARTESIAN_POINT ( 'NONE',  ( 22.84463062875807893, 149.4631731099488832, -0.5130293307460864760 ) ) ;
#28480 = DIRECTION ( 'NONE',  ( 0.3582377630123958490, -0.9336303900108837706, 3.445432962228686790E-16 ) ) ;
#28481 = CARTESIAN_POINT ( 'NONE',  ( -58.29410838023627406, -0.1313788046413840727, 0.3526482289038367912 ) ) ;
#28482 = CARTESIAN_POINT ( 'NONE',  ( 5.423544988499409136, 78.92590603608628896, 5.135347845727595839 ) ) ;
#28483 = CARTESIAN_POINT ( 'NONE',  ( 5.586884702347364673, 81.62746620154572952, 0.1116392523995368424 ) ) ;
#28484 = LINE ( 'NONE', #18459, #11794 ) ;
#28485 = VERTEX_POINT ( 'NONE', #25070 ) ;
#28486 = CARTESIAN_POINT ( 'NONE',  ( 8.247687365870664422, 120.4923382035136683, -1.097851349060563475 ) ) ;
#28487 = CARTESIAN_POINT ( 'NONE',  ( -5.332935397695335311, 104.6144662015457385, -0.1065647409268299373 ) ) ;
#28488 = CARTESIAN_POINT ( 'NONE',  ( -3.627630705028967117, 120.8049117488720015, -0.4115075270184372358 ) ) ;
#28489 = CARTESIAN_POINT ( 'NONE',  ( 23.29064488658015719, 149.3519930085110161, 0.4911336289882584638 ) ) ;
#28490 = ORIENTED_EDGE ( 'NONE', *, *, #32859, .F. ) ;
#28491 = CARTESIAN_POINT ( 'NONE',  ( 4.458631606973747274, 16.91056413504885825, 1.251853190366734259 ) ) ;
#28492 = FACE_OUTER_BOUND ( 'NONE', #26716, .T. ) ;
#28493 = CARTESIAN_POINT ( 'NONE',  ( -8.078287538471746743, 158.6595088495342338, -0.1614234102745197019 ) ) ;
#28494 = DIRECTION ( 'NONE',  ( -0.9998004120163609398, 0.000000000000000000, -0.01997839162482749689 ) ) ;
#28495 = DIRECTION ( 'NONE',  ( 0.1951894777626611566, 0.9807655518882887336, 0.000000000000000000 ) ) ;
#28496 = CARTESIAN_POINT ( 'NONE',  ( -7.785084361432222266, 122.6279490200930837, -0.1367715089808489159 ) ) ;
#28497 = AXIS2_PLACEMENT_3D ( 'NONE', #18248, #21864, #14848 ) ;
#28498 = CARTESIAN_POINT ( 'NONE',  ( 1.027636191897724816, 24.96647085856908177, -4.506105791511280323 ) ) ;
#28499 = EDGE_CURVE ( 'NONE', #11997, #1559, #23272, .T. ) ;
#28500 = CARTESIAN_POINT ( 'NONE',  ( 16.38310316169952330, 155.2191194103077407, 1.312707330359597524 ) ) ;
#28501 = FACE_OUTER_BOUND ( 'NONE', #15293, .T. ) ;
#28503 = CARTESIAN_POINT ( 'NONE',  ( 9.669117252159342257, 157.4977751962898083, -1.392273965589622353 ) ) ;
#28502 = CARTESIAN_POINT ( 'NONE',  ( 0.1568724191532814560, 105.9762912437439155, 5.300943958216106644 ) ) ;
#28504 = CARTESIAN_POINT ( 'NONE',  ( -16.09548914235268313, 150.9843922791743296, 1.671617783681723646 ) ) ;
#28505 = AXIS2_PLACEMENT_3D ( 'NONE', #36949, #10944, #7558 ) ;
#28506 = CARTESIAN_POINT ( 'NONE',  ( 2.794707274389933715, 24.31675177525179876, -3.679445548267922916 ) ) ;
#28507 = CARTESIAN_POINT ( 'NONE',  ( 0.01133159106138491301, 159.5297144918048673, -0.5670791535570575137 ) ) ;
#28508 = CARTESIAN_POINT ( 'NONE',  ( -0.9353260110528880400, 8.126651709021682990, 0.2714574413461035007 ) ) ;
#28509 = EDGE_LOOP ( 'NONE', ( #17239, #35438, #33535, #15852 ) ) ;
#28510 = CARTESIAN_POINT ( 'NONE',  ( -55.65298819915649631, 5.540485941798498182, 2.823722248809246160 ) ) ;
#28511 = CARTESIAN_POINT ( 'NONE',  ( -2.758537940429013346, 120.8469057251343060, 0.1732774955029140751 ) ) ;
#28512 = EDGE_CURVE ( 'NONE', #41032, #21375, #34888, .T. ) ;
#28513 = CARTESIAN_POINT ( 'NONE',  ( 4.896986379477733742, -14.09362661677580952, 4.057159877996594055 ) ) ;
#28514 = CARTESIAN_POINT ( 'NONE',  ( 10.06555281207532815, 123.2077283916686525, -0.8929836319946561352 ) ) ;
#28515 = ORIENTED_EDGE ( 'NONE', *, *, #30873, .T. ) ;
#28516 = CARTESIAN_POINT ( 'NONE',  ( 0.06879994401897256140, 115.7029491485452581, 1.763577627545462878 ) ) ;
#28517 = ADVANCED_FACE ( 'NONE', ( #19666 ), #34815, .T. ) ;
#28518 = CARTESIAN_POINT ( 'NONE',  ( -4.707492808873059431, 117.7228541735984066, -1.103909285615471081 ) ) ;
#28519 = CARTESIAN_POINT ( 'NONE',  ( 1.563936845556439303, 156.2577446057484281, 0.001723203835320212280 ) ) ;
#28520 = EDGE_LOOP ( 'NONE', ( #9759, #8138, #18365, #25543 ) ) ;
#28521 = CARTESIAN_POINT ( 'NONE',  ( 12.01076045986759233, 121.8643784861682065, 1.757760809232696175 ) ) ;
#28522 = CARTESIAN_POINT ( 'NONE',  ( 7.783246152616065672, 154.6561476914895081, 0.1555277812256516956 ) ) ;
#28523 = DIRECTION ( 'NONE',  ( -0.4849315768086535083, -0.8745520943968250194, -1.030032898892974695E-16 ) ) ;
#28524 = ADVANCED_FACE ( 'NONE', ( #16685 ), #19432, .T. ) ;
#28525 = CARTESIAN_POINT ( 'NONE',  ( 4.848342634033197207, 117.5455766057886393, -0.9616795127513765307 ) ) ;
#28526 = CARTESIAN_POINT ( 'NONE',  ( 22.77159426375455098, 150.3871190066015799, 0.004147128915567849759 ) ) ;
#28527 = VECTOR ( 'NONE', #29762, 1000.000000000000000 ) ;
#28528 = AXIS2_PLACEMENT_3D ( 'NONE', #4937, #24707, #8111 ) ;
#28529 = CARTESIAN_POINT ( 'NONE',  ( 0.05238710761679706701, 113.0327356262574341, -2.621665085262908423 ) ) ;
#28530 = CARTESIAN_POINT ( 'NONE',  ( -10.54112285291058981, 57.14999999999385949, 5.016499999999999737 ) ) ;
#28531 = CARTESIAN_POINT ( 'NONE',  ( -46.95766867967832070, 25.94401225812155332, -8.271762106911890930E-15 ) ) ;
#28532 = CARTESIAN_POINT ( 'NONE',  ( 1.707630795344756480, -15.17184983623502603, 5.724163072428519072 ) ) ;
#28533 = CARTESIAN_POINT ( 'NONE',  ( -46.20552558087364758, 24.41938074005533466, 2.020549794458497139 ) ) ;
#28534 = DIRECTION ( 'NONE',  ( -0.000000000000000000, -0.000000000000000000, -1.000000000000000000 ) ) ;
#28535 = CARTESIAN_POINT ( 'NONE',  ( -4.639261538484346303, 118.0227684624969413, 0.6550054986553982550 ) ) ;
#28536 = ORIENTED_EDGE ( 'NONE', *, *, #37840, .T. ) ;
#28537 = CARTESIAN_POINT ( 'NONE',  ( -20.56295647043122798, 79.40745607177142062, 1.269999999999995133 ) ) ;
#28538 = CARTESIAN_POINT ( 'NONE',  ( 5.953013861836208065, 119.1077922858878679, -1.025847558928856929 ) ) ;
#28539 = CARTESIAN_POINT ( 'NONE',  ( -2.588518934356020207, 109.4146836159258669, -3.874296054094246600 ) ) ;
#28540 = CARTESIAN_POINT ( 'NONE',  ( 4.596289261446199426, 117.9776677021676221, 0.9191970225659147342 ) ) ;
#28541 = DIRECTION ( 'NONE',  ( 1.000000000000000000, 6.353134868986659519E-16, 0.000000000000000000 ) ) ;
#28542 = CARTESIAN_POINT ( 'NONE',  ( -0.3786798576917292380, 121.5961256765096152, 0.3764709079149205495 ) ) ;
#28543 = CARTESIAN_POINT ( 'NONE',  ( -2.424025297795170619, -5.104216246930970868, 3.935102955759355758 ) ) ;
#28544 = DIRECTION ( 'NONE',  ( 0.8745520943968243532, -0.4849315768086547296, 6.829619984160642269E-16 ) ) ;
#28545 = CARTESIAN_POINT ( 'NONE',  ( 16.87828382557106721, 17.14499999999999957, -5.016499999999999737 ) ) ;
#28546 = CARTESIAN_POINT ( 'NONE',  ( 6.650203214911467597, 123.1390089711370166, 0.06171709628626046579 ) ) ;
#28547 = CARTESIAN_POINT ( 'NONE',  ( -12.49704818634944381, 126.0212559692275249, -1.705261654849118846 ) ) ;
#28548 = CARTESIAN_POINT ( 'NONE',  ( -4.792324638262678960, 56.51998046905272588, 4.972049999962470324 ) ) ;
#28549 = CARTESIAN_POINT ( 'NONE',  ( -3.044072069279135651, 34.44269722464345307, 3.574075509920750626 ) ) ;
#28550 = CARTESIAN_POINT ( 'NONE',  ( -2.432812730531299650, 115.7029433065083879, 1.605937827969098342 ) ) ;
#28551 = CARTESIAN_POINT ( 'NONE',  ( -4.492784857928645792, 12.16275517495587977, -1.104450737933446725 ) ) ;
#28553 = ORIENTED_EDGE ( 'NONE', *, *, #20593, .F. ) ;
#28552 = CARTESIAN_POINT ( 'NONE',  ( 15.27623507474945086, 120.8527393138689376, 0.8201955439070727216 ) ) ;
#28554 = CARTESIAN_POINT ( 'NONE',  ( 1.274087442039063101, 104.6144662015545492, -5.191363564694317034 ) ) ;
#28555 = CARTESIAN_POINT ( 'NONE',  ( 3.235674727752381852, -14.79813088844142399, -0.3705354414145333730 ) ) ;
#28556 = CARTESIAN_POINT ( 'NONE',  ( -11.87140890173658647, 122.0047285378078357, 1.287708742280476715 ) ) ;
#28557 = CARTESIAN_POINT ( 'NONE',  ( -0.8351715869602673870, 27.76506109569598024, 0.5290732382595327854 ) ) ;
#28558 = CARTESIAN_POINT ( 'NONE',  ( -0.6518678778066554491, 5.040965284779599820, 0.7259998264446282379 ) ) ;
#28559 = VERTEX_POINT ( 'NONE', #29053 ) ;
#28560 = AXIS2_PLACEMENT_3D ( 'NONE', #35813, #3440, #38793 ) ;
#28561 = ORIENTED_EDGE ( 'NONE', *, *, #28983, .T. ) ;
#28562 = DIRECTION ( 'NONE',  ( 0.8745520943968221328, -0.4849315768086585043, -5.226292508699494473E-15 ) ) ;
#28563 = CARTESIAN_POINT ( 'NONE',  ( 6.983090746392633719, 124.7321584522365896, 0.1405484879196984560 ) ) ;
#28564 = CARTESIAN_POINT ( 'NONE',  ( -10.01767202841750581, 124.1433363813624311, 0.6017494237236775678 ) ) ;
#28565 = DIRECTION ( 'NONE',  ( 0.9998501190848636533, 0.01731298258487584674, -2.441448296158442805E-15 ) ) ;
#28566 = AXIS2_PLACEMENT_3D ( 'NONE', #21823, #18009, #31432 ) ;
#28567 = CARTESIAN_POINT ( 'NONE',  ( 2.131140412894510838, -15.01828590152304344, 5.319755587316977952 ) ) ;
#28568 = CARTESIAN_POINT ( 'NONE',  ( 11.17823620286574382, 123.1247571232444784, -1.162497134544157706 ) ) ;
#28569 = CARTESIAN_POINT ( 'NONE',  ( -17.39176377602798240, 131.6241255656270255, -2.296140998891703422 ) ) ;
#28570 = LINE ( 'NONE', #38379, #5919 ) ;
#28571 = EDGE_CURVE ( 'NONE', #22816, #27091, #17702, .T. ) ;
#28572 = CARTESIAN_POINT ( 'NONE',  ( 8.504347257126880777, 119.0088918578701396, 1.280434527939347866 ) ) ;
#28573 = DIRECTION ( 'NONE',  ( -0.9734199927291317112, -0.2290273297124542085, -2.993963672467862566E-15 ) ) ;
#28574 = CARTESIAN_POINT ( 'NONE',  ( 3.712124141557857637, 121.0264708767875561, -0.07522066808841043617 ) ) ;
#28575 = ORIENTED_EDGE ( 'NONE', *, *, #32552, .T. ) ;
#28576 = CARTESIAN_POINT ( 'NONE',  ( 3.220330141560203696, -14.30903721375789317, 2.546581355196453345 ) ) ;
#28577 = ADVANCED_FACE ( 'NONE', ( #19458 ), #33458, .T. ) ;
#28578 = CARTESIAN_POINT ( 'NONE',  ( 8.936628967501334841, 56.51500000000000057, 4.721553682181185430 ) ) ;
#28579 = CARTESIAN_POINT ( 'NONE',  ( -8.095114962461808616, 74.19100168833409725, -1.523999999999996691 ) ) ;
#28580 = CARTESIAN_POINT ( 'NONE',  ( -58.27365357893031472, 0.4699239364188423362, 1.042275140647600296 ) ) ;
#28581 = CARTESIAN_POINT ( 'NONE',  ( -8.287855504117665362, 18.49606730478969752, 1.603550922811438406 ) ) ;
#28582 = CARTESIAN_POINT ( 'NONE',  ( 3.381852828898099794, 156.3978305292817481, 1.289121224278522160 ) ) ;
#28583 = CARTESIAN_POINT ( 'NONE',  ( -19.33375693323417011, 80.42273151551299293, -1.524000000000003574 ) ) ;
#28584 = CARTESIAN_POINT ( 'NONE',  ( 22.98521553460854605, 150.1595482613961110, 0.3823759483556145589 ) ) ;
#28585 = CARTESIAN_POINT ( 'NONE',  ( -7.304536785993930970, 123.0387167848234355, -0.07720001398428667783 ) ) ;
#28586 = CARTESIAN_POINT ( 'NONE',  ( 3.315635589170360831, -10.27688868798473720, -3.234826238065521053 ) ) ;
#28587 = LINE ( 'NONE', #22166, #6265 ) ;
#28588 = CARTESIAN_POINT ( 'NONE',  ( 2.927854471352651533, -7.645316342317141967, 7.903470162911977681 ) ) ;
#28589 = CARTESIAN_POINT ( 'NONE',  ( -5.490732243613680730, 117.1204472715084677, -0.7545457724575556080 ) ) ;
#28590 = CARTESIAN_POINT ( 'NONE',  ( -0.4207377039451877243, 124.6436471961814050, -0.04080923199211373281 ) ) ;
#28591 = CARTESIAN_POINT ( 'NONE',  ( 6.475684456959278634, -13.49251406434824574, 0.1304084665236045215 ) ) ;
#28592 = LINE ( 'NONE', #41600, #21550 ) ;
#28593 = CARTESIAN_POINT ( 'NONE',  ( 8.369515367582838650, -11.69187915512254783, 0.7729349465547848963 ) ) ;
#28594 = CARTESIAN_POINT ( 'NONE',  ( 0.9717804538599504882, 118.1588881589075442, 0.8936527240592224697 ) ) ;
#28595 = DIRECTION ( 'NONE',  ( 0.000000000000000000, 0.000000000000000000, 1.000000000000000000 ) ) ;
#28596 = CARTESIAN_POINT ( 'NONE',  ( 1.860714312465608478, -15.17550571231866741, 5.451645902226371021 ) ) ;
#28597 = CARTESIAN_POINT ( 'NONE',  ( 0.8223074630896127779, 121.2007779179981384, -0.3881979734473209320 ) ) ;
#28598 = CARTESIAN_POINT ( 'NONE',  ( -10.59335592519058089, 157.9214973357695158, 0.4646299181629828801 ) ) ;
#28599 = ORIENTED_EDGE ( 'NONE', *, *, #8734, .F. ) ;
#28600 = CARTESIAN_POINT ( 'NONE',  ( -7.917360960270783288, 70.00264313970245666, -1.523999999999995802 ) ) ;
#28601 = ORIENTED_EDGE ( 'NONE', *, *, #38000, .T. ) ;
#28602 = DIRECTION ( 'NONE',  ( 4.017660918040594346E-17, -1.000000000000000000, -2.376309959284834438E-19 ) ) ;
#28603 = CARTESIAN_POINT ( 'NONE',  ( 4.813411144541747788, -15.18245576741394842, 4.205718551895911261 ) ) ;
#28604 = CARTESIAN_POINT ( 'NONE',  ( -13.60271346700661255, 122.2126086331852974, 1.213557020469313574 ) ) ;
#28605 = B_SPLINE_CURVE_WITH_KNOTS ( 'NONE', 3,
 ( #22815, #26670, #35852, #18713, #3391, #16141, #2975, #2772, #15938, #3176, #18926, #12344, #34935, #32556, #2567, #25739 ),
 .UNSPECIFIED., .F., .F.,
 ( 4, 2, 2, 2, 2, 2, 2, 4 ),
 ( 0.000000000000000000, 0.2499999999999866773, 0.3749999999999802380, 0.4374999999999798495, 0.4687499999999812372, 0.4999999999999826805, 0.7499999999999913403, 1.000000000000000000 ),
 .UNSPECIFIED. ) ;
#28606 = CIRCLE ( 'NONE', #14392, 0.2540000000000008917 ) ;
#28607 = CARTESIAN_POINT ( 'NONE',  ( 20.93040400792215650, 136.4823663107028722, -1.114867025985508242 ) ) ;
#28608 = CARTESIAN_POINT ( 'NONE',  ( 1.616848224653315569, 9.589005055319924864, -4.350374724214612243 ) ) ;
#28609 = CARTESIAN_POINT ( 'NONE',  ( -57.17105480285722763, 2.836315218834683627, -2.065842682462495805 ) ) ;
#28610 = ORIENTED_EDGE ( 'NONE', *, *, #33419, .T. ) ;
#28611 = CARTESIAN_POINT ( 'NONE',  ( -0.05238710762259597004, 113.0327356262574341, 2.621665085262795625 ) ) ;
#28612 = CARTESIAN_POINT ( 'NONE',  ( -37.29905550412968296, 27.11271634945815023, -1.270000000000003793 ) ) ;
#28613 = CARTESIAN_POINT ( 'NONE',  ( -10.54966536967472024, 123.3532649940754027, 0.9932924318631480842 ) ) ;
#28614 = FACE_OUTER_BOUND ( 'NONE', #21504, .T. ) ;
#28615 = CARTESIAN_POINT ( 'NONE',  ( 19.01335237852154947, 147.2511928822236769, -1.726116106780063886 ) ) ;
#28616 = CARTESIAN_POINT ( 'NONE',  ( -6.782271978585102445, 118.5360090424673274, -1.159066879843025255 ) ) ;
#28617 = CARTESIAN_POINT ( 'NONE',  ( -52.76912830878634253, 12.08540908813377612, -4.334427935445254398 ) ) ;
#28618 = CARTESIAN_POINT ( 'NONE',  ( 9.756861847786440833, 124.2227999206177032, -0.4199055954619891340 ) ) ;
#28619 = EDGE_LOOP ( 'NONE', ( #32967, #17675 ) ) ;
#28620 = CARTESIAN_POINT ( 'NONE',  ( -18.00824595900801839, 147.8422069945528108, -2.338981374327669727 ) ) ;
#28621 = CARTESIAN_POINT ( 'NONE',  ( 3.879201355988149746, -15.32975156973215292, 1.565980057466964670 ) ) ;
#28622 = CARTESIAN_POINT ( 'NONE',  ( -4.065972646788793554, 118.2429491485453070, -0.3080848862740693250 ) ) ;
#28623 = LINE ( 'NONE', #23047, #2296 ) ;
#28624 = CARTESIAN_POINT ( 'NONE',  ( -4.907886530739225428, 117.6707254041722308, 0.8184263495228992769 ) ) ;
#28625 = CARTESIAN_POINT ( 'NONE',  ( 17.59644933020960522, 144.4767212251450417, 2.299577266864830438 ) ) ;
#28626 = CARTESIAN_POINT ( 'NONE',  ( -46.87302333143581734, 25.14943835889833323, 1.855287453902036310 ) ) ;
#28627 = AXIS2_PLACEMENT_3D ( 'NONE', #37567, #21356, #34382 ) ;
#28628 = CARTESIAN_POINT ( 'NONE',  ( -3.562413952978887632, 23.18266144714348798, 2.948169924785601470 ) ) ;
#28629 = CARTESIAN_POINT ( 'NONE',  ( 7.590630008421936026, 122.4062900713904440, 0.3515417406328249506 ) ) ;
#28630 = CARTESIAN_POINT ( 'NONE',  ( -49.59816314059867182, 17.91649583374774224, -5.069000701391666475 ) ) ;
#28632 = ORIENTED_EDGE ( 'NONE', *, *, #22054, .T. ) ;
#28631 = CARTESIAN_POINT ( 'NONE',  ( -48.30662019010082986, 17.20352665082216248, -3.142973069415128329 ) ) ;
#28633 = CARTESIAN_POINT ( 'NONE',  ( -0.3905063200769877674, 117.9394516740210008, 1.395597172505927963 ) ) ;
#28634 = AXIS2_PLACEMENT_3D ( 'NONE', #25324, #34302, #11700 ) ;
#28635 = CARTESIAN_POINT ( 'NONE',  ( -58.03414100541874632, 0.4564111095344686175, 0.9708715263941495310 ) ) ;
#28636 = CARTESIAN_POINT ( 'NONE',  ( -53.90086641569129711, 9.437825775582018295, 3.763139710719413777 ) ) ;
#28637 = DIRECTION ( 'NONE',  ( 0.8745520943968250194, -0.4849315768086535083, 5.361993529360574930E-16 ) ) ;
#28638 = B_SPLINE_CURVE_WITH_KNOTS ( 'NONE', 3,
 ( #8150, #25120, #8938, #2566, #21904, #34934, #4769, #5760, #18712, #1572, #12343, #25331, #35341, #38334, #38538, #9152, #5965, #6168, #30516, #1355, #25948, #10400, #6789, #15937, #29582, #39597, #16140, #200, #22945, #19979, #19545, #16570, #12752, #13176, #7010, #16788, #32995, #3175, #26163, #6578 ),
 .UNSPECIFIED., .F., .F.,
 ( 4, 2, 1, 2, 2, 2, 1, 1, 2, 2, 2, 2, 1, 1, 1, 2, 2, 2, 2, 1, 1, 2, 2, 4 ),
 ( 0.000000000000000000, 0.1250000000002643996, 0.1875000000003943790, 0.2187500000004593548, 0.2500000000005243583, 0.3750000000007865375, 0.4375000000009133250, 0.4687500000009737766, 0.4843750000010039192, 0.5000000000010339507, 0.6250000000012972956, 0.6875000000014240831, 0.7187500000014875878, 0.7343750000015164536, 0.7421875000015335511, 0.7460937500015469848, 0.7500000000015603074, 0.8125000000011977086, 0.8437500000010164092, 0.8593750000009239276, 0.8671875000008757439, 0.8710937500008516521, 0.8750000000008275602, 1.000000000000000000 ),
 .UNSPECIFIED. ) ;
#28639 = CARTESIAN_POINT ( 'NONE',  ( -5.664977208693910526, 88.73331249999999670, -5.033228321271210781 ) ) ;
#28640 = CARTESIAN_POINT ( 'NONE',  ( -53.35592009511452716, 14.94916803242400682, 1.377413129700644889 ) ) ;
#28641 = CARTESIAN_POINT ( 'NONE',  ( -0.3042766021093734619, 116.4832816433156069, 0.08781055504204338114 ) ) ;
#28642 = ORIENTED_EDGE ( 'NONE', *, *, #15764, .F. ) ;
#28643 = CARTESIAN_POINT ( 'NONE',  ( -48.75318004186330967, 22.89261100037833785, -1.301163434177661893 ) ) ;
#28644 = CARTESIAN_POINT ( 'NONE',  ( -7.800884090505101121, 122.5201264184580339, -0.4525784575430527590 ) ) ;
#28645 = CARTESIAN_POINT ( 'NONE',  ( 8.094215573201640979, 117.4700539315208800, 0.1617416903150405150 ) ) ;
#28646 = VERTEX_POINT ( 'NONE', #36096 ) ;
#28647 = CARTESIAN_POINT ( 'NONE',  ( 2.049820458554627134, 115.7029491482436612, -1.636007937353470387 ) ) ;
#28648 = CARTESIAN_POINT ( 'NONE',  ( -9.673174862102012384, 124.8500477395539576, -0.3609973675953364602 ) ) ;
#28649 = CARTESIAN_POINT ( 'NONE',  ( 5.820712434538892310, -12.64545009755467575, 1.387492028720230364 ) ) ;
#28650 = CARTESIAN_POINT ( 'NONE',  ( -7.920278096381575317, 118.7344292658239340, 0.9023208588851656664 ) ) ;
#28651 = CARTESIAN_POINT ( 'NONE',  ( 10.39017547737320157, 56.51500000000000767, 4.336808689942017736E-15 ) ) ;
#28652 = CARTESIAN_POINT ( 'NONE',  ( 22.58551839157529173, 137.2245694613254443, 0.7673259740012313701 ) ) ;
#28653 = CARTESIAN_POINT ( 'NONE',  ( 5.958951692567330483, 121.5457842488350764, 0.1932771691850621587 ) ) ;
#28654 = LINE ( 'NONE', #3744, #29841 ) ;
#28655 = CARTESIAN_POINT ( 'NONE',  ( -0.8572797930410298584, 14.11360927180527014, 0.4650159543037101773 ) ) ;
#28656 = CARTESIAN_POINT ( 'NONE',  ( -9.813487807256334960, 117.9943556427423488, -0.2419611575297472283 ) ) ;
#28657 = LINE ( 'NONE', #22245, #10005 ) ;
#28658 = CARTESIAN_POINT ( 'NONE',  ( -17.82828877264048018, 64.92754330167842625, 1.523999999999999355 ) ) ;
#28659 = ORIENTED_EDGE ( 'NONE', *, *, #40635, .T. ) ;
#28660 = CARTESIAN_POINT ( 'NONE',  ( -8.584196973278151788, 118.8304167724923559, 0.8833087002087991468 ) ) ;
#28661 = CARTESIAN_POINT ( 'NONE',  ( -58.36509063484196957, -0.2817187151746531337, -0.08504981361425689723 ) ) ;
#28662 = CARTESIAN_POINT ( 'NONE',  ( 3.973247942572128988, 117.7793252414215317, 0.8392447889045230314 ) ) ;
#28663 = CARTESIAN_POINT ( 'NONE',  ( 19.62644950592608240, 149.4594839399872512, -1.701416438606881965 ) ) ;
#28664 = CARTESIAN_POINT ( 'NONE',  ( 3.644365486686961919, 11.68381519529092216, 7.647779612420950279 ) ) ;
#28665 = CARTESIAN_POINT ( 'NONE',  ( -22.13959287704981449, 149.5167998366165989, -1.884152790553834667 ) ) ;
#28666 = CARTESIAN_POINT ( 'NONE',  ( 4.692231461927983460, 117.8897540888554261, -0.8101663176662557975 ) ) ;
#28667 = CIRCLE ( 'NONE', #16399, 0.5080000000000000071 ) ;
#28668 = ADVANCED_FACE ( 'NONE', ( #36308 ), #16898, .F. ) ;
#28669 = CARTESIAN_POINT ( 'NONE',  ( 0.1524052867846317494, 105.8811906981200934, 5.339394923009169958 ) ) ;
#28670 = CARTESIAN_POINT ( 'NONE',  ( -8.537819074431743260, 123.3353292868209365, -0.08920952957173433617 ) ) ;
#28671 = CARTESIAN_POINT ( 'NONE',  ( -17.69102400252393537, 149.9241642446907292, -2.437100891716216022 ) ) ;
#28672 = CARTESIAN_POINT ( 'NONE',  ( 5.114706464973534317, -15.35711304900182128, 3.188446684335360271 ) ) ;
#28673 = CIRCLE ( 'NONE', #10973, 0.5080000000000002292 ) ;
#28674 = DIRECTION ( 'NONE',  ( -0.1469470846586743706, 0.000000000000000000, 0.9891443546370348727 ) ) ;
#28675 = CARTESIAN_POINT ( 'NONE',  ( -3.313229848479803508, 118.1651004895808370, -0.7746738955758309952 ) ) ;
#28676 = ORIENTED_EDGE ( 'NONE', *, *, #8361, .T. ) ;
#28677 = CARTESIAN_POINT ( 'NONE',  ( 3.311752042447743349, 119.2933411826354728, 0.8767012952321084907 ) ) ;
#28678 = CARTESIAN_POINT ( 'NONE',  ( -5.137966006445155109, 56.84472104120887792, 5.330653870689118001 ) ) ;
#28679 = AXIS2_PLACEMENT_3D ( 'NONE', #17525, #23917, #1365 ) ;
#28680 = CARTESIAN_POINT ( 'NONE',  ( -23.62918761621517660, 82.45577215708875940, 1.269999999999993134 ) ) ;
#28681 = CARTESIAN_POINT ( 'NONE',  ( -5.132724724882987921, 121.7269124416356192, 0.09984968675566534280 ) ) ;
#28682 = CARTESIAN_POINT ( 'NONE',  ( 8.237246883283409815, -6.118032110028554627, 1.824569540066587114 ) ) ;
#28683 = CARTESIAN_POINT ( 'NONE',  ( 1.530927031713785080, 120.6610732671444595, 0.3086461854719845244 ) ) ;
#28684 = CARTESIAN_POINT ( 'NONE',  ( 14.33434017258152338, 120.4308286971427862, -0.3827902340739949283 ) ) ;
#28685 = CARTESIAN_POINT ( 'NONE',  ( 5.706177858045066387, 56.51499999999918344, -5.041924731713509189 ) ) ;
#28686 = CIRCLE ( 'NONE', #34145, 0.2540000000000027236 ) ;
#28687 = CARTESIAN_POINT ( 'NONE',  ( -58.34582891702650187, -0.2413224179734804187, 0.1928638016484154616 ) ) ;
#28688 = TOROIDAL_SURFACE ( 'NONE', #15760, 4.826000000000000512, 0.5080000000000000071 ) ;
#28689 = ADVANCED_FACE ( 'NONE', ( #25854 ), #27304, .T. ) ;
#28690 = CARTESIAN_POINT ( 'NONE',  ( -4.123530728113747656, 118.2429491485453354, 0.1804270098900454256 ) ) ;
#28691 = CARTESIAN_POINT ( 'NONE',  ( -4.713631738767456447, 116.7564862437112794, -0.09418957996065566163 ) ) ;
#28692 = ORIENTED_EDGE ( 'NONE', *, *, #34254, .F. ) ;
#28693 = CARTESIAN_POINT ( 'NONE',  ( 6.461527244427501593, 120.2130761765557452, -0.9247372324219909068 ) ) ;
#28695 = CARTESIAN_POINT ( 'NONE',  ( -17.14499999999999957, 71.11999999999999034, -1.904999999999999583 ) ) ;
#28694 = APPLICATION_CONTEXT ( 'automotive_design' ) ;
#28696 = CARTESIAN_POINT ( 'NONE',  ( -12.37067103324092443, 130.6617397222824479, -0.9131297178954277394 ) ) ;
#28697 = CARTESIAN_POINT ( 'NONE',  ( 6.059261036834405978, 56.51500000000000057, -4.547742611252458822 ) ) ;
#28698 = CARTESIAN_POINT ( 'NONE',  ( 22.66341594453896136, 150.6395781703034231, 0.4783972420343530207 ) ) ;
#28699 = ORIENTED_EDGE ( 'NONE', *, *, #27983, .F. ) ;
#28700 = CARTESIAN_POINT ( 'NONE',  ( -3.609430071560130848, 3.966570591990036032, 2.889066364458971137 ) ) ;
#28701 = CARTESIAN_POINT ( 'NONE',  ( -29.47815206431988599, 60.51098513936971557, 1.269999999999994023 ) ) ;
#28702 = DIRECTION ( 'NONE',  ( 5.188838149069472160E-16, -1.699382548006136559E-16, -1.000000000000000000 ) ) ;
#28703 = CARTESIAN_POINT ( 'NONE',  ( -42.52099730114425569, 21.88661877469040817, 1.711735796960834666 ) ) ;
#28704 = CARTESIAN_POINT ( 'NONE',  ( -15.50061618130080987, 62.14374591690594940, 1.904999999999990035 ) ) ;
#28705 = CARTESIAN_POINT ( 'NONE',  ( -7.005943499892747894, 121.7887304234075003, 0.2845919825715230167 ) ) ;
#28706 = CARTESIAN_POINT ( 'NONE',  ( -3.633452533992190592, 26.69063122243967356, -2.854640957048627747 ) ) ;
#28707 = CARTESIAN_POINT ( 'NONE',  ( 1.008854969157035431, 117.0751458430253393, 0.4193480094219991239 ) ) ;
#28708 = CARTESIAN_POINT ( 'NONE',  ( -5.591535794131392123, 65.03215273817657760, 1.270000000000005569 ) ) ;
#28710 = CARTESIAN_POINT ( 'NONE',  ( 10.59408866556482742, 119.9085704333771787, -1.028430606607102726 ) ) ;
#28709 = CARTESIAN_POINT ( 'NONE',  ( 5.638212235253492466, 56.51499999999996504, 5.060089761408623765 ) ) ;
#28711 = CARTESIAN_POINT ( 'NONE',  ( -11.64488154209797877, 123.4149316504530702, 1.218180013452823562 ) ) ;
#28712 = CARTESIAN_POINT ( 'NONE',  ( 4.233688895176465294, 13.94658232072815807, -1.861163356065342001 ) ) ;
#28713 = CARTESIAN_POINT ( 'NONE',  ( -20.68355264112289049, 132.2482564273973935, -1.400420337322433761 ) ) ;
#28714 = VERTEX_POINT ( 'NONE', #16686 ) ;
#28715 = CARTESIAN_POINT ( 'NONE',  ( -57.43854689232674815, 1.757847328446637825, 1.624773336220233011 ) ) ;
#28716 = CARTESIAN_POINT ( 'NONE',  ( -15.88665273169782921, 145.7686330500600036, 0.2792794258575000965 ) ) ;
#28717 = CARTESIAN_POINT ( 'NONE',  ( 4.992311776856191763, -13.37494578157311054, 3.269494339340476952 ) ) ;
#28718 = DIRECTION ( 'NONE',  ( -0.8745520943968243532, 0.4849315768086547296, -6.829619984160642269E-16 ) ) ;
#28719 = AXIS2_PLACEMENT_3D ( 'NONE', #37759, #21974, #22176 ) ;
#28720 = CARTESIAN_POINT ( 'NONE',  ( -4.616126210598159751, 118.0369330104597623, -0.7916877136874118648 ) ) ;
#28721 = ADVANCED_FACE ( 'NONE', ( #33318 ), #113, .T. ) ;
#28722 = CARTESIAN_POINT ( 'NONE',  ( 15.38068278028558922, 147.8292851303062321, 0.2562860988859089195 ) ) ;
#28723 = ORIENTED_EDGE ( 'NONE', *, *, #14350, .F. ) ;
#28724 = CARTESIAN_POINT ( 'NONE',  ( 12.70548372655388114, 122.4237789811383550, 1.817438969878694577 ) ) ;
#28725 = CARTESIAN_POINT ( 'NONE',  ( 5.106395947886047004, 78.95054594174945350, 1.904999999999988258 ) ) ;
#28726 = DIRECTION ( 'NONE',  ( 0.1728608224830406603, 0.000000000000000000, -0.9849462604886047856 ) ) ;
#28727 = CARTESIAN_POINT ( 'NONE',  ( -7.773589648320968770, 158.6130819278358501, 0.6584978287542905262 ) ) ;
#28728 = CARTESIAN_POINT ( 'NONE',  ( 4.887628697012647905, 117.4785758328482217, -0.9709680806009058918 ) ) ;
#28729 = CIRCLE ( 'NONE', #9707, 9.048750000000000071 ) ;
#28730 = CARTESIAN_POINT ( 'NONE',  ( 14.68764241912298729, 120.3119357913517291, -0.01896423869846134910 ) ) ;
#28731 = EDGE_CURVE ( 'NONE', #37020, #5536, #22639, .T. ) ;
#28732 = CYLINDRICAL_SURFACE ( 'NONE', #36325, 0.5080000000000000071 ) ;
#28733 = CARTESIAN_POINT ( 'NONE',  ( -11.66725022231030628, 55.24499999999999744, 5.016500000000000625 ) ) ;
#28734 = CARTESIAN_POINT ( 'NONE',  ( -46.60530155212503445, 26.17382724835477958, -8.082077239948803202E-15 ) ) ;
#28735 = CARTESIAN_POINT ( 'NONE',  ( -4.962531982528343377, 117.4056870407710989, -1.029597432040127991 ) ) ;
#28736 = CARTESIAN_POINT ( 'NONE',  ( -41.45218294293373162, 22.69057396248467384, 1.547390787314418592 ) ) ;
#28737 = CARTESIAN_POINT ( 'NONE',  ( -17.14499999999999957, 71.11999999999999034, 1.904999999999989146 ) ) ;
#28738 = CARTESIAN_POINT ( 'NONE',  ( -4.519476466213967036, 118.0838058619411441, 0.6171013934025890713 ) ) ;
#28739 = VERTEX_POINT ( 'NONE', #32469 ) ;
#28740 = EDGE_LOOP ( 'NONE', ( #2378, #12719, #27665, #14126, #2448, #12713 ) ) ;
#28741 = CARTESIAN_POINT ( 'NONE',  ( -3.160680854049036093, 118.7629491485454309, -1.175202071525837999 ) ) ;
#28742 = EDGE_CURVE ( 'NONE', #30888, #24697, #22557, .T. ) ;
#28743 = CARTESIAN_POINT ( 'NONE',  ( -3.526808273775506208, 118.7004473170249668, -0.9357397655257763125 ) ) ;
#28744 = CARTESIAN_POINT ( 'NONE',  ( -5.237871118309435303, 118.7524313932052991, -0.6368175916084591881 ) ) ;
#28745 = CARTESIAN_POINT ( 'NONE',  ( 4.811267787481693148, 117.7644185172598554, 1.004593082574424256 ) ) ;
#28746 = CARTESIAN_POINT ( 'NONE',  ( -5.451267667241070720E-14, 85.80437499999999318, 0.000000000000000000 ) ) ;
#28747 = CARTESIAN_POINT ( 'NONE',  ( -13.80305775881212327, 134.3516747369166069, -1.357216474725372546 ) ) ;
#28748 = AXIS2_PLACEMENT_3D ( 'NONE', #39294, #10728, #30740 ) ;
#28749 = EDGE_CURVE ( 'NONE', #23948, #22322, #29357, .T. ) ;
#28750 = FACE_OUTER_BOUND ( 'NONE', #13421, .T. ) ;
#28751 = CARTESIAN_POINT ( 'NONE',  ( -5.965356522962928842, 57.14999999999997016, -5.016499999999999737 ) ) ;
#28752 = CARTESIAN_POINT ( 'NONE',  ( 0.3637657132512605029, 105.8833743670705445, -5.328194401858565854 ) ) ;
#28753 = CARTESIAN_POINT ( 'NONE',  ( -11.01900745353701083, 123.5714170083676748, -1.527874194239944305 ) ) ;
#28754 = CARTESIAN_POINT ( 'NONE',  ( 20.51686376604209983, 129.1072961674477710, 0.4099757654675942331 ) ) ;
#28755 = CARTESIAN_POINT ( 'NONE',  ( -0.02537255736359531402, 39.20946620154573026, 1.269746523260778304 ) ) ;
#28756 = CARTESIAN_POINT ( 'NONE',  ( -3.475550415873033039, 115.7029637594141604, 1.501259963919143070 ) ) ;
#28757 = CARTESIAN_POINT ( 'NONE',  ( 3.345514242732226418, 6.565394131763864216, 3.211428121085859733 ) ) ;
#28759 = ORIENTED_EDGE ( 'NONE', *, *, #4350, .F. ) ;
#28758 = CARTESIAN_POINT ( 'NONE',  ( 14.97360968503852341, 156.1447123740162226, 0.9344295344441085893 ) ) ;
#28760 = CARTESIAN_POINT ( 'NONE',  ( -0.1151806861323783349, 105.1224247242857075, -5.344135852030379219 ) ) ;
#28761 = CARTESIAN_POINT ( 'NONE',  ( 3.794293369880153310, -15.39696243832143452, 2.404174946430260196 ) ) ;
#28762 = CARTESIAN_POINT ( 'NONE',  ( -15.81176147471982674, 128.5598958631237565, 1.562949982248214464 ) ) ;
#28763 = CARTESIAN_POINT ( 'NONE',  ( 0.9467939684353117169, 21.72092434492431323, 0.2316696090552467224 ) ) ;
#28764 = AXIS2_PLACEMENT_3D ( 'NONE', #38494, #32736, #41694 ) ;
#28765 = CARTESIAN_POINT ( 'NONE',  ( 0.2560056206704328097, 6.564126901726701213, 0.9442708342526761056 ) ) ;
#28766 = ORIENTED_EDGE ( 'NONE', *, *, #10562, .T. ) ;
#28767 = VECTOR ( 'NONE', #1874, 1000.000000000000000 ) ;
#28768 = ORIENTED_EDGE ( 'NONE', *, *, #32686, .F. ) ;
#28769 = CARTESIAN_POINT ( 'NONE',  ( -41.05189575270517821, 23.09451173561983950, 1.523999999999993582 ) ) ;
#28770 = ADVANCED_FACE ( 'NONE', ( #13291 ), #32772, .T. ) ;
#28771 = CARTESIAN_POINT ( 'NONE',  ( 5.810938089476312740, 124.3836500214474654, 0.1311214433933295398 ) ) ;
#28772 = SHAPE_DEFINITION_REPRESENTATION ( #6879, #11484 ) ;
#28773 = CARTESIAN_POINT ( 'NONE',  ( -6.511415066510978455, 121.4051597255373025, 0.4520850151541543904 ) ) ;
#28774 = CARTESIAN_POINT ( 'NONE',  ( -8.935197197525255319, 123.9063447689825779, -0.1785465045940570761 ) ) ;
#28775 = CARTESIAN_POINT ( 'NONE',  ( 2.973740295910565212, -14.46567735677360744, 4.831635400698222504 ) ) ;
#28776 = CARTESIAN_POINT ( 'NONE',  ( 0.02874415600660452930, 157.0795416643300939, -1.438475106415293858 ) ) ;
#28777 = CARTESIAN_POINT ( 'NONE',  ( -12.01076045986772023, 121.8643784861682065, -1.757760809232695953 ) ) ;
#28778 = CARTESIAN_POINT ( 'NONE',  ( -23.69188486464780752, 78.08202335040543574, 1.269999999999993801 ) ) ;
#28779 = CARTESIAN_POINT ( 'NONE',  ( 8.016682068476109535, 121.3927152696642366, 1.222808765174667522 ) ) ;
#28780 = CARTESIAN_POINT ( 'NONE',  ( 4.074910602682932925, 118.2429491485453354, -0.1454311599470142491 ) ) ;
#28781 = CARTESIAN_POINT ( 'NONE',  ( 15.30649785019662801, 148.0176312819745874, -0.02196777213629026379 ) ) ;
#28782 = ORIENTED_EDGE ( 'NONE', *, *, #8720, .T. ) ;
#28783 = CARTESIAN_POINT ( 'NONE',  ( -11.24191166894635430, 82.34025985790688651, 1.269999999999999352 ) ) ;
#28784 = CIRCLE ( 'NONE', #20608, 0.2540000000000057767 ) ;
#28785 = CYLINDRICAL_SURFACE ( 'NONE', #24520, 0.5080000000000007843 ) ;
#28786 = AXIS2_PLACEMENT_3D ( 'NONE', #29863, #36054, #39244 ) ;
#28787 = EDGE_CURVE ( 'NONE', #37991, #26194, #32099, .T. ) ;
#28788 = CARTESIAN_POINT ( 'NONE',  ( -9.960492004070040650, 64.81807050032566053, -1.523999999999996025 ) ) ;
#28789 = CARTESIAN_POINT ( 'NONE',  ( 4.581850893073086795, -15.30275035579069254, -0.5110622633019785699 ) ) ;
#28790 = CARTESIAN_POINT ( 'NONE',  ( 14.05504870572961629, 134.4521314832425389, 1.517394082013088674 ) ) ;
#28791 = DIRECTION ( 'NONE',  ( -0.01997839162482761832, -1.040247600000950455E-18, 0.9998004120163610509 ) ) ;
#28792 = CARTESIAN_POINT ( 'NONE',  ( 23.36108720469560041, 148.8745345081378559, 0.4410421544236570179 ) ) ;
#28793 = CARTESIAN_POINT ( 'NONE',  ( -5.578601203221947635, 117.9513286348681476, 0.5234822864975617884 ) ) ;
#28794 = CIRCLE ( 'NONE', #22654, 0.6350000000000001199 ) ;
#28795 = CARTESIAN_POINT ( 'NONE',  ( -5.177913976931285411, 57.14999999999999858, -5.372100000000001430 ) ) ;
#28796 = CARTESIAN_POINT ( 'NONE',  ( 10.18105065676961729, 125.9743313966586129, 0.2034416216762106322 ) ) ;
#28797 = CARTESIAN_POINT ( 'NONE',  ( 21.10297322700568756, 148.1333099715771766, 2.360403108977008557 ) ) ;
#28798 = CARTESIAN_POINT ( 'NONE',  ( 2.403447530314441583, 28.79142288871172539, -8.109455235164826803 ) ) ;
#28799 = CARTESIAN_POINT ( 'NONE',  ( 8.749828080525578144, 117.9752082124837074, -0.3959020732588000580 ) ) ;
#28800 = CARTESIAN_POINT ( 'NONE',  ( 0.1041500444722623514, 106.1822392402443143, -5.212094112990278028 ) ) ;
#28801 = DIRECTION ( 'NONE',  ( -0.8745520943968240202, 0.4849315768086551737, -5.361993529360572958E-16 ) ) ;
#28802 = CARTESIAN_POINT ( 'NONE',  ( -0.2386826763840395327, 104.6144662015434221, 5.340208467583181573 ) ) ;
#28803 = CARTESIAN_POINT ( 'NONE',  ( 3.740357457071568081, -9.854013591530623728, -7.545904704300070875 ) ) ;
#28804 = EDGE_CURVE ( 'NONE', #19390, #18488, #7332, .T. ) ;
#28805 = CARTESIAN_POINT ( 'NONE',  ( -11.58677707360137532, 55.24499999999999034, -4.474811398758259173 ) ) ;
#28806 = DIRECTION ( 'NONE',  ( 4.017660918040594346E-17, -1.000000000000000000, -2.376309959284834438E-19 ) ) ;
#28807 = CARTESIAN_POINT ( 'NONE',  ( 3.177488185987922709, -14.13217061847354472, 2.003775387181677026 ) ) ;
#28808 = CARTESIAN_POINT ( 'NONE',  ( 0.3869134157276650776, 116.4813942609866899, -1.514588684444738709 ) ) ;
#28809 = CARTESIAN_POINT ( 'NONE',  ( -0.9702981664979649645, 116.7682604261274264, 0.2585377725347693945 ) ) ;
#28810 = ORIENTED_EDGE ( 'NONE', *, *, #6119, .F. ) ;
#28811 = CARTESIAN_POINT ( 'NONE',  ( 5.664977208693820820, 65.30181249999998272, 5.033228321271210781 ) ) ;
#28812 = ORIENTED_EDGE ( 'NONE', *, *, #14420, .F. ) ;
#28813 = CARTESIAN_POINT ( 'NONE',  ( -43.16005656664464851, 21.89413631511616032, -2.197846903552944653 ) ) ;
#28814 = AXIS2_PLACEMENT_3D ( 'NONE', #41450, #14804, #41022 ) ;
#28815 = CARTESIAN_POINT ( 'NONE',  ( 5.396943489592968213, -15.24705710738187570, 2.503009974473451749 ) ) ;
#28816 = CARTESIAN_POINT ( 'NONE',  ( -6.797121414357407687, 118.7881172115286148, 0.9472104157431981974 ) ) ;
#28817 = CARTESIAN_POINT ( 'NONE',  ( 3.003295232750816002, 159.1263692740743068, -1.093010787580665610 ) ) ;
#28818 = CARTESIAN_POINT ( 'NONE',  ( -2.406711483539481389, 4.503775517365914638, 3.979180414515509412 ) ) ;
#28819 = CARTESIAN_POINT ( 'NONE',  ( -58.13819340830944071, 0.7633750567142213450, -1.210128363568031995 ) ) ;
#28820 = CIRCLE ( 'NONE', #4339, 0.2540000000000015024 ) ;
#28821 = ORIENTED_EDGE ( 'NONE', *, *, #25333, .F. ) ;
#28822 = CARTESIAN_POINT ( 'NONE',  ( -58.44960050528086271, -0.4277149010484683211, -0.3217025345699726646 ) ) ;
#28823 = CARTESIAN_POINT ( 'NONE',  ( -3.841520934845505941, 71.62889921741444255, 1.270000000000005125 ) ) ;
#28824 = CARTESIAN_POINT ( 'NONE',  ( -5.671251014262852941, 28.19322323727007884, 0.3848925825754440644 ) ) ;
#28825 = CARTESIAN_POINT ( 'NONE',  ( -17.48603724727291819, 147.5992144370567871, 1.461888717290058315 ) ) ;
#28826 = LINE ( 'NONE', #35026, #2099 ) ;
#28827 = CARTESIAN_POINT ( 'NONE',  ( 11.94919878421452708, 122.6721150436042223, -1.294096368778067996 ) ) ;
#28828 = CARTESIAN_POINT ( 'NONE',  ( -20.51891680819880648, 149.8464234248869786, -2.337676305755668871 ) ) ;
#28829 = CARTESIAN_POINT ( 'NONE',  ( -58.03414100541874632, 0.4564111095344686175, -0.9708715263941700702 ) ) ;
#28830 = CIRCLE ( 'NONE', #13191, 0.3810000000000015041 ) ;
#28831 = ORIENTED_EDGE ( 'NONE', *, *, #9209, .T. ) ;
#28832 = CARTESIAN_POINT ( 'NONE',  ( 8.914966108837827363, 123.2307073318660855, -0.3922733289213620744 ) ) ;
#28833 = EDGE_LOOP ( 'NONE', ( #35364, #6479, #41754, #13271 ) ) ;
#28834 = CARTESIAN_POINT ( 'NONE',  ( -5.835695000730485305, 120.1673030736515955, -1.074193948046630487 ) ) ;
#28835 = CARTESIAN_POINT ( 'NONE',  ( 3.866492242221801767, -15.24987600803320831, 0.6064936129020901401 ) ) ;
#28836 = CARTESIAN_POINT ( 'NONE',  ( -4.160788897500995454, 118.2392053592570420, -0.3833967187953443712 ) ) ;
#28837 = CARTESIAN_POINT ( 'NONE',  ( -58.37116772670351850, -0.2940390518722524327, -2.603646672650065119E-13 ) ) ;
#28838 = CARTESIAN_POINT ( 'NONE',  ( -4.936883229164080511, 117.6536490159478774, 0.7443082606323431216 ) ) ;
#28839 = CARTESIAN_POINT ( 'NONE',  ( 17.90704175211108407, 146.6345634702618952, 2.297399834898016913 ) ) ;
#28840 = CARTESIAN_POINT ( 'NONE',  ( -47.00737061383054538, 25.44871393995434872, 1.744193148939842564 ) ) ;
#28841 = AXIS2_PLACEMENT_3D ( 'NONE', #35694, #32066, #35909 ) ;
#28842 = CARTESIAN_POINT ( 'NONE',  ( 2.739727753987758252, 28.35525327666260864, -3.728201022356329553 ) ) ;
#28843 = CARTESIAN_POINT ( 'NONE',  ( 15.82044549406348288, 146.2622375132148989, 0.6472507553222683896 ) ) ;
#28844 = DIRECTION ( 'NONE',  ( 0.9998004120163608288, 0.000000000000000000, 0.01997839162482762526 ) ) ;
#28846 = ORIENTED_EDGE ( 'NONE', *, *, #27268, .F. ) ;
#28845 = CARTESIAN_POINT ( 'NONE',  ( -47.64484625134591766, 19.26749830283604936, -4.730721332201286877 ) ) ;
#28847 = DIRECTION ( 'NONE',  ( -0.8745520943968245753, 0.4849315768086539524, -5.691349986800526185E-16 ) ) ;
#28848 = DIRECTION ( 'NONE',  ( -0.9998004120163609398, 0.000000000000000000, -0.01997839162482749689 ) ) ;
#28849 = CARTESIAN_POINT ( 'NONE',  ( -49.57073425708396286, 16.97194942007707752, 5.013496192390408446 ) ) ;
#28850 = CARTESIAN_POINT ( 'NONE',  ( -6.555005513994535572E-14, 79.34146620154574236, -6.390659674827382268E-18 ) ) ;
#28851 = CARTESIAN_POINT ( 'NONE',  ( -6.059261036834474368, 65.30181249999998272, -5.016499999999999737 ) ) ;
#28852 = CARTESIAN_POINT ( 'NONE',  ( -55.80532936045742787, 9.325833942462050885, 0.2199084463661053201 ) ) ;
#28853 = CARTESIAN_POINT ( 'NONE',  ( -13.38634958471969405, 156.9592627042916604, 0.007429229355843914098 ) ) ;
#28854 = VERTEX_POINT ( 'NONE', #324 ) ;
#28855 = CARTESIAN_POINT ( 'NONE',  ( -52.96141808003752516, 14.46028723511719960, -2.643142726894160521 ) ) ;
#28856 = CARTESIAN_POINT ( 'NONE',  ( -5.970780167368420877, 121.4216606831084988, -0.2372359777413814430 ) ) ;
#28857 = DIRECTION ( 'NONE',  ( -0.8745520943968235761, 0.4849315768086558398, -5.691349986800547879E-16 ) ) ;
#28858 = ORIENTED_EDGE ( 'NONE', *, *, #30810, .F. ) ;
#28859 = CARTESIAN_POINT ( 'NONE',  ( 0.7578165627612494237, 115.7030197700005090, -1.728705102643625535 ) ) ;
#28861 = CIRCLE ( 'NONE', #38395, 0.2539999999999998925 ) ;
#28860 = CARTESIAN_POINT ( 'NONE',  ( -12.96905644698489013, 133.8854804328748571, -0.4775921230882990698 ) ) ;
#28862 = CARTESIAN_POINT ( 'NONE',  ( 6.231544205925810154, -13.28212530995504004, 1.212557631246017564 ) ) ;
#28863 = CARTESIAN_POINT ( 'NONE',  ( -20.87437586479492779, 150.1670661137953289, 1.386469220648549383 ) ) ;
#28864 = DIRECTION ( 'NONE',  ( -0.8745520943968235761, 0.4849315768086558398, -5.691349986800547879E-16 ) ) ;
#28865 = CARTESIAN_POINT ( 'NONE',  ( 5.727173706516636820, 159.1225378944267845, 0.2665985390141683009 ) ) ;
#28866 = CARTESIAN_POINT ( 'NONE',  ( 8.943424089997177973, 124.0488429294995711, 0.3121749486774180182 ) ) ;
#28867 = CARTESIAN_POINT ( 'NONE',  ( 4.808056391921498474, 118.5266822147775940, -0.8104460292946976674 ) ) ;
#28868 = CARTESIAN_POINT ( 'NONE',  ( -0.8667032531718782407, 4.505117207799016477, 0.4606053492026337959 ) ) ;
#28869 = CARTESIAN_POINT ( 'NONE',  ( -17.22116264704572686, 122.7389118244895769, -0.4537515290936992574 ) ) ;
#28870 = CARTESIAN_POINT ( 'NONE',  ( 5.586884702347363785, 100.6774662015457409, 0.1116392523995368286 ) ) ;
#28871 = DIRECTION ( 'NONE',  ( -0.8745520943968235761, 0.4849315768086558953, -5.361993529360570985E-16 ) ) ;
#28872 = ORIENTED_EDGE ( 'NONE', *, *, #21522, .T. ) ;
#28873 = CARTESIAN_POINT ( 'NONE',  ( -5.574303926328670222, 117.3559425346390839, 0.6178643877552448815 ) ) ;
#28874 = ORIENTED_EDGE ( 'NONE', *, *, #19947, .T. ) ;
#28875 = CARTESIAN_POINT ( 'NONE',  ( 2.958531772299235918, 50.13146620154573441, 1.329372033065076453 ) ) ;
#28876 = CARTESIAN_POINT ( 'NONE',  ( 17.95761459997873999, 128.5942011134444272, 1.926528613670785095 ) ) ;
#28877 = CARTESIAN_POINT ( 'NONE',  ( 18.88973499030869618, 150.3568762430427910, -1.706130117709411476 ) ) ;
#28878 = AXIS2_PLACEMENT_3D ( 'NONE', #8737, #21697, #5553 ) ;
#28879 = CARTESIAN_POINT ( 'NONE',  ( 5.986726992493722754, 14.59627609256335923, -5.926391003037220884 ) ) ;
#28880 = CARTESIAN_POINT ( 'NONE',  ( -22.34269864632769043, 148.4347612714453248, -1.893969414928640571 ) ) ;
#28881 = CARTESIAN_POINT ( 'NONE',  ( 4.752741535181148613, 117.9428596717473283, -0.6274105461657691896 ) ) ;
#28882 = FACE_OUTER_BOUND ( 'NONE', #19126, .T. ) ;
#28883 = CARTESIAN_POINT ( 'NONE',  ( -15.64855408859538244, 147.2205073051419504, -0.1844942485914528030 ) ) ;
#28884 = CARTESIAN_POINT ( 'NONE',  ( -16.04699077284492148, 131.4332636412663931, -2.269269673164716838 ) ) ;
#28885 = CARTESIAN_POINT ( 'NONE',  ( 2.040901337265842663, -15.69771917786945359, 5.688463219523050896 ) ) ;
#28886 = DIRECTION ( 'NONE',  ( -0.8745520943968361216, 0.4849315768086333023, -6.829619984160648185E-16 ) ) ;
#28887 = CARTESIAN_POINT ( 'NONE',  ( -46.67659519887700981, 22.71018310752411651, -3.598098858967615055 ) ) ;
#28888 = ORIENTED_EDGE ( 'NONE', *, *, #39258, .T. ) ;
#28889 = CARTESIAN_POINT ( 'NONE',  ( 18.01629081398013099, 149.0664087073519681, 2.421686302305671390 ) ) ;
#28890 = CARTESIAN_POINT ( 'NONE',  ( 14.39766717389552220, 12.96416000000000146, 1.904999999999990923 ) ) ;
#28891 = CARTESIAN_POINT ( 'NONE',  ( -2.922973558833878549, 114.3344743418335128, 2.013556875909916943 ) ) ;
#28892 = CARTESIAN_POINT ( 'NONE',  ( 4.580344459542567748, 28.35322510196829171, -7.077419036913218164 ) ) ;
#28893 = CARTESIAN_POINT ( 'NONE',  ( 4.473455768776775976, 120.9326014760084007, 0.4576173489010091910 ) ) ;
#28894 = CARTESIAN_POINT ( 'NONE',  ( 0.005915287708639699847, 116.9295063353193882, -0.2960251855814708954 ) ) ;
#28895 = CARTESIAN_POINT ( 'NONE',  ( 5.237379388564935567, 115.7029491485453150, 1.024072862575109655 ) ) ;
#28896 = DIRECTION ( 'NONE',  ( -0.8745520943968225769, 0.4849315768086578382, -5.691349986800571545E-16 ) ) ;
#28897 = CARTESIAN_POINT ( 'NONE',  ( -2.744962145539713294, 116.5337465564440578, -0.01469834071105278160 ) ) ;
#28898 = VERTEX_POINT ( 'NONE', #26276 ) ;
#28899 = CARTESIAN_POINT ( 'NONE',  ( 6.426253893156781416, 120.1342996155803888, -0.9373394870581658322 ) ) ;
#28900 = CARTESIAN_POINT ( 'NONE',  ( 3.641052418405362090, -15.28906014138697422, 5.355520729203003150 ) ) ;
#28901 = CARTESIAN_POINT ( 'NONE',  ( -15.91553746749639942, 146.9815093338748966, -1.044385907527698443 ) ) ;
#28902 = CARTESIAN_POINT ( 'NONE',  ( -6.068413118431933206, 121.4395679076997823, -0.1212613395058407956 ) ) ;
#28903 = CARTESIAN_POINT ( 'NONE',  ( 22.66375647020915807, 150.6386093215955100, 0.4528757910175261192 ) ) ;
#28904 = EDGE_LOOP ( 'NONE', ( #12989, #10215, #24939, #33338 ) ) ;
#28905 = CARTESIAN_POINT ( 'NONE',  ( 4.364008504204949013, 7.202613900313124873, 1.580794030135405537 ) ) ;
#28906 = FACE_OUTER_BOUND ( 'NONE', #40110, .T. ) ;
#28907 = CARTESIAN_POINT ( 'NONE',  ( -22.46755768833301303, 150.8526571111528654, -0.4489552724284875951 ) ) ;
#28908 = CARTESIAN_POINT ( 'NONE',  ( -8.519412162535125788, 69.40335734044577976, -1.523999999999996025 ) ) ;
#28909 = CARTESIAN_POINT ( 'NONE',  ( -14.39766717389552220, 60.02151067229126369, 1.905000000000008686 ) ) ;
#28910 = CARTESIAN_POINT ( 'NONE',  ( 6.972867087885918025, 121.1626460931736347, 0.9873634393825863054 ) ) ;
#28911 = CARTESIAN_POINT ( 'NONE',  ( 1.748379858460863856, 5.525481214791113871, -4.283037568778763848 ) ) ;
#28912 = CARTESIAN_POINT ( 'NONE',  ( 2.920589480036142049, 117.1197906563906344, 0.5561477985301584992 ) ) ;
#28913 = FACE_OUTER_BOUND ( 'NONE', #15174, .T. ) ;
#28915 = CARTESIAN_POINT ( 'NONE',  ( 13.59286959522813909, 121.6867650304669013, -1.114243377227002396 ) ) ;
#28914 = CARTESIAN_POINT ( 'NONE',  ( 1.569777447552894500, 106.5494078766684822, 5.038031550283630366 ) ) ;
#28916 = CARTESIAN_POINT ( 'NONE',  ( 1.391598188199559161, 15.24595356501894017, -4.406646451508545503 ) ) ;
#28917 = CARTESIAN_POINT ( 'NONE',  ( -5.829268545577303229, 117.2350771734024164, -0.5950018394081720841 ) ) ;
#28918 = ORIENTED_EDGE ( 'NONE', *, *, #23848, .F. ) ;
#28919 = CARTESIAN_POINT ( 'NONE',  ( -15.66930740726056293, 147.5723176251010784, 0.2779681209298468514 ) ) ;
#28920 = CARTESIAN_POINT ( 'NONE',  ( 4.815776949948430641, -14.65450223259012752, 4.385166865640996114 ) ) ;
#28921 = CARTESIAN_POINT ( 'NONE',  ( -26.51793118801306548, 72.98537704160715123, 1.269999999999993134 ) ) ;
#28922 = CARTESIAN_POINT ( 'NONE',  ( -4.608275094037495911, 117.9807440340913303, -0.9110670956906681273 ) ) ;
#28923 = CARTESIAN_POINT ( 'NONE',  ( 11.82813386268891165, 130.3161362890850512, 0.2363542639706543158 ) ) ;
#28925 = ORIENTED_EDGE ( 'NONE', *, *, #19182, .F. ) ;
#28924 = AXIS2_PLACEMENT_3D ( 'NONE', #435, #32577, #38559 ) ;
#28926 = CARTESIAN_POINT ( 'NONE',  ( 1.054772537320672887, 158.2739225783580537, 1.630455200628576851 ) ) ;
#28927 = FACE_OUTER_BOUND ( 'NONE', #2905, .T. ) ;
#28928 = CARTESIAN_POINT ( 'NONE',  ( -21.97872426622829067, 150.5960492154097778, 0.7309654607748480304 ) ) ;
#28929 = B_SPLINE_CURVE_WITH_KNOTS ( 'NONE', 3,
 ( #541, #36728, #39085, #29492, #333, #29910 ),
 .UNSPECIFIED., .F., .F.,
 ( 4, 2, 4 ),
 ( 0.000000000000000000, 0.4999999999999998890, 0.5010344700412979746 ),
 .UNSPECIFIED. ) ;
#28930 = CARTESIAN_POINT ( 'NONE',  ( 4.987388792096843382, 117.4712839033013694, -0.8196840828292851766 ) ) ;
#28931 = CARTESIAN_POINT ( 'NONE',  ( 22.86474403352223561, 150.1122123445777277, -0.1353427831800515235 ) ) ;
#28932 = CARTESIAN_POINT ( 'NONE',  ( -5.217562798876929975, 115.7029491485453576, -1.133914326198557587 ) ) ;
#28933 = DIRECTION ( 'NONE',  ( 5.206863593109713661E-17, -1.000000000000000000, 1.077750396879097183E-30 ) ) ;
#28934 = CARTESIAN_POINT ( 'NONE',  ( -46.60530155212504155, 26.17382724835477248, 0.2116666666666584817 ) ) ;
#28935 = CARTESIAN_POINT ( 'NONE',  ( 1.913489507893775698, -15.20816560145711627, 5.407669831558338913 ) ) ;
#28936 = CARTESIAN_POINT ( 'NONE',  ( -47.61549956331938915, 19.66157307908738261, 5.197827534590556908 ) ) ;
#28937 = CARTESIAN_POINT ( 'NONE',  ( -58.65723136083905587, -0.3152049157291291204, 0.3253893282242821261 ) ) ;
#28938 = ADVANCED_FACE ( 'NONE', ( #20290 ), #19169, .T. ) ;
#28939 = CARTESIAN_POINT ( 'NONE',  ( -4.689025485151536721, 118.0064216981434129, 0.5872937155463054948 ) ) ;
#28940 = B_SPLINE_SURFACE_WITH_KNOTS ( 'NONE', 3, 3, ( 
 ( #10616, #33424, #23598, #14017, #30213 ),
 ( #30003, #24020, #16797, #20397, #7647 ),
 ( #36619, #7019, #26598, #33216, #13815 ),
 ( #37038, #23163, #36413, #33843, #4042 ),
 ( #4253, #14221, #36829, #7438, #17216 ),
 ( #20605, #1266, #1053, #36198, #13607 ),
 ( #637, #19987, #39605, #7856, #13395 ),
 ( #33637, #10408, #20191, #33004, #27024 ),
 ( #11038, #40032, #10825, #39822, #17003 ),
 ( #842, #23808, #4464, #3833, #17421 ),
 ( #26814, #27230, #40244, #20817, #17627 ),
 ( #425, #26383, #24645, #5298, #38079 ),
 ( #34672, #5718, #24433, #21436, #40857 ),
 ( #8894, #27639, #11660, #14429, #18246 ),
 ( #21862, #24228, #37656, #18461, #28275 ),
 ( #14637, #8480, #18044, #11243, #34465 ),
 ( #5502, #5091, #40652, #31045, #24866 ),
 ( #41280, #27437, #1683, #41066, #34887 ),
 ( #37862, #8686, #17837, #31251, #34052 ),
 ( #34262, #21648, #30629, #1884, #31466 ),
 ( #11445, #2309, #25074, #27850, #14846 ),
 ( #40452, #37438, #1472, #37238, #8260 ),
 ( #28057, #8056, #15269, #11877, #2093 ),
 ( #15057, #21029, #21233, #12086, #4882 ),
 ( #30835, #15486, #115, #10517, #9881 ),
 ( #10094, #33112, #13509, #29485, #36100 ),
 ( #39502, #20089, #23067, #29056, #32471 ),
 ( #6486, #38865, #3301, #26711, #31681 ),
 ( #26498, #19462, #16265, #42075, #6914 ),
 ( #29904, #3731, #13293, #16480, #29268 ),
 ( #13079, #19884, #32899, #12869, #23276 ),
 ( #22852, #19670, #22641, #25857, #35891 ),
 ( #326, #26069, #32684, #39079, #16902 ),
 ( #3519, #9676, #39717, #10308, #3942 ),
 ( #36312, #7132, #6701, #35677, #26279 ),
 ( #39288, #16688, #742, #29694, #2523 ),
 ( #535, #13717, #23488, #36514, #18674 ),
 ( #11354, #23920, #4365, #36936, #1583 ),
 ( #17946, #4149, #20505, #17734, #14750 ) ),
 .UNSPECIFIED., .F., .F., .F.,
 ( 4, 1, 1, 1, 1, 1, 1, 1, 1, 1, 1, 2, 1, 1, 1, 1, 1, 1, 1, 1, 1, 1, 1, 1, 1, 1, 1, 1, 1, 1, 1, 1, 1, 1, 1, 4 ),
 ( 4, 1, 4 ),
 ( 0.000000000000000000, 0.01653533301974152367, 0.03307066603948304734, 0.04960599905922460223, 0.06614133207896609468, 0.08267666509870763569, 0.09921199811844919059, 0.1322826641579321894, 0.1653533301974152714, 0.1984239962368983812, 0.2314946622763813522, 0.2645653283158643787, 0.3105299952961229071, 0.3335123287862520880, 0.3564946622763812689, 0.4024593292566397418, 0.4484239962368982702, 0.4943886632171566875, 0.5403533301974150493, 0.5863179971776735222, 0.6322826641579321061, 0.6782473311381906900, 0.7242119981184491628, 0.7701766650987074136, 0.8161413320789658865, 0.8621059990592241373, 0.8735971658042887000, 0.8850883325493537068, 0.8965794992944182695, 0.9080706660394826102, 0.9195618327845473949, 0.9310529995296121797, 0.9425441662746769644, 0.9540353330197415271, 0.9770176665098706525, 1.000000000000000000 ),
 ( 0.000000000000000000, 0.5000000000000000000, 1.000000000000000000 ),
 .UNSPECIFIED. ) ;
#28941 = ORIENTED_EDGE ( 'NONE', *, *, #40560, .T. ) ;
#28942 = ORIENTED_EDGE ( 'NONE', *, *, #25895, .F. ) ;
#28943 = CARTESIAN_POINT ( 'NONE',  ( -1.580745382963060441, 115.6909491485438650, -1.732186872891357421 ) ) ;
#28944 = CARTESIAN_POINT ( 'NONE',  ( -3.461366646325571672, 118.6363893151611393, -0.9320101371334748031 ) ) ;
#28945 = CARTESIAN_POINT ( 'NONE',  ( -5.292905998138487611, 116.9650601603920279, -0.9543338394691547322 ) ) ;
#28946 = CARTESIAN_POINT ( 'NONE',  ( 4.666052514813301855, 117.8348563039157000, 1.040256194233742937 ) ) ;
#28947 = CARTESIAN_POINT ( 'NONE',  ( 3.026662605148213725, -13.87242449132548217, 1.205013440933411228 ) ) ;
#28948 = CARTESIAN_POINT ( 'NONE',  ( -9.710114326862248291, 153.9716628027005925, -1.336640340121901360 ) ) ;
#28949 = CARTESIAN_POINT ( 'NONE',  ( -0.1058213901579529159, 105.9761915687834914, 5.295735085524055030 ) ) ;
#28950 = FACE_OUTER_BOUND ( 'NONE', #25617, .T. ) ;
#28951 = CARTESIAN_POINT ( 'NONE',  ( 6.300894124712196565, 120.0808430858776887, -0.2013153013476511599 ) ) ;
#28952 = CARTESIAN_POINT ( 'NONE',  ( -3.458815983099662539, 120.0787590019544098, -0.7189451402107607247 ) ) ;
#28953 = EDGE_CURVE ( 'NONE', #38617, #14467, #39077, .T. ) ;
#28954 = CARTESIAN_POINT ( 'NONE',  ( 15.47023807670824525, 120.6682698389898576, 0.3091321738930620788 ) ) ;
#28955 = CARTESIAN_POINT ( 'NONE',  ( -6.341522686457216729, 28.91400451575042752, 0.4646910016499272156 ) ) ;
#28956 = CIRCLE ( 'NONE', #3812, 2.539999999999996483 ) ;
#28957 = LINE ( 'NONE', #12772, #19461 ) ;
#28958 = CARTESIAN_POINT ( 'NONE',  ( -2.070226828232369254, -8.352695179381779411, -4.151654383260235726 ) ) ;
#28960 = EDGE_LOOP ( 'NONE', ( #8166, #13120, #29543, #23541 ) ) ;
#28959 = CARTESIAN_POINT ( 'NONE',  ( 3.814135102937691979, 116.8938343318378088, 0.4443717020561036013 ) ) ;
#28961 = DIRECTION ( 'NONE',  ( -0.2883665106726583938, -0.9575201071113210727, 0.000000000000000000 ) ) ;
#28962 = CARTESIAN_POINT ( 'NONE',  ( 2.500182370989485925, -15.36189011820890471, 4.810483652035355107 ) ) ;
#28963 = CARTESIAN_POINT ( 'NONE',  ( -19.45999741126005489, 148.3988719805327037, 1.735632530687203579 ) ) ;
#28964 = CARTESIAN_POINT ( 'NONE',  ( 0.9435450883166688341, 2.505659174922684418, 0.2465458143858453577 ) ) ;
#28965 = CARTESIAN_POINT ( 'NONE',  ( 0.8400667230086624748, -1.857414735510459547, 0.5005776846920441114 ) ) ;
#28966 = ORIENTED_EDGE ( 'NONE', *, *, #10952, .T. ) ;
#28967 = ORIENTED_EDGE ( 'NONE', *, *, #22006, .T. ) ;
#28968 = CYLINDRICAL_SURFACE ( 'NONE', #16737, 0.2539999999999997260 ) ;
#28969 = CARTESIAN_POINT ( 'NONE',  ( 2.840201032364488842, 114.3344743418335128, 2.128718819835312637 ) ) ;
#28970 = CARTESIAN_POINT ( 'NONE',  ( -7.149839403334910415, 121.7184703992695773, 0.4778388566947555649 ) ) ;
#28971 = CARTESIAN_POINT ( 'NONE',  ( 3.948573903914379457, -12.48127506095717010, 1.805458641749257520 ) ) ;
#28972 = CARTESIAN_POINT ( 'NONE',  ( 5.873652769538419527, 120.2771794157441008, -0.8114825934776856986 ) ) ;
#28973 = CARTESIAN_POINT ( 'NONE',  ( -10.78248307147206475, 155.9024031350590462, -2.169211330499415613 ) ) ;
#28974 = CARTESIAN_POINT ( 'NONE',  ( -48.03056308610731406, 19.49280019387112972, -5.381938484679579915 ) ) ;
#28975 = CARTESIAN_POINT ( 'NONE',  ( 1.852819980464847305, -15.24972552306870455, 5.408883774200016425 ) ) ;
#28976 = CARTESIAN_POINT ( 'NONE',  ( -3.409494081961937706, 34.07961874667937963, 1.512047642211102216 ) ) ;
#28977 = EDGE_CURVE ( 'NONE', #34270, #3266, #10306, .T. ) ;
#28978 = CARTESIAN_POINT ( 'NONE',  ( 1.588992450109044663, 120.9073379818811134, -0.1002710119552033263 ) ) ;
#28979 = ORIENTED_EDGE ( 'NONE', *, *, #34248, .F. ) ;
#28980 = CARTESIAN_POINT ( 'NONE',  ( -17.14500000000466784, 71.11999999999886768, -1.524000000000000909 ) ) ;
#28981 = ADVANCED_FACE ( 'NONE', ( #33109 ), #825, .F. ) ;
#28982 = DIRECTION ( 'NONE',  ( -0.000000000000000000, -0.000000000000000000, -1.000000000000000000 ) ) ;
#28983 = EDGE_CURVE ( 'NONE', #33959, #38171, #41635, .T. ) ;
#28984 = VECTOR ( 'NONE', #25411, 1000.000000000000114 ) ;
#28985 = CARTESIAN_POINT ( 'NONE',  ( -4.580899860306842264, 27.87760619330545708, 0.5121266511161914892 ) ) ;
#28986 = AXIS2_PLACEMENT_3D ( 'NONE', #8973, #31542, #21940 ) ;
#28987 = CARTESIAN_POINT ( 'NONE',  ( 3.555938004931198382, 120.5283240077024800, 0.5587344792657806813 ) ) ;
#28988 = CARTESIAN_POINT ( 'NONE',  ( 10.92199999999999704, 55.24500000000000455, 0.000000000000000000 ) ) ;
#28989 = CARTESIAN_POINT ( 'NONE',  ( 21.90557141593800949, 151.4352167165723415, 0.3614719721193419555 ) ) ;
#28990 = AXIS2_PLACEMENT_3D ( 'NONE', #1096, #16843, #23210 ) ;
#28991 = CARTESIAN_POINT ( 'NONE',  ( -7.500421786656923828, 123.6595150816924047, -0.1155007223820209428 ) ) ;
#28992 = CARTESIAN_POINT ( 'NONE',  ( -4.645572480595541620, 117.9340260526530813, 0.7769932229682322555 ) ) ;
#28993 = DIRECTION ( 'NONE',  ( 0.9998004120163608288, 0.000000000000000000, 0.01997839162482736852 ) ) ;
#28994 = CARTESIAN_POINT ( 'NONE',  ( -4.761417829420920178, 31.88590546210041410, 0.3075751490760140205 ) ) ;
#28995 = CARTESIAN_POINT ( 'NONE',  ( 3.096092393556910238, 118.0390668470448929, 0.8277768005040343491 ) ) ;
#28996 = CARTESIAN_POINT ( 'NONE',  ( 4.103230867730633058, 22.16771668783608007, 2.168033597859526651 ) ) ;
#28997 = CARTESIAN_POINT ( 'NONE',  ( -8.368269197548203309, 31.49133049583987187, -0.7708832981534754492 ) ) ;
#28998 = CARTESIAN_POINT ( 'NONE',  ( -8.723683256387298357, 117.9901670288953284, -0.7589823086946332342 ) ) ;
#28999 = CARTESIAN_POINT ( 'NONE',  ( -1.733652500133141983, 120.5851793143259130, -0.4713357653683601378 ) ) ;
#29000 = CARTESIAN_POINT ( 'NONE',  ( -15.27962295839633811, 80.49293118800726177, -1.524000000000001576 ) ) ;
#29001 = DIRECTION ( 'NONE',  ( -0.9998501190848629872, -0.01731298258490734585, -8.537024980200777445E-16 ) ) ;
#29002 = CARTESIAN_POINT ( 'NONE',  ( 0.7256241136818852855, 104.6144662015456959, 4.780927069660905637 ) ) ;
#29003 = CARTESIAN_POINT ( 'NONE',  ( -3.366035089439492811, 13.68705809737886447, 3.178168622443589886 ) ) ;
#29004 = DIRECTION ( 'NONE',  ( 0.000000000000000000, 1.000000000000000000, 0.000000000000000000 ) ) ;
#29005 = CARTESIAN_POINT ( 'NONE',  ( 1.589478822742971486E-15, 16.51000000000000156, 0.000000000000000000 ) ) ;
#29006 = CARTESIAN_POINT ( 'NONE',  ( 2.768561164044480272, -13.57843041371762460, 0.3119852368007841603 ) ) ;
#29007 = CARTESIAN_POINT ( 'NONE',  ( 0.5468943487520009361, 107.2171362991012842, -4.774625097732313250 ) ) ;
#29008 = CARTESIAN_POINT ( 'NONE',  ( -2.881812722985489295, 116.8851979753409580, 0.3221759108904498903 ) ) ;
#29009 = ORIENTED_EDGE ( 'NONE', *, *, #31595, .F. ) ;
#29010 = CARTESIAN_POINT ( 'NONE',  ( 6.059261036834406866, 53.58606249999999704, 5.016499999999999737 ) ) ;
#29011 = EDGE_LOOP ( 'NONE', ( #12118, #22724, #12555, #14091 ) ) ;
#29012 = CARTESIAN_POINT ( 'NONE',  ( -43.40712238249138011, 21.47926646521734639, -2.288489392298376668 ) ) ;
#29013 = CARTESIAN_POINT ( 'NONE',  ( 5.875553665316252783, -14.89341971632543427, 0.3075322240006022056 ) ) ;
#29014 = CARTESIAN_POINT ( 'NONE',  ( -13.04666149862689828, 122.0079276396459704, 1.242691380407616286 ) ) ;
#29015 = CARTESIAN_POINT ( 'NONE',  ( 3.032027503100430899, 117.5448765310053005, -0.5892388327060570363 ) ) ;
#29016 = CARTESIAN_POINT ( 'NONE',  ( -3.609430071560130848, 3.966570591990036032, 2.889066364458971137 ) ) ;
#29017 = CARTESIAN_POINT ( 'NONE',  ( -55.11053650837317974, 7.076797490156363502, -3.243731704390616866 ) ) ;
#29018 = EDGE_CURVE ( 'NONE', #23764, #40944, #11693, .T. ) ;
#29019 = ORIENTED_EDGE ( 'NONE', *, *, #790, .T. ) ;
#29020 = CARTESIAN_POINT ( 'NONE',  ( -57.45676042280280171, 1.677525466749221650, -1.437765377950721346 ) ) ;
#29021 = AXIS2_PLACEMENT_3D ( 'NONE', #33518, #39705, #16890 ) ;
#29022 = CARTESIAN_POINT ( 'NONE',  ( 0.3576380314657462423, 120.7331730230137623, 0.5311352847986058334 ) ) ;
#29023 = CARTESIAN_POINT ( 'NONE',  ( -4.801647862234980302, 117.4032733357427105, 1.015449305853463491 ) ) ;
#29024 = CARTESIAN_POINT ( 'NONE',  ( -17.55799248491159759, 146.4615580561186050, 1.465990265564338868 ) ) ;
#29025 = DIRECTION ( 'NONE',  ( 0.000000000000000000, 0.000000000000000000, 1.000000000000000000 ) ) ;
#29026 = CARTESIAN_POINT ( 'NONE',  ( 5.876330432687248084, 119.7498067647950961, -0.9241301181796094388 ) ) ;
#29027 = CARTESIAN_POINT ( 'NONE',  ( -11.89465070410510883, 120.7721054874162974, -1.583610710261881049 ) ) ;
#29028 = CARTESIAN_POINT ( 'NONE',  ( -57.93941708942283952, 2.052042089854988483, -1.628789306319529118 ) ) ;
#29029 = EDGE_LOOP ( 'NONE', ( #39414, #15318, #13166, #10433 ) ) ;
#29030 = CARTESIAN_POINT ( 'NONE',  ( 4.466647412601136402, 118.1267704881138769, -0.5518082194138826946 ) ) ;
#29031 = CARTESIAN_POINT ( 'NONE',  ( 16.17919469456363757, 146.7365623387580342, -0.6462428564100393125 ) ) ;
#29032 = VERTEX_POINT ( 'NONE', #26709 ) ;
#29033 = CARTESIAN_POINT ( 'NONE',  ( -0.8526219981722428232, 157.1001331247151143, -1.466586365881669352 ) ) ;
#29034 = CARTESIAN_POINT ( 'NONE',  ( 2.939911579247540541, -15.51555475658629391, 4.434558482745560859 ) ) ;
#29035 = CARTESIAN_POINT ( 'NONE',  ( -4.065972646788793554, 118.2429491485453070, -0.3080848862740693250 ) ) ;
#29036 = VECTOR ( 'NONE', #1761, 1000.000000000000114 ) ;
#29037 = EDGE_CURVE ( 'NONE', #29982, #332, #30719, .T. ) ;
#29038 = CARTESIAN_POINT ( 'NONE',  ( -57.22211421646275653, 1.778355698664441098, -1.009576694067165286E-14 ) ) ;
#29039 = EDGE_CURVE ( 'NONE', #28714, #1088, #38863, .T. ) ;
#29040 = CARTESIAN_POINT ( 'NONE',  ( -4.947839762289965471, 117.6245774892788205, 0.7566444795842055537 ) ) ;
#29041 = CARTESIAN_POINT ( 'NONE',  ( 6.534901955148902708, 120.8223817900871495, 1.022280983926979303 ) ) ;
#29042 = CARTESIAN_POINT ( 'NONE',  ( -46.96231544241641842, 24.98353995950040840, 1.991484372665509595 ) ) ;
#29043 = CIRCLE ( 'NONE', #2560, 6.349999999999999645 ) ;
#29044 = CARTESIAN_POINT ( 'NONE',  ( 4.815508964495446520, -10.08105153662837061, -6.929324068793707880 ) ) ;
#29045 = CARTESIAN_POINT ( 'NONE',  ( 10.42406139656909758, 153.0845720789597522, 0.4157246174923903692 ) ) ;
#29046 = DIRECTION ( 'NONE',  ( 5.188838149069472160E-16, -1.699382548006136559E-16, -1.000000000000000000 ) ) ;
#29047 = CIRCLE ( 'NONE', #16795, 3.683000000000001162 ) ;
#29048 = CARTESIAN_POINT ( 'NONE',  ( -45.23155955595164812, 20.39474799592974463, -2.956275845755119924 ) ) ;
#29049 = CARTESIAN_POINT ( 'NONE',  ( -0.1313276950969750889, 117.9394518359770530, 1.405280662291707339 ) ) ;
#29050 = CARTESIAN_POINT ( 'NONE',  ( -46.60530155212503445, 26.17382724835477958, -1.270000000000008233 ) ) ;
#29051 = CARTESIAN_POINT ( 'NONE',  ( -51.04632475015682047, 14.57504837431617339, 4.679247123343607484 ) ) ;
#29052 = CARTESIAN_POINT ( 'NONE',  ( -8.314080580956096256, 119.9198965104016565, -1.454033707264238195 ) ) ;
#29053 = CARTESIAN_POINT ( 'NONE',  ( -27.88833342972739615, 78.11058938209563962, 1.269999999999991580 ) ) ;
#29054 = CARTESIAN_POINT ( 'NONE',  ( -5.241362157049125337, 53.58606249999999704, -5.310945289804168468 ) ) ;
#29055 = CARTESIAN_POINT ( 'NONE',  ( -56.90576330281450623, 4.524090327013369439, 2.207515467630526196 ) ) ;
#29056 = CARTESIAN_POINT ( 'NONE',  ( -56.82628769568140115, 4.502340570254503405, 2.499646007873237430 ) ) ;
#29057 = CARTESIAN_POINT ( 'NONE',  ( -5.816519783795449428, 117.0096406922080376, 0.1181936270109639059 ) ) ;
#29058 = ORIENTED_EDGE ( 'NONE', *, *, #19707, .T. ) ;
#29059 = CARTESIAN_POINT ( 'NONE',  ( -53.63638764239521350, 11.23543775674477807, -3.971736527645129744 ) ) ;
#29060 = CARTESIAN_POINT ( 'NONE',  ( 7.817500836422443200, 122.5000612203145778, -0.1730797909992374539 ) ) ;
#29061 = EDGE_LOOP ( 'NONE', ( #22001, #33636, #37886, #5115 ) ) ;
#29062 = CARTESIAN_POINT ( 'NONE',  ( 3.014263063806961185, 115.7029722995355741, -1.552917389829764572 ) ) ;
#29063 = CARTESIAN_POINT ( 'NONE',  ( -9.045001602728936163, 123.9859359328134190, -0.2652644514531632969 ) ) ;
#29064 = CARTESIAN_POINT ( 'NONE',  ( 4.978007909399718045, -14.21992039213325398, 4.057701602070913793 ) ) ;
#29065 = CARTESIAN_POINT ( 'NONE',  ( -15.22748671137947518, 123.1171956318823533, 1.061527106655570707 ) ) ;
#29066 = CARTESIAN_POINT ( 'NONE',  ( 5.348924234570989533, 56.51499999999999346, -4.492130288940734850 ) ) ;
#29067 = CARTESIAN_POINT ( 'NONE',  ( 23.26558566580226639, 149.3390083238215595, 0.6953334291057012839 ) ) ;
#29068 = AXIS2_PLACEMENT_3D ( 'NONE', #34577, #27958, #34364 ) ;
#29069 = CARTESIAN_POINT ( 'NONE',  ( 1.634769624693551027, 120.9957931938675841, 0.1332809887664035686 ) ) ;
#29070 = CARTESIAN_POINT ( 'NONE',  ( -6.059261036834082681, 78.87450423423038615, 5.016499999999999737 ) ) ;
#29071 = CARTESIAN_POINT ( 'NONE',  ( 0.8411255309083253140, 9.366862202269544468, -0.4933303560167117130 ) ) ;
#29072 = CARTESIAN_POINT ( 'NONE',  ( -20.68667083660097816, 152.5691845998198346, -0.5628278541506290811 ) ) ;
#29073 = DIRECTION ( 'NONE',  ( -1.011795553208986377E-16, -1.000000000000000000, 0.000000000000000000 ) ) ;
#29074 = DIRECTION ( 'NONE',  ( 0.1469470846586743706, 9.335746474409589170E-17, 0.9891443546370348727 ) ) ;
#29075 = ORIENTED_EDGE ( 'NONE', *, *, #16675, .T. ) ;
#29076 = CARTESIAN_POINT ( 'NONE',  ( 5.537890225724539484, 117.2894663389777463, 0.8086631719369541393 ) ) ;
#29077 = ORIENTED_EDGE ( 'NONE', *, *, #13171, .F. ) ;
#29078 = DIRECTION ( 'NONE',  ( 0.9998004120163608288, 0.000000000000000000, 0.01997839162482760791 ) ) ;
#29079 = CARTESIAN_POINT ( 'NONE',  ( 20.92851329017031148, 150.0074445146613584, 2.223361304733721955 ) ) ;
#29080 = CARTESIAN_POINT ( 'NONE',  ( 5.018689047519269586, 118.8869175073591578, -0.8997529482361044106 ) ) ;
#29081 = CARTESIAN_POINT ( 'NONE',  ( -3.928768625441322104, 16.54256788600693895, -7.448509604454663702 ) ) ;
#29082 = CARTESIAN_POINT ( 'NONE',  ( -4.887760029584870658, 117.7409041207840090, -0.8724161813180755232 ) ) ;
#29083 = CARTESIAN_POINT ( 'NONE',  ( 4.706159131466354673, 117.8933722103456887, -0.8009178487074127828 ) ) ;
#29084 = CARTESIAN_POINT ( 'NONE',  ( -13.79703500197642896, 79.79115557309579287, -1.270000000000000462 ) ) ;
#29085 = VECTOR ( 'NONE', #24080, 1000.000000000000000 ) ;
#29086 = CARTESIAN_POINT ( 'NONE',  ( -14.67586190579459604, 148.8475317811793559, -0.2426438148417037477 ) ) ;
#29087 = CARTESIAN_POINT ( 'NONE',  ( -12.85862358090732194, 153.8477531742089468, -2.225956515383983092 ) ) ;
#29088 = EDGE_CURVE ( 'NONE', #700, #18747, #1157, .T. ) ;
#29089 = CARTESIAN_POINT ( 'NONE',  ( 4.032098335577404491, -15.72255795053374783, 4.298576634473052493 ) ) ;
#29090 = CARTESIAN_POINT ( 'NONE',  ( 4.726447923106682047, 118.5931160184169073, 1.020546415897938708 ) ) ;
#29091 = ADVANCED_FACE ( 'NONE', ( #23700 ), #28688, .T. ) ;
#29092 = CARTESIAN_POINT ( 'NONE',  ( -46.68395179480138779, 26.03198510454123848, -1.524000000000008459 ) ) ;
#29093 = VERTEX_POINT ( 'NONE', #1786 ) ;
#29094 = CARTESIAN_POINT ( 'NONE',  ( 18.30884121703834921, 147.6341482083243761, 2.394331140672893099 ) ) ;
#29095 = CARTESIAN_POINT ( 'NONE',  ( 11.58677707360137532, 12.96416000000000146, 4.474811398758259173 ) ) ;
#29096 = CARTESIAN_POINT ( 'NONE',  ( -10.53334313995851446, 65.32054992887103140, -1.269999999999996465 ) ) ;
#29097 = AXIS2_PLACEMENT_3D ( 'NONE', #12217, #31602, #5636 ) ;
#29098 = CARTESIAN_POINT ( 'NONE',  ( -4.981054720647350109, 121.2162878128435892, 0.1538846217318252940 ) ) ;
#29099 = CARTESIAN_POINT ( 'NONE',  ( -1.630640499631123452, 19.93121390510496838, -8.274862188801900942 ) ) ;
#29100 = CARTESIAN_POINT ( 'NONE',  ( 9.448695200928735716, 153.9068681542131856, 1.043141309954137563 ) ) ;
#29101 = CARTESIAN_POINT ( 'NONE',  ( 6.911158149689221375, 117.5201695557886410, -0.4259063301137958613 ) ) ;
#29102 = CARTESIAN_POINT ( 'NONE',  ( 5.332935392244917416, 115.7029491189645825, 0.1065647408284378928 ) ) ;
#29103 = CARTESIAN_POINT ( 'NONE',  ( 4.581731014592691054, -15.30239759458089388, -0.5121113081912510578 ) ) ;
#29104 = UNCERTAINTY_MEASURE_WITH_UNIT (LENGTH_MEASURE( 1.000000000000000082E-05 ), #24013, 'distance_accuracy_value', 'NONE');
#29105 = CARTESIAN_POINT ( 'NONE',  ( -14.90010799439755651, 120.3262451489332818, -0.2810636626631669022 ) ) ;
#29106 = EDGE_LOOP ( 'NONE', ( #26032, #38316, #34800, #29882 ) ) ;
#29107 = CARTESIAN_POINT ( 'NONE',  ( 4.708107117004457720, 119.7860639267805283, -0.7247629778888364793 ) ) ;
#29108 = CARTESIAN_POINT ( 'NONE',  ( 4.376067305622965975, -15.09428741806564034, 4.801372945859158747 ) ) ;
#29109 = CARTESIAN_POINT ( 'NONE',  ( -9.499123264218946261, 124.0643708016488063, -0.7086372128104243551 ) ) ;
#29110 = CARTESIAN_POINT ( 'NONE',  ( 3.889980283446199838, -12.05568003970028457, 1.127423567058935205 ) ) ;
#29111 = CARTESIAN_POINT ( 'NONE',  ( -5.878298779570172883, 78.21245918282636467, -1.523999999999996247 ) ) ;
#29112 = CARTESIAN_POINT ( 'NONE',  ( 14.89944180985295574, 120.3262451489332818, 0.3144022614128134108 ) ) ;
#29113 = ORIENTED_EDGE ( 'NONE', *, *, #8114, .F. ) ;
#29114 = CARTESIAN_POINT ( 'NONE',  ( -4.374560056058969693, 13.03735028915297534, 1.504755201125916875 ) ) ;
#29115 = CARTESIAN_POINT ( 'NONE',  ( -1.165688202727937828, 105.1231265544458466, 5.215447108397309073 ) ) ;
#29116 = DIRECTION ( 'NONE',  ( 9.627370216492862708E-17, 1.000000000000000000, -0.000000000000000000 ) ) ;
#29117 = CARTESIAN_POINT ( 'NONE',  ( 0.4456520612264974202, 105.8204370143460693, 5.321309051583069660 ) ) ;
#29118 = DIRECTION ( 'NONE',  ( 0.8745520943968240202, -0.4849315768086551182, 4.268512490100404500E-16 ) ) ;
#29119 = CARTESIAN_POINT ( 'NONE',  ( 6.106687141107508765, 121.1151792713842781, 0.7286823287528870763 ) ) ;
#29120 = CARTESIAN_POINT ( 'NONE',  ( 3.912982837994093188, 14.17146771520798332, -2.459658384584827218 ) ) ;
#29121 = CARTESIAN_POINT ( 'NONE',  ( 5.838122194618472705, 117.4684171610355747, 0.7518181979692857286 ) ) ;
#29122 = CARTESIAN_POINT ( 'NONE',  ( -6.059261036834474368, 56.51499999999998636, -4.381499999999999950 ) ) ;
#29124 = CARTESIAN_POINT ( 'NONE',  ( 7.864631202759840178, 118.9574329095587757, -0.9664042006415772823 ) ) ;
#29123 = CARTESIAN_POINT ( 'NONE',  ( 2.697962015452238571, 107.8418472309013794, 4.476687650674952224 ) ) ;
#29125 = CARTESIAN_POINT ( 'NONE',  ( -4.422273941422524501, 8.986318502778324557, 1.404945367500548548 ) ) ;
#29126 = CARTESIAN_POINT ( 'NONE',  ( -22.82453445504512857, 148.6346580502994073, -1.538154475459324821 ) ) ;
#29127 = ORIENTED_EDGE ( 'NONE', *, *, #4770, .F. ) ;
#29128 = CARTESIAN_POINT ( 'NONE',  ( -7.884012465051817742, 154.6027768716304820, 0.2197914096094752134 ) ) ;
#29129 = CARTESIAN_POINT ( 'NONE',  ( 4.359322289182287591, -14.87073230766630694, 4.862486896750754184 ) ) ;
#29130 = FACE_OUTER_BOUND ( 'NONE', #4620, .T. ) ;
#29131 = EDGE_CURVE ( 'NONE', #2172, #16499, #30062, .T. ) ;
#29132 = VERTEX_POINT ( 'NONE', #4986 ) ;
#29133 = CARTESIAN_POINT ( 'NONE',  ( -0.03212618750959795461, 158.2819368290249713, 1.607725792532325615 ) ) ;
#29134 = DIRECTION ( 'NONE',  ( -0.9998004120163610509, -4.016384292689131511E-17, -0.01997839162482749689 ) ) ;
#29135 = LINE ( 'NONE', #25733, #107 ) ;
#29136 = AXIS2_PLACEMENT_3D ( 'NONE', #32625, #22378, #28801 ) ;
#29137 = CARTESIAN_POINT ( 'NONE',  ( -22.86776170061665425, 148.6346580502994073, 0.6251136566479099654 ) ) ;
#29138 = CARTESIAN_POINT ( 'NONE',  ( 4.865100810417520627, 117.4776273858779234, -0.9871917231070708176 ) ) ;
#29139 = CARTESIAN_POINT ( 'NONE',  ( 5.699072711719705531, 159.1209727096294273, -0.1881040421785056538 ) ) ;
#29140 =( BOUNDED_SURFACE ( )  B_SPLINE_SURFACE ( 3, 3, ( 
 ( #7657, #20614, #33644, #4471, #17429, #1273, #28282, #8903, #11885, #17845, #21241, #8488, #37447, #27649, #34271, #15493, #21038, #27859, #2317, #8271, #5099, #30844, #41077, #41289, #18681, #34681, #2102, #5307, #18051, #24874, #31054, #37869, #8693, #1691, #12093, #12307, #21656, #5510, #14855, #21444, #1893, #34473, #18468, #40867, #31689, #24443, #28066, #15278, #25295, #18256, #14646, #11668, #24655, #31260, #25081, #2531, #4890, #37664, #41500, #15066, #34063, #31473, #21869, #38088, #34895, #5726, #28491, #8063, #40660, #11452, #5932, #9322, #38716, #25506, #15694, #22285, #3581, #9118, #15905, #32529, #38506, #35310, #18893, #29114, #29333, #6759, #22705, #32318, #35521, #6138, #42132, #19102, #12929, #38927, #31902, #174, #387, #25919, #35107, #22080, #19727, #6342, #32110, #2941, #9526, #22494, #3147, #9737, #16543, #28905, #13144, #13353, #41920, #35735, #19313, #6547, #29553, #12720, #16110, #2738, #19521, #3360, #38298, #28700, #16327, #26136, #35947, #9943, #25710, #39137, #22915, #41709, #32748, #12515, #30376, #802, #23341, #13777, #20567, #7195, #36998, #23124, #39566, #36789, #33804, #26774, #33595, #4428, #13570, #1015, #29758, #32968, #29962, #17386, #1431, #39784, #1226, #4632, #10370, #14185, #20780, #23557, #10579, #7394, #36161, #27188, #3793, #26984, #20153, #13979, #4004, #40203, #10999, #17175, #36578, #33176, #16962, #20355, #597, #6977, #33379, #26559, #4213, #36379, #30174, #39994, #23979, #7818, #10785, #19949, #17588, #30591, #26343, #23765, #39350, #10153, #7606, #16753 ),
 ( #2271, #12045, #28234, #40611, #21395, #1844, #37198, #18209, #34849, #18421, #31001, #11410, #14808, #8645, #37401, #25034, #11203, #27601, #24823, #21821, #27810, #21606, #34634, #1642, #31210, #17795, #20990, #18004, #5461, #31644, #40818, #31429, #5681, #24397, #15235, #8857, #11619, #24606, #37611, #24188, #2053, #21193, #8437, #8220, #34422, #15018, #5049, #38037, #30792, #5255, #41240, #18639, #28018, #34012, #34219, #41028, #11836, #14390, #27397, #8019, #37818, #40408, #4841, #14596, #35475, #16280, #38879, #12679, #19270, #42090, #22658, #3314, #6299, #12259, #15650, #2900, #31854, #22038, #28655, #9895, #15446, #22243, #9691, #2693, #41667, #25251, #32277, #35691, #13094, #35269, #28449, #3107, #29285, #6500, #25669, #16068, #12885, #19478, #129, #29071, #38256, #12475, #15862, #25469, #35066, #38465, #22868, #41454, #6093, #32486, #9283, #19056, #9073, #25873, #26086, #39093, #35906, #38676, #41880, #32061, #6715, #28868, #19684, #2484, #5888, #18849, #9482, #22446, #29501, #16495, #14137, #757, #32915, #3745, #33127, #3957, #26726, #7349, #40152, #19900, #36736, #8333, #26512, #23502, #13732, #967, #11517, #29708, #39734, #341, #20308, #36529, #24502, #26294, #10533, #20519, #30328, #4380, #16703, #33334, #20103, #13307, #4164, #37507, #7559, #7146, #550, #16918, #26932, #13524, #1174, #39302, #39517, #13936, #32700, #29918, #39944, #10736, #10323, #17127, #36115, #10110, #36330, #23717, #3536, #30128, #33549, #23081, #23292, #17338, #27139, #6929, #24937, #2382, #31119, #8967, #28130, #21720 ),
 ( #41356, #28557, #25564, #31538, #27920, #5368, #11946, #34744, #38366, #15759, #18114, #2168, #12577, #31324, #5576, #21935, #37935, #2801, #37725, #12159, #41565, #38568, #15342, #40926, #18322, #8759, #18533, #9180, #28763, #1956, #15127, #21303, #28347, #34332, #25151, #35166, #15555, #38154, #34964, #18742, #12374, #22137, #5787, #14916, #34541, #31752, #8549, #11732, #41140, #41777, #5160, #2595, #25361, #21508, #5993, #24721, #18956, #31962, #20006, #36005, #3420, #6608, #9587, #232, #32378, #26191, #10003, #3007, #13415, #13625, #13209, #6198, #35368, #33023, #19579, #22556, #35586, #9797, #22763, #16387, #39195, #16816, #38776, #26404, #26616, #3207, #22975, #32587, #19787, #29818, #6403, #29392, #19168, #6817, #32806, #657, #15966, #3637, #39409, #7038, #23182, #19372, #16602, #38987, #32171, #29610, #9381, #10212, #25979, #16169, #35796, #445, #29174, #3852, #28964, #20, #36217, #22345, #41980, #12779, #25769, #12986, #14242, #862, #4064, #1070, #30650, #14658, #14038, #1494, #17857, #10637, #17648, #34076, #36850, #27042, #20626, #7250, #27249, #4272, #40051, #33863, #39840, #26833, #20209, #30438, #14450, #8077, #24043, #33656, #7668, #23616, #1284, #20417, #40265, #11058, #33236, #27460, #1703, #37058, #36431, #23400, #21050, #4481, #36637, #7459, #10844, #23830, #17441, #7876, #4903, #33445, #40473, #39623, #17235, #20839, #4693, #11264, #30858, #30231, #24250, #17024, #37258, #10429, #30022, #13835, #8706, #15505, #25307, #41513, #11681, #34693, #15078, #8284, #31485, #5946, #31702, #2115 ),
 ( #40880, #38100, #35119, #28078, #21881, #5739, #14869, #2330, #31067, #34283, #31272, #18692, #2752, #41089, #2544, #18905, #24667, #28506, #22092, #24886, #11897, #21670, #37459, #15290, #34486, #37883, #37676, #5523, #28295, #18270, #9131, #1905, #18480, #34907, #31916, #41302, #5112, #8499, #12106, #25096, #12320, #27662, #24455, #21456, #40673, #8915, #11466, #38311, #21253, #18064, #27871, #5318, #13155, #35957, #16554, #19532, #25518, #28916, #16122, #2953, #35323, #41931, #23133, #28712, #35535, #6771, #15916, #32539, #19116, #22298, #19325, #19737, #32977, #32329, #32759, #36172, #12732, #3592, #10165, #12939, #3158, #38937, #38518, #3372, #22506, #29125, #25721, #42145, #16338, #6354, #39360, #32122, #35745, #22926, #19959, #25930, #6149, #38729, #9749, #22717, #29562, #6989, #12527, #9536, #15708, #6557, #41722, #29344, #398, #9953, #185, #26147, #39149, #13365, #26354, #9335, #13581, #16973, #4226, #33188, #23352, #29972, #11215, #16764, #23567, #40213, #4016, #813, #26569, #36800, #37010, #14401, #30388, #40006, #1026, #13788, #7619, #26785, #20579, #4438, #39577, #7828, #8030, #33606, #607, #29771, #27409, #13990, #39795, #10589, #17186, #30185, #10797, #17396, #24199, #36589, #20790, #21001, #7407, #1239, #26995, #14195, #37210, #20369, #23779, #10382, #27200, #11011, #3802, #36389, #23990, #33815, #1441, #17599, #33391, #4642, #30603, #7205, #40420, #20163, #38047, #8448, #31013, #21405, #28245, #14819, #2494, #30804, #5061, #2280, #41464, #34433, #41249, #37624, #8867, #12271, #18016, #12055 ),
 ( #1856, #28458, #14608, #27821, #5267, #31438, #38265, #18648, #15244, #2064, #9082, #40623, #40830, #11629, #25044, #15457, #34858, #11421, #34231, #24616, #18219, #31220, #15028, #28028, #31654, #27613, #18430, #24407, #41038, #11848, #25260, #24834, #37829, #5690, #17807, #34026, #4851, #8656, #21205, #21616, #8232, #34643, #5471, #37413, #21829, #1654, #2703, #16292, #15872, #32497, #15660, #29081, #19067, #16077, #32073, #9702, #19488, #19280, #38686, #2909, #28879, #12689, #12484, #31863, #41891, #25479, #9492, #38474, #25679, #22253, #29296, #3325, #22457, #28664, #9907, #35702, #139, #35486, #6513, #13106, #9292, #41676, #6308, #39104, #35279, #6104, #26098, #32288, #35076, #3117, #42100, #12895, #25883, #38890, #22669, #22879, #35917, #22048, #5897, #18859, #5395, #37539, #38184, #2413, #34776, #9001, #5188, #1776, #8362, #21329, #11973, #22169, #14737, #21749, #21968, #37751, #31145, #12190, #27740, #41596, #28164, #18141, #1986, #18351, #31357, #24966, #5610, #25398, #14948, #34998, #35200, #11763, #8791, #41169, #28378, #38400, #27948, #37966, #40750, #18566, #31573, #9212, #11547, #15373, #5818, #15583, #31784, #40957, #41385, #2200, #24530, #25184, #17934, #18774, #34568, #24752, #15158, #2624, #8575, #28588, #34356, #21538, #12406, #30937, #35618, #264, #26222, #35401, #22794, #9409, #12608, #9618, #39226, #23215, #22586, #10036, #26437, #19199, #23008, #476, #3243, #6432, #29207, #15790, #35829, #12810, #19406, #15998, #32413, #6645, #38806, #29639, #22375, #26010, #13238, #10244, #16202, #25595 ),
 ( #28997, #39441, #50, #18988, #39019, #19820, #36036, #13016, #19609, #3455, #6851, #32837, #9827, #28798, #32207, #32622, #6228, #38603, #3040, #13449, #31992, #25800, #3666, #42014, #16417, #41812, #29423, #16632, #6026, #2830, #30260, #33476, #36458, #27072, #17053, #10875, #36882, #29847, #40295, #40500, #40080, #33052, #23863, #11088, #13867, #7277, #30469, #14270, #11296, #26861, #7700, #20661, #36668, #1101, #20239, #33687, #3882, #33265, #30677, #16847, #4094, #7489, #4511, #36248, #20869, #17472, #4306, #7069, #685, #30055, #893, #1314, #4723, #37087, #13657, #39869, #10665, #23646, #20449, #17269, #14068, #33893, #26647, #27281, #39655, #24075, #7905, #17676, #1525, #14481, #27492, #20033, #10459, #23429, #10927, #4779, #17107, #37340, #11350, #17321, #4361, #26911, #7957, #8159, #27747, #1580, #11140, #14323, #30311, #20925, #40135, #33948, #17729, #10717, #21128, #21335, #30731, #13918, #949, #40757, #27334, #1155, #14120, #17524, #30524, #24126, #14537, #24538, #27120, #34157, #34362, #23916, #27546, #40346, #40552, #37546, #36932, #37136, #39924, #24336, #4984, #8369, #23698, #17942, #30944, #14745, #1784, #7751, #11554, #4565, #36718, #30109, #7540, #20501, #33741, #20717, #1364, #33528, #28171, #15795, #1992, #18357, #15588, #12614, #34783, #41602, #25404, #34574, #21972, #9007, #14954, #31363, #5616, #5400, #24758, #41175, #35004, #5194, #38406, #12411, #2206, #15164, #27955, #38190, #9217, #28803, #31790, #41391, #2419, #11979, #5823, #24973, #18779, #2629, #40963, #22174, #9415, #28593 ),
 ( #18572, #31580, #12196, #35205, #25601, #37972, #6031, #22382, #8797, #18993, #15379, #31997, #38609, #21755, #28385, #31151, #2836, #41820, #18148, #11768, #25188, #37757, #8581, #21544, #19412, #270, #22800, #16004, #39232, #13663, #39447, #9833, #32419, #35835, #29645, #16209, #3889, #32213, #6438, #3673, #690, #6651, #483, #13456, #22592, #10041, #38811, #42020, #39025, #26443, #10466, #19615, #10250, #26655, #3249, #23223, #29853, #32628, #3461, #16425, #3046, #23014, #56, #29429, #29213, #13244, #36042, #26016, #16853, #9625, #26228, #36255, #39662, #6857, #12817, #13024, #19828, #32843, #7076, #35407, #29003, #16637, #6235, #20039, #19205, #33058, #25805, #35624, #33693, #40302, #20876, #1532, #24287, #40708, #17277, #14277, #4517, #33901, #1737, #20455, #17479, #7284, #11095, #27287, #14695, #17059, #30476, #11302, #21084, #37292, #7495, #1320, #10882, #4100, #24082, #27701, #27500, #40086, #33483, #23869, #17682, #4313, #34109, #20245, #36674, #4730, #30897, #36889, #30683, #14487, #10672, #37093, #26867, #30063, #27078, #40507, #23435, #7706, #8110, #36464, #30266, #4936, #17895, #20669, #7911, #33271, #900, #13874, #1107, #39875, #14075, #23653, #12143, #2152, #35153, #27906, #31523, #18727, #15744, #21704, #18102, #37711, #15112, #24922, #28543, #5979, #8320, #34527, #2787, #28115, #24490, #2367, #25347, #5773, #34729, #28332, #8953, #31737, #12359, #15325, #21291, #24706, #11930, #40913, #31106, #5352, #41341, #11504, #2581, #15542, #11719, #8534, #34319, #25135, #41551, #22123, #38138, #5560 ) ),
 .UNSPECIFIED., .T., .F., .F. ) 
 B_SPLINE_SURFACE_WITH_KNOTS ( ( 4, 3, 4 ),
 ( 4, 1, 1, 1, 1, 1, 1, 1, 1, 1, 1, 1, 1, 1, 1, 1, 1, 1, 1, 1, 1, 1, 1, 1, 1, 1, 1, 1, 1, 1, 1, 1, 1, 1, 1, 1, 1, 1, 1, 1, 1, 1, 1, 1, 1, 1, 1, 1, 1, 1, 1, 1, 1, 1, 1, 1, 1, 1, 1, 1, 1, 1, 1, 1, 1, 1, 1, 1, 1, 1, 1, 1, 1, 1, 1, 1, 1, 1, 1, 1, 1, 1, 1, 1, 1, 1, 1, 1, 1, 1, 1, 1, 1, 1, 1, 1, 1, 1, 1, 1, 1, 1, 1, 1, 1, 1, 1, 1, 1, 1, 1, 1, 1, 1, 1, 1, 1, 1, 1, 1, 1, 1, 1, 1, 1, 1, 1, 1, 1, 1, 1, 1, 1, 1, 1, 1, 1, 1, 1, 1, 1, 1, 1, 1, 1, 1, 1, 1, 1, 1, 1, 1, 1, 1, 1, 1, 1, 1, 1, 1, 1, 1, 1, 1, 1, 1, 1, 1, 1, 1, 1, 1, 1, 1, 1, 1, 1, 1, 1, 1, 1, 1, 1, 1, 1, 1, 1, 1, 1, 1, 1, 1, 3, 4 ),
 ( 0.000000000000000000, 0.5000000000000000000, 1.000000000000000000 ),
 ( 0.000000000000000000, 0.007812500000000423273, 0.01388888888888889506, 0.01562500000000000000, 0.02343749999999998959, 0.02777777777777778317, 0.03125000000000092981, 0.03906249999999999306, 0.04166666666666667823, 0.04687500000000000000, 0.05468749999999999306, 0.05555555555555556635, 0.06249999999999997918, 0.06944444444444446141, 0.07031250000000000000, 0.07812500000000000000, 0.08333333333333334259, 0.08593749999999998612, 0.09374999999999603095, 0.09722222222222223764, 0.1015625000000000139, 0.1093750000000000000, 0.1111111111111111188, 0.1171875000000000000, 0.1250000000000000000, 0.1328125000000000000, 0.1388888888888889228, 0.1406250000000000000, 0.1484375000000000000, 0.1527777777777778179, 0.1562500000000039690, 0.1640625000000000000, 0.1666666666666666852, 0.1718750000000000000, 0.1796875000000000000, 0.1805555555555555802, 0.1875000000000000000, 0.1944444444444444753, 0.1953125000000000000, 0.2031250000000000000, 0.2083333333333333703, 0.2109375000000000000, 0.2187499999999960310, 0.2222222222222222376, 0.2265625000000000000, 0.2343750000000000000, 0.2361111111111111327, 0.2421875000000000000, 0.2500000000000000000, 0.2578125000000000000, 0.2638888888888888951, 0.2656250000000000000, 0.2734375000000000000, 0.2777777777777777346, 0.2812500000000039968, 0.2890625000000000000, 0.2916666666666665741, 0.2968750000000000000, 0.3046875000000000000, 0.3055555555555554692, 0.3125000000000000000, 0.3194444444444443088, 0.3203125000000000000, 0.3281250000000000000, 0.3333333333333332038, 0.3359375000000000000, 0.3437499999999960587, 0.3472222222222220434, 0.3515625000000000000, 0.3593750000000000000, 0.3611111111111109384, 0.3671875000000000000, 0.3750000000000000000, 0.3828125000000000000, 0.3888888888888886175, 0.3906250000000000000, 0.3984375000000000000, 0.4027777777777775126, 0.4062500000000039968, 0.4140625000000000000, 0.4166666666666663521, 0.4218750000000000000, 0.4296875000000000000, 0.4305555555555552472, 0.4375000000000000000, 0.4444444444444440867, 0.4453125000000000000, 0.4531250000000000000, 0.4583333333333329818, 0.4609375000000000000, 0.4687499999999960587, 0.4722222222222218768, 0.4765625000000000000, 0.4843750000000000000, 0.4861111111111107719, 0.4921875000000000000, 0.5000000000000000000, 0.5078125000000000000, 0.5138888888888886175, 0.5156250000000000000, 0.5234375000000000000, 0.5277777777777775681, 0.5312500000000039968, 0.5390625000000000000, 0.5416666666666664076, 0.5468750000000000000, 0.5546875000000000000, 0.5555555555555553582, 0.5625000000000000000, 0.5694444444444443088, 0.5703125000000000000, 0.5781250000000000000, 0.5833333333333331483, 0.5859375000000000000, 0.5937499999999960032, 0.5972222222222220989, 0.6015625000000000000, 0.6093750000000000000, 0.6111111111111110494, 0.6171875000000000000, 0.6250000000000000000, 0.6328125000000000000, 0.6388888888888888395, 0.6406250000000000000, 0.6484375000000000000, 0.6527777777777777901, 0.6562500000000039968, 0.6640625000000000000, 0.6666666666666666297, 0.6718750000000000000, 0.6796875000000000000, 0.6805555555555555802, 0.6875000000000000000, 0.6944444444444445308, 0.6953125000000000000, 0.7031250000000000000, 0.7083333333333333703, 0.7109375000000000000, 0.7187499999999960032, 0.7222222222222223209, 0.7265625000000000000, 0.7343750000000000000, 0.7361111111111111605, 0.7421875000000000000, 0.7500000000000000000, 0.7578125000000000000, 0.7638888888888889506, 0.7656250000000000000, 0.7734375000000000000, 0.7777777777777779011, 0.7812500000000039968, 0.7890625000000000000, 0.7916666666666668517, 0.7968750000000000000, 0.8046875000000000000, 0.8055555555555556912, 0.8125000000000000000, 0.8194444444444446418, 0.8203125000000000000, 0.8281250000000000000, 0.8333333333333335924, 0.8359375000000000000, 0.8437499999999960032, 0.8472222222222224319, 0.8515625000000000000, 0.8593750000000000000, 0.8611111111111113825, 0.8671875000000000000, 0.8750000000000000000, 0.8828125000000000000, 0.8888888888888891726, 0.8906250000000000000, 0.8984375000000000000, 0.9027777777777781232, 0.9062500000000039968, 0.9140625000000000000, 0.9166666666666670737, 0.9218750000000000000, 0.9296875000000000000, 0.9305555555555559133, 0.9375000000000000000, 0.9444444444444447528, 0.9453125000000000000, 0.9531250000000000000, 0.9583333333333335924, 0.9609375000000000000, 0.9687499999999991118, 0.9722222222222224319, 0.9765625000000000000, 0.9843750000000000000, 0.9861111111111111605, 0.9921874999999995559, 1.000000000000000000, 1.000012325855852646 ),
 .UNSPECIFIED. ) 
 GEOMETRIC_REPRESENTATION_ITEM ( )  RATIONAL_B_SPLINE_SURFACE ( (
 ( 1.000000000000000000, 1.000000000000000000, 1.000000000000000000, 1.000000000000000000, 1.000000000000000000, 1.000000000000000000, 0.9999999999999998890, 0.9999999999999997780, 1.000000000000000000, 1.000000000000000000, 1.000000000000000000, 1.000000000000000000, 1.000000000000000000, 1.000000000000000000, 0.9999999999999998890, 1.000000000000000000, 1.000000000000000222, 1.000000000000000000, 1.000000000000000000, 1.000000000000000000, 1.000000000000000000, 1.000000000000000000, 0.9999999999999998890, 0.9999999999999997780, 1.000000000000000000, 1.000000000000000222, 1.000000000000000000, 1.000000000000000000, 1.000000000000000000, 1.000000000000000000, 0.9999999999999998890, 0.9999999999999997780, 1.000000000000000000, 0.9999999999999998890, 0.9999999999999997780, 1.000000000000000000, 1.000000000000000222, 1.000000000000000222, 1.000000000000000000, 1.000000000000000000, 1.000000000000000222, 1.000000000000000000, 0.9999999999999997780, 1.000000000000000000, 1.000000000000000000, 1.000000000000000000, 1.000000000000000000, 1.000000000000000000, 1.000000000000000000, 1.000000000000000222, 1.000000000000000222, 1.000000000000000000, 1.000000000000000000, 1.000000000000000222, 1.000000000000000222, 1.000000000000000222, 1.000000000000000000, 1.000000000000000000, 1.000000000000000222, 1.000000000000000000, 1.000000000000000000, 1.000000000000000222, 1.000000000000000000, 1.000000000000000000, 1.000000000000000222, 1.000000000000000000, 1.000000000000000000, 0.9999999999999997780, 0.9999999999999998890, 1.000000000000000000, 1.000000000000000000, 1.000000000000000000, 1.000000000000000000, 1.000000000000000222, 1.000000000000000222, 1.000000000000000000, 1.000000000000000000, 1.000000000000000222, 1.000000000000000222, 1.000000000000000222, 1.000000000000000000, 1.000000000000000000, 1.000000000000000222, 1.000000000000000000, 1.000000000000000000, 1.000000000000000222, 1.000000000000000000, 1.000000000000000000, 1.000000000000000222, 1.000000000000000000, 1.000000000000000000, 0.9999999999999997780, 0.9999999999999998890, 1.000000000000000000, 1.000000000000000000, 1.000000000000000000, 1.000000000000000000, 1.000000000000000222, 1.000000000000000222, 1.000000000000000000, 1.000000000000000000, 1.000000000000000222, 1.000000000000000222, 1.000000000000000222, 1.000000000000000000, 1.000000000000000000, 1.000000000000000222, 1.000000000000000000, 0.9999999999999998890, 1.000000000000000222, 1.000000000000000000, 1.000000000000000000, 1.000000000000000222, 1.000000000000000000, 1.000000000000000000, 1.000000000000000222, 1.000000000000000000, 1.000000000000000000, 1.000000000000000000, 1.000000000000000000, 1.000000000000000000, 1.000000000000000222, 1.000000000000000222, 1.000000000000000000, 1.000000000000000000, 1.000000000000000222, 1.000000000000000222, 1.000000000000000222, 1.000000000000000000, 1.000000000000000222, 1.000000000000000222, 1.000000000000000000, 1.000000000000000000, 1.000000000000000222, 1.000000000000000000, 1.000000000000000000, 1.000000000000000222, 1.000000000000000000, 1.000000000000000000, 1.000000000000000222, 1.000000000000000222, 1.000000000000000000, 1.000000000000000000, 1.000000000000000222, 1.000000000000000000, 1.000000000000000222, 1.000000000000000222, 1.000000000000000000, 1.000000000000000000, 1.000000000000000222, 1.000000000000000222, 1.000000000000000222, 1.000000000000000000, 1.000000000000000000, 1.000000000000000222, 1.000000000000000000, 0.9999999999999998890, 1.000000000000000222, 1.000000000000000000, 1.000000000000000000, 1.000000000000000222, 1.000000000000000000, 1.000000000000000000, 1.000000000000000222, 1.000000000000000000, 1.000000000000000000, 1.000000000000000000, 1.000000000000000000, 1.000000000000000000, 1.000000000000000222, 1.000000000000000222, 1.000000000000000000, 1.000000000000000000, 1.000000000000000222, 1.000000000000000222, 1.000000000000000222, 1.000000000000000000, 1.000000000000000000, 1.000000000000000222, 1.000000000000000000, 1.000000000000000000, 1.000000000000000222, 1.000000000000000000, 1.000000000000000000, 1.000000000000000222, 1.000000000000000000, 0.9999999999999996669, 0.9999999999999996669, 1.000000000000000000, 1.000000000000000222, 1.000000000000000000, 1.000000000000000000, 1.000000000000000000, 1.000000000000000000, 1.000000000000000000, 1.000000000000000000, 1.000000000000000000, 1.000000000000000000),
 ( 0.3333333333333333703, 0.3333333333333333703, 0.3333333333333333703, 0.3333333333333334259, 0.3333333333333334259, 0.3333333333333334259, 0.3333333333333333703, 0.3333333333333333148, 0.3333333333333333703, 0.3333333333333333703, 0.3333333333333333148, 0.3333333333333333703, 0.3333333333333333703, 0.3333333333333334814, 0.3333333333333333703, 0.3333333333333333703, 0.3333333333333334259, 0.3333333333333333703, 0.3333333333333333148, 0.3333333333333333703, 0.3333333333333333703, 0.3333333333333333703, 0.3333333333333333703, 0.3333333333333333703, 0.3333333333333333148, 0.3333333333333334259, 0.3333333333333333703, 0.3333333333333333703, 0.3333333333333333703, 0.3333333333333334259, 0.3333333333333333703, 0.3333333333333333703, 0.3333333333333333703, 0.3333333333333333703, 0.3333333333333333148, 0.3333333333333333703, 0.3333333333333334259, 0.3333333333333333703, 0.3333333333333333703, 0.3333333333333333703, 0.3333333333333333703, 0.3333333333333333703, 0.3333333333333333703, 0.3333333333333333703, 0.3333333333333333703, 0.3333333333333333148, 0.3333333333333333703, 0.3333333333333333703, 0.3333333333333333703, 0.3333333333333334259, 0.3333333333333333703, 0.3333333333333333703, 0.3333333333333333703, 0.3333333333333333703, 0.3333333333333333703, 0.3333333333333334259, 0.3333333333333333703, 0.3333333333333333703, 0.3333333333333333703, 0.3333333333333333703, 0.3333333333333334259, 0.3333333333333333703, 0.3333333333333333703, 0.3333333333333333703, 0.3333333333333333703, 0.3333333333333333703, 0.3333333333333333703, 0.3333333333333333148, 0.3333333333333333148, 0.3333333333333333148, 0.3333333333333333703, 0.3333333333333333703, 0.3333333333333333148, 0.3333333333333334259, 0.3333333333333333703, 0.3333333333333333703, 0.3333333333333333703, 0.3333333333333333703, 0.3333333333333333703, 0.3333333333333333703, 0.3333333333333333703, 0.3333333333333333703, 0.3333333333333333703, 0.3333333333333334259, 0.3333333333333334259, 0.3333333333333333703, 0.3333333333333333703, 0.3333333333333333703, 0.3333333333333333703, 0.3333333333333333703, 0.3333333333333333703, 0.3333333333333333703, 0.3333333333333333148, 0.3333333333333333148, 0.3333333333333333703, 0.3333333333333333703, 0.3333333333333333148, 0.3333333333333334259, 0.3333333333333333703, 0.3333333333333333703, 0.3333333333333333703, 0.3333333333333333703, 0.3333333333333333703, 0.3333333333333333703, 0.3333333333333333703, 0.3333333333333333703, 0.3333333333333333703, 0.3333333333333333703, 0.3333333333333333703, 0.3333333333333333148, 0.3333333333333333703, 0.3333333333333333703, 0.3333333333333333703, 0.3333333333333333703, 0.3333333333333333148, 0.3333333333333333703, 0.3333333333333333703, 0.3333333333333333148, 0.3333333333333333703, 0.3333333333333333703, 0.3333333333333333148, 0.3333333333333334259, 0.3333333333333333703, 0.3333333333333333703, 0.3333333333333333703, 0.3333333333333333703, 0.3333333333333333703, 0.3333333333333334259, 0.3333333333333333703, 0.3333333333333333703, 0.3333333333333334259, 0.3333333333333334259, 0.3333333333333334259, 0.3333333333333333703, 0.3333333333333333703, 0.3333333333333333703, 0.3333333333333333703, 0.3333333333333333703, 0.3333333333333333703, 0.3333333333333333703, 0.3333333333333333703, 0.3333333333333333703, 0.3333333333333334259, 0.3333333333333333703, 0.3333333333333333148, 0.3333333333333334259, 0.3333333333333333703, 0.3333333333333333703, 0.3333333333333333703, 0.3333333333333333703, 0.3333333333333333703, 0.3333333333333334259, 0.3333333333333333703, 0.3333333333333333703, 0.3333333333333333703, 0.3333333333333334259, 0.3333333333333333703, 0.3333333333333333703, 0.3333333333333333703, 0.3333333333333333703, 0.3333333333333333703, 0.3333333333333333703, 0.3333333333333333148, 0.3333333333333334259, 0.3333333333333333703, 0.3333333333333333148, 0.3333333333333333703, 0.3333333333333333703, 0.3333333333333333703, 0.3333333333333334259, 0.3333333333333333703, 0.3333333333333333703, 0.3333333333333333703, 0.3333333333333333703, 0.3333333333333333703, 0.3333333333333334259, 0.3333333333333333703, 0.3333333333333333703, 0.3333333333333333703, 0.3333333333333333703, 0.3333333333333334259, 0.3333333333333333703, 0.3333333333333333703, 0.3333333333333333703, 0.3333333333333333703, 0.3333333333333333703, 0.3333333333333333703, 0.3333333333333333148, 0.3333333333333333703, 0.3333333333333333703, 0.3333333333333333703, 0.3333333333333333703, 0.3333333333333333148, 0.3333333333333333703, 0.3333333333333333703, 0.3333333333333333703, 0.3333333333333333703, 0.3333333333333333703),
 ( 0.3333333333333333703, 0.3333333333333333703, 0.3333333333333333703, 0.3333333333333334259, 0.3333333333333334259, 0.3333333333333334259, 0.3333333333333333703, 0.3333333333333333148, 0.3333333333333333703, 0.3333333333333333703, 0.3333333333333333148, 0.3333333333333333703, 0.3333333333333333703, 0.3333333333333334814, 0.3333333333333333703, 0.3333333333333333703, 0.3333333333333334259, 0.3333333333333333703, 0.3333333333333333148, 0.3333333333333333703, 0.3333333333333333703, 0.3333333333333333703, 0.3333333333333333703, 0.3333333333333333703, 0.3333333333333333148, 0.3333333333333334259, 0.3333333333333333703, 0.3333333333333333703, 0.3333333333333333703, 0.3333333333333334259, 0.3333333333333333703, 0.3333333333333333703, 0.3333333333333333703, 0.3333333333333333703, 0.3333333333333333148, 0.3333333333333333703, 0.3333333333333334259, 0.3333333333333333703, 0.3333333333333333703, 0.3333333333333333703, 0.3333333333333333703, 0.3333333333333333703, 0.3333333333333333703, 0.3333333333333333703, 0.3333333333333333703, 0.3333333333333333148, 0.3333333333333333703, 0.3333333333333333703, 0.3333333333333333703, 0.3333333333333334259, 0.3333333333333333703, 0.3333333333333333703, 0.3333333333333333703, 0.3333333333333333703, 0.3333333333333333703, 0.3333333333333334259, 0.3333333333333333703, 0.3333333333333333703, 0.3333333333333333703, 0.3333333333333333703, 0.3333333333333334259, 0.3333333333333333703, 0.3333333333333333703, 0.3333333333333333703, 0.3333333333333333703, 0.3333333333333333703, 0.3333333333333333703, 0.3333333333333333148, 0.3333333333333333148, 0.3333333333333333148, 0.3333333333333333703, 0.3333333333333333703, 0.3333333333333333148, 0.3333333333333334259, 0.3333333333333333703, 0.3333333333333333703, 0.3333333333333333703, 0.3333333333333333703, 0.3333333333333333703, 0.3333333333333333703, 0.3333333333333333703, 0.3333333333333333703, 0.3333333333333333703, 0.3333333333333334259, 0.3333333333333334259, 0.3333333333333333703, 0.3333333333333333703, 0.3333333333333333703, 0.3333333333333333703, 0.3333333333333333703, 0.3333333333333333703, 0.3333333333333333703, 0.3333333333333333148, 0.3333333333333333148, 0.3333333333333333703, 0.3333333333333333703, 0.3333333333333333148, 0.3333333333333334259, 0.3333333333333333703, 0.3333333333333333703, 0.3333333333333333703, 0.3333333333333333703, 0.3333333333333333703, 0.3333333333333333703, 0.3333333333333333703, 0.3333333333333333703, 0.3333333333333333703, 0.3333333333333333703, 0.3333333333333333703, 0.3333333333333333148, 0.3333333333333333703, 0.3333333333333333703, 0.3333333333333333703, 0.3333333333333333703, 0.3333333333333333148, 0.3333333333333333703, 0.3333333333333333703, 0.3333333333333333148, 0.3333333333333333703, 0.3333333333333333703, 0.3333333333333333148, 0.3333333333333334259, 0.3333333333333333703, 0.3333333333333333703, 0.3333333333333333703, 0.3333333333333333703, 0.3333333333333333703, 0.3333333333333334259, 0.3333333333333333703, 0.3333333333333333703, 0.3333333333333334259, 0.3333333333333334259, 0.3333333333333334259, 0.3333333333333333703, 0.3333333333333333703, 0.3333333333333333703, 0.3333333333333333703, 0.3333333333333333703, 0.3333333333333333703, 0.3333333333333333703, 0.3333333333333333703, 0.3333333333333333703, 0.3333333333333334259, 0.3333333333333333703, 0.3333333333333333148, 0.3333333333333334259, 0.3333333333333333703, 0.3333333333333333703, 0.3333333333333333703, 0.3333333333333333703, 0.3333333333333333703, 0.3333333333333334259, 0.3333333333333333703, 0.3333333333333333703, 0.3333333333333333703, 0.3333333333333334259, 0.3333333333333333703, 0.3333333333333333703, 0.3333333333333333703, 0.3333333333333333703, 0.3333333333333333703, 0.3333333333333333703, 0.3333333333333333148, 0.3333333333333334259, 0.3333333333333333703, 0.3333333333333333148, 0.3333333333333333703, 0.3333333333333333703, 0.3333333333333333703, 0.3333333333333334259, 0.3333333333333333703, 0.3333333333333333703, 0.3333333333333333703, 0.3333333333333333703, 0.3333333333333333703, 0.3333333333333334259, 0.3333333333333333703, 0.3333333333333333703, 0.3333333333333333703, 0.3333333333333333703, 0.3333333333333334259, 0.3333333333333333703, 0.3333333333333333703, 0.3333333333333333703, 0.3333333333333333703, 0.3333333333333333703, 0.3333333333333333703, 0.3333333333333333148, 0.3333333333333333703, 0.3333333333333333703, 0.3333333333333333703, 0.3333333333333333703, 0.3333333333333333148, 0.3333333333333333703, 0.3333333333333333703, 0.3333333333333333703, 0.3333333333333333703, 0.3333333333333333703),
 ( 1.000000000000000000, 1.000000000000000000, 1.000000000000000000, 1.000000000000000000, 1.000000000000000000, 1.000000000000000000, 0.9999999999999998890, 0.9999999999999997780, 1.000000000000000000, 1.000000000000000000, 1.000000000000000000, 1.000000000000000000, 1.000000000000000000, 1.000000000000000000, 0.9999999999999998890, 1.000000000000000000, 1.000000000000000222, 1.000000000000000000, 1.000000000000000000, 1.000000000000000000, 1.000000000000000000, 1.000000000000000000, 0.9999999999999998890, 0.9999999999999997780, 1.000000000000000000, 1.000000000000000222, 1.000000000000000000, 1.000000000000000000, 1.000000000000000000, 1.000000000000000000, 0.9999999999999998890, 0.9999999999999997780, 1.000000000000000000, 0.9999999999999998890, 0.9999999999999997780, 1.000000000000000000, 1.000000000000000222, 1.000000000000000222, 1.000000000000000000, 1.000000000000000000, 1.000000000000000222, 1.000000000000000000, 0.9999999999999997780, 1.000000000000000000, 1.000000000000000000, 1.000000000000000000, 1.000000000000000000, 1.000000000000000000, 1.000000000000000000, 1.000000000000000222, 1.000000000000000222, 1.000000000000000000, 1.000000000000000000, 1.000000000000000222, 1.000000000000000222, 1.000000000000000222, 1.000000000000000000, 1.000000000000000000, 1.000000000000000222, 1.000000000000000000, 1.000000000000000000, 1.000000000000000222, 1.000000000000000000, 1.000000000000000000, 1.000000000000000222, 1.000000000000000000, 1.000000000000000000, 0.9999999999999997780, 0.9999999999999998890, 1.000000000000000000, 1.000000000000000000, 1.000000000000000000, 1.000000000000000000, 1.000000000000000222, 1.000000000000000222, 1.000000000000000000, 1.000000000000000000, 1.000000000000000222, 1.000000000000000222, 1.000000000000000222, 1.000000000000000000, 1.000000000000000000, 1.000000000000000222, 1.000000000000000000, 1.000000000000000000, 1.000000000000000222, 1.000000000000000000, 1.000000000000000000, 1.000000000000000222, 1.000000000000000000, 1.000000000000000000, 0.9999999999999997780, 0.9999999999999998890, 1.000000000000000000, 1.000000000000000000, 1.000000000000000000, 1.000000000000000000, 1.000000000000000222, 1.000000000000000222, 1.000000000000000000, 1.000000000000000000, 1.000000000000000222, 1.000000000000000222, 1.000000000000000222, 1.000000000000000000, 1.000000000000000000, 1.000000000000000222, 1.000000000000000000, 0.9999999999999998890, 1.000000000000000222, 1.000000000000000000, 1.000000000000000000, 1.000000000000000222, 1.000000000000000000, 1.000000000000000000, 1.000000000000000222, 1.000000000000000000, 1.000000000000000000, 1.000000000000000000, 1.000000000000000000, 1.000000000000000000, 1.000000000000000222, 1.000000000000000222, 1.000000000000000000, 1.000000000000000000, 1.000000000000000222, 1.000000000000000222, 1.000000000000000222, 1.000000000000000000, 1.000000000000000222, 1.000000000000000222, 1.000000000000000000, 1.000000000000000000, 1.000000000000000222, 1.000000000000000000, 1.000000000000000000, 1.000000000000000222, 1.000000000000000000, 1.000000000000000000, 1.000000000000000222, 1.000000000000000222, 1.000000000000000000, 1.000000000000000000, 1.000000000000000222, 1.000000000000000000, 1.000000000000000222, 1.000000000000000222, 1.000000000000000000, 1.000000000000000000, 1.000000000000000222, 1.000000000000000222, 1.000000000000000222, 1.000000000000000000, 1.000000000000000000, 1.000000000000000222, 1.000000000000000000, 0.9999999999999998890, 1.000000000000000222, 1.000000000000000000, 1.000000000000000000, 1.000000000000000222, 1.000000000000000000, 1.000000000000000000, 1.000000000000000222, 1.000000000000000000, 1.000000000000000000, 1.000000000000000000, 1.000000000000000000, 1.000000000000000000, 1.000000000000000222, 1.000000000000000222, 1.000000000000000000, 1.000000000000000000, 1.000000000000000222, 1.000000000000000222, 1.000000000000000222, 1.000000000000000000, 1.000000000000000000, 1.000000000000000222, 1.000000000000000000, 1.000000000000000000, 1.000000000000000222, 1.000000000000000000, 1.000000000000000000, 1.000000000000000222, 1.000000000000000000, 0.9999999999999996669, 0.9999999999999996669, 1.000000000000000000, 1.000000000000000222, 1.000000000000000000, 1.000000000000000000, 1.000000000000000000, 1.000000000000000000, 1.000000000000000000, 1.000000000000000000, 1.000000000000000000, 1.000000000000000000),
 ( 0.3333333333333333703, 0.3333333333333333703, 0.3333333333333333703, 0.3333333333333334259, 0.3333333333333334259, 0.3333333333333334259, 0.3333333333333333703, 0.3333333333333333148, 0.3333333333333333703, 0.3333333333333333703, 0.3333333333333333148, 0.3333333333333333703, 0.3333333333333333703, 0.3333333333333334814, 0.3333333333333333703, 0.3333333333333333703, 0.3333333333333334259, 0.3333333333333333703, 0.3333333333333333148, 0.3333333333333333703, 0.3333333333333333703, 0.3333333333333333703, 0.3333333333333333703, 0.3333333333333333703, 0.3333333333333333148, 0.3333333333333334259, 0.3333333333333333703, 0.3333333333333333703, 0.3333333333333333703, 0.3333333333333334259, 0.3333333333333333703, 0.3333333333333333703, 0.3333333333333333703, 0.3333333333333333703, 0.3333333333333333148, 0.3333333333333333703, 0.3333333333333334259, 0.3333333333333333703, 0.3333333333333333703, 0.3333333333333333703, 0.3333333333333333703, 0.3333333333333333703, 0.3333333333333333703, 0.3333333333333333703, 0.3333333333333333703, 0.3333333333333333148, 0.3333333333333333703, 0.3333333333333333703, 0.3333333333333333703, 0.3333333333333334259, 0.3333333333333333703, 0.3333333333333333703, 0.3333333333333333703, 0.3333333333333333703, 0.3333333333333333703, 0.3333333333333334259, 0.3333333333333333703, 0.3333333333333333703, 0.3333333333333333703, 0.3333333333333333703, 0.3333333333333334259, 0.3333333333333333703, 0.3333333333333333703, 0.3333333333333333703, 0.3333333333333333703, 0.3333333333333333703, 0.3333333333333333703, 0.3333333333333333148, 0.3333333333333333148, 0.3333333333333333148, 0.3333333333333333703, 0.3333333333333333703, 0.3333333333333333148, 0.3333333333333334259, 0.3333333333333333703, 0.3333333333333333703, 0.3333333333333333703, 0.3333333333333333703, 0.3333333333333333703, 0.3333333333333333703, 0.3333333333333333703, 0.3333333333333333703, 0.3333333333333333703, 0.3333333333333334259, 0.3333333333333334259, 0.3333333333333333703, 0.3333333333333333703, 0.3333333333333333703, 0.3333333333333333703, 0.3333333333333333703, 0.3333333333333333703, 0.3333333333333333703, 0.3333333333333333148, 0.3333333333333333148, 0.3333333333333333703, 0.3333333333333333703, 0.3333333333333333148, 0.3333333333333334259, 0.3333333333333333703, 0.3333333333333333703, 0.3333333333333333703, 0.3333333333333333703, 0.3333333333333333703, 0.3333333333333333703, 0.3333333333333333703, 0.3333333333333333703, 0.3333333333333333703, 0.3333333333333333703, 0.3333333333333333703, 0.3333333333333333148, 0.3333333333333333703, 0.3333333333333333703, 0.3333333333333333703, 0.3333333333333333703, 0.3333333333333333148, 0.3333333333333333703, 0.3333333333333333703, 0.3333333333333333148, 0.3333333333333333703, 0.3333333333333333703, 0.3333333333333333148, 0.3333333333333334259, 0.3333333333333333703, 0.3333333333333333703, 0.3333333333333333703, 0.3333333333333333703, 0.3333333333333333703, 0.3333333333333334259, 0.3333333333333333703, 0.3333333333333333703, 0.3333333333333334259, 0.3333333333333334259, 0.3333333333333334259, 0.3333333333333333703, 0.3333333333333333703, 0.3333333333333333703, 0.3333333333333333703, 0.3333333333333333703, 0.3333333333333333703, 0.3333333333333333703, 0.3333333333333333703, 0.3333333333333333703, 0.3333333333333334259, 0.3333333333333333703, 0.3333333333333333148, 0.3333333333333334259, 0.3333333333333333703, 0.3333333333333333703, 0.3333333333333333703, 0.3333333333333333703, 0.3333333333333333703, 0.3333333333333334259, 0.3333333333333333703, 0.3333333333333333703, 0.3333333333333333703, 0.3333333333333334259, 0.3333333333333333703, 0.3333333333333333703, 0.3333333333333333703, 0.3333333333333333703, 0.3333333333333333703, 0.3333333333333333703, 0.3333333333333333148, 0.3333333333333334259, 0.3333333333333333703, 0.3333333333333333148, 0.3333333333333333703, 0.3333333333333333703, 0.3333333333333333703, 0.3333333333333334259, 0.3333333333333333703, 0.3333333333333333703, 0.3333333333333333703, 0.3333333333333333703, 0.3333333333333333703, 0.3333333333333334259, 0.3333333333333333703, 0.3333333333333333703, 0.3333333333333333703, 0.3333333333333333703, 0.3333333333333334259, 0.3333333333333333703, 0.3333333333333333703, 0.3333333333333333703, 0.3333333333333333703, 0.3333333333333333703, 0.3333333333333333703, 0.3333333333333333148, 0.3333333333333333703, 0.3333333333333333703, 0.3333333333333333703, 0.3333333333333333703, 0.3333333333333333148, 0.3333333333333333703, 0.3333333333333333703, 0.3333333333333333703, 0.3333333333333333703, 0.3333333333333333703),
 ( 0.3333333333333333703, 0.3333333333333333703, 0.3333333333333333703, 0.3333333333333334259, 0.3333333333333334259, 0.3333333333333334259, 0.3333333333333333703, 0.3333333333333333148, 0.3333333333333333703, 0.3333333333333333703, 0.3333333333333333148, 0.3333333333333333703, 0.3333333333333333703, 0.3333333333333334814, 0.3333333333333333703, 0.3333333333333333703, 0.3333333333333334259, 0.3333333333333333703, 0.3333333333333333148, 0.3333333333333333703, 0.3333333333333333703, 0.3333333333333333703, 0.3333333333333333703, 0.3333333333333333703, 0.3333333333333333148, 0.3333333333333334259, 0.3333333333333333703, 0.3333333333333333703, 0.3333333333333333703, 0.3333333333333334259, 0.3333333333333333703, 0.3333333333333333703, 0.3333333333333333703, 0.3333333333333333703, 0.3333333333333333148, 0.3333333333333333703, 0.3333333333333334259, 0.3333333333333333703, 0.3333333333333333703, 0.3333333333333333703, 0.3333333333333333703, 0.3333333333333333703, 0.3333333333333333703, 0.3333333333333333703, 0.3333333333333333703, 0.3333333333333333148, 0.3333333333333333703, 0.3333333333333333703, 0.3333333333333333703, 0.3333333333333334259, 0.3333333333333333703, 0.3333333333333333703, 0.3333333333333333703, 0.3333333333333333703, 0.3333333333333333703, 0.3333333333333334259, 0.3333333333333333703, 0.3333333333333333703, 0.3333333333333333703, 0.3333333333333333703, 0.3333333333333334259, 0.3333333333333333703, 0.3333333333333333703, 0.3333333333333333703, 0.3333333333333333703, 0.3333333333333333703, 0.3333333333333333703, 0.3333333333333333148, 0.3333333333333333148, 0.3333333333333333148, 0.3333333333333333703, 0.3333333333333333703, 0.3333333333333333148, 0.3333333333333334259, 0.3333333333333333703, 0.3333333333333333703, 0.3333333333333333703, 0.3333333333333333703, 0.3333333333333333703, 0.3333333333333333703, 0.3333333333333333703, 0.3333333333333333703, 0.3333333333333333703, 0.3333333333333334259, 0.3333333333333334259, 0.3333333333333333703, 0.3333333333333333703, 0.3333333333333333703, 0.3333333333333333703, 0.3333333333333333703, 0.3333333333333333703, 0.3333333333333333703, 0.3333333333333333148, 0.3333333333333333148, 0.3333333333333333703, 0.3333333333333333703, 0.3333333333333333148, 0.3333333333333334259, 0.3333333333333333703, 0.3333333333333333703, 0.3333333333333333703, 0.3333333333333333703, 0.3333333333333333703, 0.3333333333333333703, 0.3333333333333333703, 0.3333333333333333703, 0.3333333333333333703, 0.3333333333333333703, 0.3333333333333333703, 0.3333333333333333148, 0.3333333333333333703, 0.3333333333333333703, 0.3333333333333333703, 0.3333333333333333703, 0.3333333333333333148, 0.3333333333333333703, 0.3333333333333333703, 0.3333333333333333148, 0.3333333333333333703, 0.3333333333333333703, 0.3333333333333333148, 0.3333333333333334259, 0.3333333333333333703, 0.3333333333333333703, 0.3333333333333333703, 0.3333333333333333703, 0.3333333333333333703, 0.3333333333333334259, 0.3333333333333333703, 0.3333333333333333703, 0.3333333333333334259, 0.3333333333333334259, 0.3333333333333334259, 0.3333333333333333703, 0.3333333333333333703, 0.3333333333333333703, 0.3333333333333333703, 0.3333333333333333703, 0.3333333333333333703, 0.3333333333333333703, 0.3333333333333333703, 0.3333333333333333703, 0.3333333333333334259, 0.3333333333333333703, 0.3333333333333333148, 0.3333333333333334259, 0.3333333333333333703, 0.3333333333333333703, 0.3333333333333333703, 0.3333333333333333703, 0.3333333333333333703, 0.3333333333333334259, 0.3333333333333333703, 0.3333333333333333703, 0.3333333333333333703, 0.3333333333333334259, 0.3333333333333333703, 0.3333333333333333703, 0.3333333333333333703, 0.3333333333333333703, 0.3333333333333333703, 0.3333333333333333703, 0.3333333333333333148, 0.3333333333333334259, 0.3333333333333333703, 0.3333333333333333148, 0.3333333333333333703, 0.3333333333333333703, 0.3333333333333333703, 0.3333333333333334259, 0.3333333333333333703, 0.3333333333333333703, 0.3333333333333333703, 0.3333333333333333703, 0.3333333333333333703, 0.3333333333333334259, 0.3333333333333333703, 0.3333333333333333703, 0.3333333333333333703, 0.3333333333333333703, 0.3333333333333334259, 0.3333333333333333703, 0.3333333333333333703, 0.3333333333333333703, 0.3333333333333333703, 0.3333333333333333703, 0.3333333333333333703, 0.3333333333333333148, 0.3333333333333333703, 0.3333333333333333703, 0.3333333333333333703, 0.3333333333333333703, 0.3333333333333333148, 0.3333333333333333703, 0.3333333333333333703, 0.3333333333333333703, 0.3333333333333333703, 0.3333333333333333703),
 ( 1.000000000000000000, 1.000000000000000000, 1.000000000000000000, 1.000000000000000000, 1.000000000000000000, 1.000000000000000000, 0.9999999999999998890, 0.9999999999999997780, 1.000000000000000000, 1.000000000000000000, 1.000000000000000000, 1.000000000000000000, 1.000000000000000000, 1.000000000000000000, 0.9999999999999998890, 1.000000000000000000, 1.000000000000000222, 1.000000000000000000, 1.000000000000000000, 1.000000000000000000, 1.000000000000000000, 1.000000000000000000, 0.9999999999999998890, 0.9999999999999997780, 1.000000000000000000, 1.000000000000000222, 1.000000000000000000, 1.000000000000000000, 1.000000000000000000, 1.000000000000000000, 0.9999999999999998890, 0.9999999999999997780, 1.000000000000000000, 0.9999999999999998890, 0.9999999999999997780, 1.000000000000000000, 1.000000000000000222, 1.000000000000000222, 1.000000000000000000, 1.000000000000000000, 1.000000000000000222, 1.000000000000000000, 0.9999999999999997780, 1.000000000000000000, 1.000000000000000000, 1.000000000000000000, 1.000000000000000000, 1.000000000000000000, 1.000000000000000000, 1.000000000000000222, 1.000000000000000222, 1.000000000000000000, 1.000000000000000000, 1.000000000000000222, 1.000000000000000222, 1.000000000000000222, 1.000000000000000000, 1.000000000000000000, 1.000000000000000222, 1.000000000000000000, 1.000000000000000000, 1.000000000000000222, 1.000000000000000000, 1.000000000000000000, 1.000000000000000222, 1.000000000000000000, 1.000000000000000000, 0.9999999999999997780, 0.9999999999999998890, 1.000000000000000000, 1.000000000000000000, 1.000000000000000000, 1.000000000000000000, 1.000000000000000222, 1.000000000000000222, 1.000000000000000000, 1.000000000000000000, 1.000000000000000222, 1.000000000000000222, 1.000000000000000222, 1.000000000000000000, 1.000000000000000000, 1.000000000000000222, 1.000000000000000000, 1.000000000000000000, 1.000000000000000222, 1.000000000000000000, 1.000000000000000000, 1.000000000000000222, 1.000000000000000000, 1.000000000000000000, 0.9999999999999997780, 0.9999999999999998890, 1.000000000000000000, 1.000000000000000000, 1.000000000000000000, 1.000000000000000000, 1.000000000000000222, 1.000000000000000222, 1.000000000000000000, 1.000000000000000000, 1.000000000000000222, 1.000000000000000222, 1.000000000000000222, 1.000000000000000000, 1.000000000000000000, 1.000000000000000222, 1.000000000000000000, 0.9999999999999998890, 1.000000000000000222, 1.000000000000000000, 1.000000000000000000, 1.000000000000000222, 1.000000000000000000, 1.000000000000000000, 1.000000000000000222, 1.000000000000000000, 1.000000000000000000, 1.000000000000000000, 1.000000000000000000, 1.000000000000000000, 1.000000000000000222, 1.000000000000000222, 1.000000000000000000, 1.000000000000000000, 1.000000000000000222, 1.000000000000000222, 1.000000000000000222, 1.000000000000000000, 1.000000000000000222, 1.000000000000000222, 1.000000000000000000, 1.000000000000000000, 1.000000000000000222, 1.000000000000000000, 1.000000000000000000, 1.000000000000000222, 1.000000000000000000, 1.000000000000000000, 1.000000000000000222, 1.000000000000000222, 1.000000000000000000, 1.000000000000000000, 1.000000000000000222, 1.000000000000000000, 1.000000000000000222, 1.000000000000000222, 1.000000000000000000, 1.000000000000000000, 1.000000000000000222, 1.000000000000000222, 1.000000000000000222, 1.000000000000000000, 1.000000000000000000, 1.000000000000000222, 1.000000000000000000, 0.9999999999999998890, 1.000000000000000222, 1.000000000000000000, 1.000000000000000000, 1.000000000000000222, 1.000000000000000000, 1.000000000000000000, 1.000000000000000222, 1.000000000000000000, 1.000000000000000000, 1.000000000000000000, 1.000000000000000000, 1.000000000000000000, 1.000000000000000222, 1.000000000000000222, 1.000000000000000000, 1.000000000000000000, 1.000000000000000222, 1.000000000000000222, 1.000000000000000222, 1.000000000000000000, 1.000000000000000000, 1.000000000000000222, 1.000000000000000000, 1.000000000000000000, 1.000000000000000222, 1.000000000000000000, 1.000000000000000000, 1.000000000000000222, 1.000000000000000000, 0.9999999999999996669, 0.9999999999999996669, 1.000000000000000000, 1.000000000000000222, 1.000000000000000000, 1.000000000000000000, 1.000000000000000000, 1.000000000000000000, 1.000000000000000000, 1.000000000000000000, 1.000000000000000000, 1.000000000000000000) ) ) 
 REPRESENTATION_ITEM ( '' )  SURFACE ( )  );
#29141 = CARTESIAN_POINT ( 'NONE',  ( -6.442348895218290093E-14, 63.84746620154572838, 4.408874939877717575E-29 ) ) ;
#29142 = CARTESIAN_POINT ( 'NONE',  ( -50.47475848037564816, 15.37778258171979218, 4.692728031515248865 ) ) ;
#29143 = CARTESIAN_POINT ( 'NONE',  ( -46.81070079724250377, 25.76746909427398435, 1.215830024444411572 ) ) ;
#29144 = DIRECTION ( 'NONE',  ( -1.000000000000000000, 0.000000000000000000, 0.000000000000000000 ) ) ;
#29145 = CARTESIAN_POINT ( 'NONE',  ( -42.33919149967392315, 22.05006338260229271, 1.842566675324087022 ) ) ;
#29146 = DIRECTION ( 'NONE',  ( 5.188838149069472160E-16, -1.699382548006136559E-16, -1.000000000000000000 ) ) ;
#29147 = CARTESIAN_POINT ( 'NONE',  ( -4.667303623731948292, 118.0255731622509643, 0.5720496121413468638 ) ) ;
#29148 = CARTESIAN_POINT ( 'NONE',  ( -5.675123159882439872, 78.90545016724971106, -5.052246757648558351 ) ) ;
#29149 = ORIENTED_EDGE ( 'NONE', *, *, #31878, .F. ) ;
#29150 = VERTEX_POINT ( 'NONE', #4567 ) ;
#29151 = FACE_OUTER_BOUND ( 'NONE', #20152, .T. ) ;
#29152 = AXIS2_PLACEMENT_3D ( 'NONE', #9669, #41433, #12452 ) ;
#29153 = CARTESIAN_POINT ( 'NONE',  ( 8.403226289273074912, 119.7337369526196369, -1.096787843810197893 ) ) ;
#29154 = CARTESIAN_POINT ( 'NONE',  ( -1.365700293149888278, 106.2535611835979239, -5.166841330979377034 ) ) ;
#29155 = CARTESIAN_POINT ( 'NONE',  ( 4.704201265585868263, 117.9644370305355210, 0.8021818384322239037 ) ) ;
#29156 = AXIS2_PLACEMENT_3D ( 'NONE', #17265, #36032, #32833 ) ;
#29157 = CARTESIAN_POINT ( 'NONE',  ( -5.309060684617390516E-14, 83.56599999999998829, 0.000000000000000000 ) ) ;
#29158 = CARTESIAN_POINT ( 'NONE',  ( -15.33786013020733563, 149.0334586719817764, -1.566117276479743303 ) ) ;
#29159 = CARTESIAN_POINT ( 'NONE',  ( -3.908125678941627879, 115.7034627620156044, -1.591772151217179188 ) ) ;
#29160 = CARTESIAN_POINT ( 'NONE',  ( 16.87828382557106721, 17.14499999999999957, 5.016499999999999737 ) ) ;
#29161 = CARTESIAN_POINT ( 'NONE',  ( -47.85244527695896011, 19.39403540832957518, 5.219971639306693056 ) ) ;
#29162 = CARTESIAN_POINT ( 'NONE',  ( 5.086085965935678743, 114.3657942991566472, -1.756424186875608751 ) ) ;
#29163 = CARTESIAN_POINT ( 'NONE',  ( -8.769168840778196028, 122.1986804192922875, -1.175795117382457455 ) ) ;
#29164 = LINE ( 'NONE', #39615, #35339 ) ;
#29165 = FACE_OUTER_BOUND ( 'NONE', #8428, .T. ) ;
#29166 = CARTESIAN_POINT ( 'NONE',  ( -0.6420072254102160425, 156.3034662015458593, 0.02290919489485064575 ) ) ;
#29167 = EDGE_CURVE ( 'NONE', #17268, #5804, #40348, .T. ) ;
#29168 = CARTESIAN_POINT ( 'NONE',  ( -3.974385726840726107, -7.478117039488521023, -2.359557994316856533 ) ) ;
#29170 = ORIENTED_EDGE ( 'NONE', *, *, #10346, .T. ) ;
#29169 = CARTESIAN_POINT ( 'NONE',  ( 11.45183593531609745, 118.8698716516685465, 0.7694570404682200548 ) ) ;
#29171 = DIRECTION ( 'NONE',  ( 5.188838149069472160E-16, -1.699382548006136559E-16, -1.000000000000000000 ) ) ;
#29172 = CARTESIAN_POINT ( 'NONE',  ( 3.340243159461592448, -15.49156354636899202, 3.813188716183662397 ) ) ;
#29173 = CARTESIAN_POINT ( 'NONE',  ( -1.037157837436492702, 157.7941190989783991, 1.604419329240822201 ) ) ;
#29174 = CARTESIAN_POINT ( 'NONE',  ( 0.9749890475506259868, 2.950361319068162569, -0.03356295239053608964 ) ) ;
#29175 = CARTESIAN_POINT ( 'NONE',  ( -23.12711913739495984, 149.5941399179437781, -0.9155080916133789826 ) ) ;
#29176 = CARTESIAN_POINT ( 'NONE',  ( -0.9350042896817728488, 3.318609271805546435, -0.2773724203853295545 ) ) ;
#29177 = ORIENTED_EDGE ( 'NONE', *, *, #35448, .F. ) ;
#29178 = EDGE_CURVE ( 'NONE', #21156, #25364, #35511, .T. ) ;
#29179 = CARTESIAN_POINT ( 'NONE',  ( -41.98003980773050614, 22.15641273310255954, 0.9734550245784977518 ) ) ;
#29180 = CARTESIAN_POINT ( 'NONE',  ( 4.970930975556632880, 121.2162878128435892, 0.3527489803516246081 ) ) ;
#29181 = APPLICATION_PROTOCOL_DEFINITION ( 'draft international standard', 'automotive_design', 1998, #1237 ) ;
#29182 = CARTESIAN_POINT ( 'NONE',  ( -10.46017523140589134, 124.8149993102252182, 0.6249645713522344881 ) ) ;
#29183 = CARTESIAN_POINT ( 'NONE',  ( 4.087908758852305091, -13.37781719547838399, 3.422002167429263331 ) ) ;
#29184 = CARTESIAN_POINT ( 'NONE',  ( 6.603469437764709404, 120.5225452898634728, -0.8609044167644230861 ) ) ;
#29185 = CARTESIAN_POINT ( 'NONE',  ( 0.03245814172805068509, 158.1186941186938952, -1.624338139048501217 ) ) ;
#29186 = CARTESIAN_POINT ( 'NONE',  ( -10.75478607932181241, 82.07015292912137738, -1.523999999999999355 ) ) ;
#29187 = ADVANCED_FACE ( 'NONE', ( #7754 ), #27989, .T. ) ;
#29188 = CARTESIAN_POINT ( 'NONE',  ( 2.460727335429193197, -15.06314154744310585, 4.845259171755021299 ) ) ;
#29189 = CARTESIAN_POINT ( 'NONE',  ( -0.01249116623180959208, 38.87185441664305330, -1.227828225846576471 ) ) ;
#29190 = CARTESIAN_POINT ( 'NONE',  ( 10.40586874195270362, 126.0814211662656419, -0.04952998093763438803 ) ) ;
#29191 = ORIENTED_EDGE ( 'NONE', *, *, #24135, .T. ) ;
#29192 = CARTESIAN_POINT ( 'NONE',  ( 0.1909974646900941819, 105.7854974534635346, 5.338829247572753900 ) ) ;
#29193 = AXIS2_PLACEMENT_3D ( 'NONE', #28695, #18046, #11447 ) ;
#29194 = CIRCLE ( 'NONE', #12862, 0.2539999999999997260 ) ;
#29195 = CARTESIAN_POINT ( 'NONE',  ( -15.23999999999999311, 71.11999999999999034, 5.714999999999999858 ) ) ;
#29196 = CARTESIAN_POINT ( 'NONE',  ( 4.878702690786834495, 117.7581303304119729, -0.7584199409633860522 ) ) ;
#29197 = ADVANCED_FACE ( 'NONE', ( #10719 ), #36720, .T. ) ;
#29198 = FACE_OUTER_BOUND ( 'NONE', #36378, .T. ) ;
#29199 = CARTESIAN_POINT ( 'NONE',  ( 23.35271726849051177, 148.8653451956335516, 0.3123667622787954512 ) ) ;
#29200 = FACE_OUTER_BOUND ( 'NONE', #19481, .T. ) ;
#29201 = DIRECTION ( 'NONE',  ( -0.9998004120163608288, 0.000000000000000000, -0.01997839162482749342 ) ) ;
#29202 = CARTESIAN_POINT ( 'NONE',  ( -0.8472427164685307766, -8.777537934218566207, -4.544909406875613733 ) ) ;
#29203 = CARTESIAN_POINT ( 'NONE',  ( 1.104298428969494816, 36.37359162847545235, -0.6925126829677044071 ) ) ;
#29204 = CARTESIAN_POINT ( 'NONE',  ( 21.07518769967733974, 148.4376209648218321, 2.358402543220756264 ) ) ;
#29205 = EDGE_CURVE ( 'NONE', #21592, #32447, #33743, .T. ) ;
#29206 = CARTESIAN_POINT ( 'NONE',  ( 0.4006815055314144058, 20.64345356492705719, 4.603752038498275745 ) ) ;
#29207 = CARTESIAN_POINT ( 'NONE',  ( -0.9165671635830696662, -12.81903285835614525, -8.372742598224451882 ) ) ;
#29208 = CARTESIAN_POINT ( 'NONE',  ( 8.740654271741430392, 118.0242495335989759, -0.4400757740126230444 ) ) ;
#29209 = CARTESIAN_POINT ( 'NONE',  ( -0.7595712053401582065, 120.2878791493615296, -0.5727019010319392978 ) ) ;
#29210 = CARTESIAN_POINT ( 'NONE',  ( -3.590474171207809651E-14, 56.51499999999999346, 0.000000000000000000 ) ) ;
#29211 = CARTESIAN_POINT ( 'NONE',  ( 1.351374093494389417, 106.2781030281888235, -5.112228481377823819 ) ) ;
#29212 = CARTESIAN_POINT ( 'NONE',  ( 3.260699289383273136, 104.6144662015456959, 3.570726652201047013 ) ) ;
#29213 = CARTESIAN_POINT ( 'NONE',  ( 4.636458409304901274, 17.36039413176390411, -0.09481320587925551324 ) ) ;
#29214 = CARTESIAN_POINT ( 'NONE',  ( -47.04837031381860157, 23.61299024743492581, -3.054033755318078303 ) ) ;
#29215 = CARTESIAN_POINT ( 'NONE',  ( 5.177913976931196594, 78.94499979771845233, -5.372100000000001430 ) ) ;
#29216 = CARTESIAN_POINT ( 'NONE',  ( 3.149239739297259533, -13.85570235734440203, 1.885463239856044027 ) ) ;
#29217 = ADVANCED_FACE ( 'NONE', ( #30312, #1366 ), #20927, .F. ) ;
#29218 = CARTESIAN_POINT ( 'NONE',  ( 0.1833862045735744073, 106.0860833631645193, -5.249533627824054527 ) ) ;
#29219 = CARTESIAN_POINT ( 'NONE',  ( -15.31827776641181060, 121.1074504348956964, 0.3839962087354599762 ) ) ;
#29220 = AXIS2_PLACEMENT_3D ( 'NONE', #14155, #7577, #33568 ) ;
#29221 = EDGE_LOOP ( 'NONE', ( #22060, #26285, #41279, #21472 ) ) ;
#29222 = CARTESIAN_POINT ( 'NONE',  ( 5.305748947172213015, 65.30181249999998272, 5.247078976224250013 ) ) ;
#29223 = AXIS2_PLACEMENT_3D ( 'NONE', #20201, #3629, #39401 ) ;
#29224 = ORIENTED_EDGE ( 'NONE', *, *, #41697, .F. ) ;
#29225 = CARTESIAN_POINT ( 'NONE',  ( 5.586884702347362897, 136.3644662015457527, 0.1116392523995368563 ) ) ;
#29226 = CARTESIAN_POINT ( 'NONE',  ( 4.032098335577404491, -15.72255795053374783, 4.298576634473052493 ) ) ;
#29227 = CARTESIAN_POINT ( 'NONE',  ( -8.870548826841627488, 119.8693228481767932, 1.115469810106635595 ) ) ;
#29228 = CARTESIAN_POINT ( 'NONE',  ( 6.863242444369292983, 118.1252062928739832, -0.7545491157480663791 ) ) ;
#29229 = EDGE_CURVE ( 'NONE', #22232, #40883, #13023, .T. ) ;
#29230 = CARTESIAN_POINT ( 'NONE',  ( 2.551540157903699146, -0.3564265548712530207, -3.854280124997286450 ) ) ;
#29231 = CARTESIAN_POINT ( 'NONE',  ( -58.80444036411011410, -0.2843080703047338176, -0.1310653756851450913 ) ) ;
#29232 = EDGE_LOOP ( 'NONE', ( #4200, #14517, #30867, #10984 ) ) ;
#29233 = CARTESIAN_POINT ( 'NONE',  ( 7.784012320830338005, 122.6313477005580665, 0.1555430910899518460 ) ) ;
#29234 = CARTESIAN_POINT ( 'NONE',  ( -14.60500000000000043, 71.11999999999999034, 5.016499999999999737 ) ) ;
#29235 = CARTESIAN_POINT ( 'NONE',  ( -11.13866856781930359, 123.6647009725989648, 1.091370626813936706 ) ) ;
#29236 = LINE ( 'NONE', #6672, #4145 ) ;
#29237 = CARTESIAN_POINT ( 'NONE',  ( 19.00012635448478449, 147.0452383304005082, -1.727400128179959804 ) ) ;
#29238 = CARTESIAN_POINT ( 'NONE',  ( -1.134298505455661354, 158.7113841514841681, -1.516915449716996767 ) ) ;
#29239 = CARTESIAN_POINT ( 'NONE',  ( -57.29531047346088712, 2.067549486662559222, -1.749273462387503031 ) ) ;
#29240 = EDGE_LOOP ( 'NONE', ( #39804, #40905, #25171, #27396 ) ) ;
#29241 = CARTESIAN_POINT ( 'NONE',  ( 4.493133734558046655, 118.1300458714410269, -0.5260358870164894007 ) ) ;
#29242 = CARTESIAN_POINT ( 'NONE',  ( 10.87798892776812210, 126.1616406593870607, -0.4640774846651394281 ) ) ;
#29243 = ORIENTED_EDGE ( 'NONE', *, *, #38940, .T. ) ;
#29244 = CARTESIAN_POINT ( 'NONE',  ( -9.109784082438133979, 121.7740273863187923, -1.385347505406782087 ) ) ;
#29245 = CARTESIAN_POINT ( 'NONE',  ( 2.557542807212066283, -15.51814986354871451, 4.851437248720891660 ) ) ;
#29246 = CARTESIAN_POINT ( 'NONE',  ( -13.85159022459153988, 59.63164443796365077, 5.016499999999999737 ) ) ;
#29247 = B_SPLINE_CURVE_WITH_KNOTS ( 'NONE', 3,
 ( #21658, #5512, #5728, #14439, #27449, #40464, #11254 ),
 .UNSPECIFIED., .F., .F.,
 ( 4, 3, 4 ),
 ( 0.000000000000000000, 6.533385608969465084E-05, 6.539385608967072667E-05 ),
 .UNSPECIFIED. ) ;
#29248 = CARTESIAN_POINT ( 'NONE',  ( 9.094996104468805243, 78.64197151092925253, -5.392902600000141433 ) ) ;
#29249 = TOROIDAL_SURFACE ( 'NONE', #17687, 5.080000000000005400, 0.5080000000000000071 ) ;
#29250 = CARTESIAN_POINT ( 'NONE',  ( -4.818488311985083428, 117.7362444359860945, 0.8718948188861159743 ) ) ;
#29251 = CARTESIAN_POINT ( 'NONE',  ( 0.5297590882381500998, 119.7690751942239729, 0.5117926329762008120 ) ) ;
#29252 = CARTESIAN_POINT ( 'NONE',  ( -46.60530155212504155, 26.17382724835477958, 1.269999999999990692 ) ) ;
#29253 = CARTESIAN_POINT ( 'NONE',  ( -3.685501180670149424, 30.72893705507438611, -2.802369389919810772 ) ) ;
#29254 = CARTESIAN_POINT ( 'NONE',  ( 1.603837441938149144, 120.9755568995931156, 0.09629321774905875986 ) ) ;
#29255 = LINE ( 'NONE', #18823, #18093 ) ;
#29256 = EDGE_CURVE ( 'NONE', #588, #31926, #10358, .T. ) ;
#29258 = ORIENTED_EDGE ( 'NONE', *, *, #22738, .T. ) ;
#29257 = CARTESIAN_POINT ( 'NONE',  ( -48.46138709710082537, 15.22468166490328123, -0.8008350491754933076 ) ) ;
#29259 = CARTESIAN_POINT ( 'NONE',  ( -8.798071503329609300, 117.6842349159552867, -0.1758064076808953657 ) ) ;
#29260 = CARTESIAN_POINT ( 'NONE',  ( -47.84356795211461844, 19.38525671449500010, -5.197506975155170572 ) ) ;
#29261 = CARTESIAN_POINT ( 'NONE',  ( 11.66725022231030984, 17.14500000000046498, -5.016499999999999737 ) ) ;
#29262 = CARTESIAN_POINT ( 'NONE',  ( -33.42971872652992005, 49.93539301574497102, 1.269999999999992468 ) ) ;
#29263 = CARTESIAN_POINT ( 'NONE',  ( -8.243407495045023126, 120.2654484654224092, -1.445016461426329224 ) ) ;
#29264 = CIRCLE ( 'NONE', #6170, 0.5080000000000000071 ) ;
#29265 = CARTESIAN_POINT ( 'NONE',  ( -5.871452009091403745, 77.01756250000002524, 5.016499999999999737 ) ) ;
#29266 = CARTESIAN_POINT ( 'NONE',  ( -5.106395947886143816, 78.95054594174945350, -5.392902600000144986 ) ) ;
#29267 = CARTESIAN_POINT ( 'NONE',  ( -54.55302389503632554, 12.80492160976152327, 0.5954867740797897824 ) ) ;
#29268 = CARTESIAN_POINT ( 'NONE',  ( -57.66338803320029882, 2.692357263605615891, 1.869785753600835987 ) ) ;
#29269 = CARTESIAN_POINT ( 'NONE',  ( -15.14699153459433845, 156.1345691653134509, -0.01578391296358631554 ) ) ;
#29270 = VERTEX_POINT ( 'NONE', #30733 ) ;
#29271 = CARTESIAN_POINT ( 'NONE',  ( -55.38777061991515183, 7.924152594517688719, -2.969223861581061996 ) ) ;
#29272 = CARTESIAN_POINT ( 'NONE',  ( 7.791101006339050450, 122.6066354939652570, 0.05439624365677588058 ) ) ;
#29273 = ADVANCED_FACE ( 'NONE', ( #17323 ), #2197, .T. ) ;
#29274 = ORIENTED_EDGE ( 'NONE', *, *, #14081, .T. ) ;
#29275 = DIRECTION ( 'NONE',  ( 5.188838149069472160E-16, -1.699382548006136559E-16, -1.000000000000000000 ) ) ;
#29277 = CARTESIAN_POINT ( 'NONE',  ( -15.53993717541254149, 147.5346097818530211, -0.5395553097850841473 ) ) ;
#29276 = TOROIDAL_SURFACE ( 'NONE', #10908, 0.3809999999999993947, 0.2540000000000000036 ) ;
#29278 = CARTESIAN_POINT ( 'NONE',  ( 4.583978111877545558, -14.49189839317011064, 4.572462404262108038 ) ) ;
#29279 = CARTESIAN_POINT ( 'NONE',  ( -13.10001109591399349, 121.1598417376693533, 1.052633080380691144 ) ) ;
#29280 = CARTESIAN_POINT ( 'NONE',  ( -31.59722765895411101, 71.22255575826451945, 1.523999999999991140 ) ) ;
#29281 = CARTESIAN_POINT ( 'NONE',  ( 13.37536684427238320, 156.9592627042916604, 0.5421920129525309440 ) ) ;
#29282 = EDGE_CURVE ( 'NONE', #35171, #10724, #35542, .T. ) ;
#29283 = CARTESIAN_POINT ( 'NONE',  ( 8.978876846644611831, 124.0550666853292086, 0.2683953620638208637 ) ) ;
#29284 = CARTESIAN_POINT ( 'NONE',  ( -41.28107547821696954, 23.22158991241121839, -1.270000000000005125 ) ) ;
#29285 = CARTESIAN_POINT ( 'NONE',  ( -0.08510646190747463147, 11.08924109716144280, -0.9717149503703566005 ) ) ;
#29286 = CARTESIAN_POINT ( 'NONE',  ( -1.824897337458840640, 116.5125207362610951, -0.1392185346034942595 ) ) ;
#29287 = CARTESIAN_POINT ( 'NONE',  ( -17.14500000000466784, 71.11999999999886768, -1.270000000000000684 ) ) ;
#29288 = CARTESIAN_POINT ( 'NONE',  ( -14.73199999999999399, 12.70000000000000462, 1.804149664503880250E-15 ) ) ;
#29289 = ORIENTED_EDGE ( 'NONE', *, *, #1147, .T. ) ;
#29290 = CARTESIAN_POINT ( 'NONE',  ( -2.623632515124386444, 116.9061775504940641, 0.4731523196332259040 ) ) ;
#29291 = EDGE_LOOP ( 'NONE', ( #23546, #23493 ) ) ;
#29292 = CARTESIAN_POINT ( 'NONE',  ( -58.30309248033832858, -0.1506202810087469701, -0.3290154619008041070 ) ) ;
#29293 = CARTESIAN_POINT ( 'NONE',  ( 13.21493909911900033, 121.0513591912305316, 1.522979426720440843 ) ) ;
#29294 = CARTESIAN_POINT ( 'NONE',  ( 16.44572402506187103, 128.5611466799914240, -1.520858254922803354 ) ) ;
#29295 = CARTESIAN_POINT ( 'NONE',  ( -0.2870776928289196506, 5.753151106566044781, -0.9307745581249481370 ) ) ;
#29296 = CARTESIAN_POINT ( 'NONE',  ( 6.828157356468467221, 12.44753447943134184, 4.948315318077098901 ) ) ;
#29297 = CARTESIAN_POINT ( 'NONE',  ( -13.91935487398219529, 155.8415165211600595, -1.849969996916311699 ) ) ;
#29298 = CARTESIAN_POINT ( 'NONE',  ( 4.890857177472106798, 117.7454522775086758, -0.7293204476797061631 ) ) ;
#29299 = AXIS2_PLACEMENT_3D ( 'NONE', #36554, #33357, #17563 ) ;
#29300 = DIRECTION ( 'NONE',  ( -0.8745520943968235761, 0.4849315768086558398, -5.691349986800547879E-16 ) ) ;
#29301 = CARTESIAN_POINT ( 'NONE',  ( 10.33346200648606050, 123.4707319107414492, -0.9080611472405731854 ) ) ;
#29302 = CARTESIAN_POINT ( 'NONE',  ( -9.007539097974415654, 123.9742709865185191, -0.1460878630902625874 ) ) ;
#29303 = ORIENTED_EDGE ( 'NONE', *, *, #35725, .F. ) ;
#29304 = CARTESIAN_POINT ( 'NONE',  ( -18.13772925547832315, 148.8986565181125457, -2.425799293919265409 ) ) ;
#29305 = CARTESIAN_POINT ( 'NONE',  ( 2.988498945533646367, -15.63929389023541106, 5.494461050752756925 ) ) ;
#29306 = CARTESIAN_POINT ( 'NONE',  ( 4.787223994907250813, 118.5931160184169073, 0.9409944917690892252 ) ) ;
#29307 = TOROIDAL_SURFACE ( 'NONE', #40927, 0.3810000000000001719, 0.2540000000000000036 ) ;
#29308 = CARTESIAN_POINT ( 'NONE',  ( -48.16508968810062896, 19.01313136326716347, -5.219744232931991412 ) ) ;
#29309 = ORIENTED_EDGE ( 'NONE', *, *, #26920, .F. ) ;
#29310 = PRODUCT ( 'Wing Lever', 'Wing Lever', '', ( #37064 ) ) ;
#29311 = CARTESIAN_POINT ( 'NONE',  ( 11.58192335640127446, 123.0696236843973281, 1.706247406239837616 ) ) ;
#29312 = CARTESIAN_POINT ( 'NONE',  ( -15.76285804746350649, 145.9067145067647857, -0.3149794173055759927 ) ) ;
#29313 = TOROIDAL_SURFACE ( 'NONE', #10938, 0.3809999999999999498, 0.2540000000000000036 ) ;
#29314 = LINE ( 'NONE', #22475, #11662 ) ;
#29315 = CARTESIAN_POINT ( 'NONE',  ( -4.584908976608091713, 124.7699485019152945, -0.08702032153807684467 ) ) ;
#29316 = CARTESIAN_POINT ( 'NONE',  ( 4.725500162001525339, -13.89046571553399900, -6.993667195001821213 ) ) ;
#29317 = CARTESIAN_POINT ( 'NONE',  ( 8.743035643995668238, 123.3024417045633498, 0.5730362264965975783 ) ) ;
#29318 = CARTESIAN_POINT ( 'NONE',  ( 3.877771370679228280, 117.0975898859979054, -0.4181078409183315303 ) ) ;
#29319 = CARTESIAN_POINT ( 'NONE',  ( -17.14500000000466784, 71.11999999999886768, 1.523999999999998689 ) ) ;
#29320 = CARTESIAN_POINT ( 'NONE',  ( -11.56352105402813280, 78.55269139521317356, -1.269999999999998908 ) ) ;
#29321 = CARTESIAN_POINT ( 'NONE',  ( -3.707388773974424900, 116.6237204831772232, -0.06043239539139034361 ) ) ;
#29322 = ORIENTED_EDGE ( 'NONE', *, *, #17768, .T. ) ;
#29323 = CARTESIAN_POINT ( 'NONE',  ( 6.381125341793176808, 120.0353217841789331, -0.9518924694056809521 ) ) ;
#29324 = CARTESIAN_POINT ( 'NONE',  ( 3.843300253784490028, -15.24301522717705026, 5.225518813476231372 ) ) ;
#29325 = CARTESIAN_POINT ( 'NONE',  ( -15.83096054209209136, 147.2950763206921181, -1.041347660067663217 ) ) ;
#29326 = CARTESIAN_POINT ( 'NONE',  ( 2.954207113090831616, -14.52495373116942368, 5.111795949899043734 ) ) ;
#29327 = CARTESIAN_POINT ( 'NONE',  ( -5.153942072456670687, 116.8381265693619895, -0.06466201385226102993 ) ) ;
#29328 = AXIS2_PLACEMENT_3D ( 'NONE', #25573, #28565, #38577 ) ;
#29329 = CARTESIAN_POINT ( 'NONE',  ( 4.716951831472176337, 116.7562497393984415, 0.1081823505139637015 ) ) ;
#29330 = ADVANCED_FACE ( 'NONE', ( #14539 ), #17161, .T. ) ;
#29331 = B_SPLINE_CURVE_WITH_KNOTS ( 'NONE', 3,
 ( #4321, #26453, #29861, #40308, #39456, #13672 ),
 .UNSPECIFIED., .F., .F.,
 ( 4, 2, 4 ),
 ( 0.0007477044786395083131, 0.001108740074962858389, 0.001469775671286208465 ),
 .UNSPECIFIED. ) ;
#29332 = VERTEX_POINT ( 'NONE', #21130 ) ;
#29333 = CARTESIAN_POINT ( 'NONE',  ( -4.544942180623752215, 12.81246518813932589, 0.8472608254572608910 ) ) ;
#29334 = CARTESIAN_POINT ( 'NONE',  ( -4.713631738767456447, 116.7564862437112794, -0.09418957996065560612 ) ) ;
#29335 = CARTESIAN_POINT ( 'NONE',  ( -17.14499999999999957, 71.11999999999999034, -1.904999999999999583 ) ) ;
#29336 = FACE_OUTER_BOUND ( 'NONE', #4342, .T. ) ;
#29337 = CARTESIAN_POINT ( 'NONE',  ( 6.993874078755136559, 121.7930633702997341, 0.5635671808028978047 ) ) ;
#29338 = CARTESIAN_POINT ( 'NONE',  ( -2.394960105286914942, 16.54535949628658997, -3.951836011466995036 ) ) ;
#29339 = CARTESIAN_POINT ( 'NONE',  ( 16.14352587498443015, 122.8183540351560907, 1.297681478882586337 ) ) ;
#29340 = FACE_OUTER_BOUND ( 'NONE', #9935, .T. ) ;
#29342 = CARTESIAN_POINT ( 'NONE',  ( 18.67489051167924785, 151.9584835496716266, -1.528205706551668319 ) ) ;
#29341 = CARTESIAN_POINT ( 'NONE',  ( 3.150244473240279675, -14.07033042043420146, 1.813758411523331393 ) ) ;
#29343 = VECTOR ( 'NONE', #29985, 1000.000000000000000 ) ;
#29344 = CARTESIAN_POINT ( 'NONE',  ( 4.531904421025400254, 4.026177021345840323, -0.9239884639389631671 ) ) ;
#29345 = CARTESIAN_POINT ( 'NONE',  ( -5.835170694357168841, 117.3723397083485622, -0.6929373658347460774 ) ) ;
#29346 = ORIENTED_EDGE ( 'NONE', *, *, #2160, .T. ) ;
#29347 = CARTESIAN_POINT ( 'NONE',  ( -3.695597174622082370, 120.9852966486377710, 0.1212977071129683060 ) ) ;
#29348 = CARTESIAN_POINT ( 'NONE',  ( 2.834973442847717351, -15.21714937722351557, 5.773325752997570781 ) ) ;
#29349 = AXIS2_PLACEMENT_3D ( 'NONE', #16210, #25602, #9416 ) ;
#29350 = CYLINDRICAL_SURFACE ( 'NONE', #33619, 3.175000000000001155 ) ;
#29351 = CARTESIAN_POINT ( 'NONE',  ( -1.698985622072688884, 106.4942957007677649, -5.056388078100372496 ) ) ;
#29352 = ORIENTED_EDGE ( 'NONE', *, *, #8411, .F. ) ;
#29353 = CARTESIAN_POINT ( 'NONE',  ( 1.258058525836107444, 118.8689652838214244, 0.6902481975293249805 ) ) ;
#29354 = LINE ( 'NONE', #22938, #20952 ) ;
#29355 = CARTESIAN_POINT ( 'NONE',  ( 9.163388821854780986, 124.2347608867413413, 0.1831063163140475014 ) ) ;
#29356 = VECTOR ( 'NONE', #27488, 1000.000000000000227 ) ;
#29357 = CIRCLE ( 'NONE', #2169, 15.21260244842765808 ) ;
#29358 = CARTESIAN_POINT ( 'NONE',  ( -22.64859486804675726, 149.7032342875954498, 0.6240689893612101358 ) ) ;
#29359 = CIRCLE ( 'NONE', #21769, 17.68910244842765778 ) ;
#29360 = CARTESIAN_POINT ( 'NONE',  ( 4.789291700406207219, 116.8922783744782379, -0.1888386708474939224 ) ) ;
#29361 = CARTESIAN_POINT ( 'NONE',  ( -5.322370864742718588, 56.51499999999976609, -5.239063871132868755 ) ) ;
#29362 = CARTESIAN_POINT ( 'NONE',  ( -52.36976898921572143, 11.96785871290047787, 4.095024579493532713 ) ) ;
#29363 = CARTESIAN_POINT ( 'NONE',  ( -49.10997966587441965, 20.64911895071488956, 3.108984601230522671 ) ) ;
#29364 = CARTESIAN_POINT ( 'NONE',  ( 1.934325240867707629, -15.05852118660004635, 5.638101517764280146 ) ) ;
#29365 = CARTESIAN_POINT ( 'NONE',  ( -51.81113891419111894, 13.24950054771400332, 4.495723625053109629 ) ) ;
#29366 = CARTESIAN_POINT ( 'NONE',  ( 2.666490510518176649, -13.49855353256042712, 0.05227394649444803282 ) ) ;
#29367 = CARTESIAN_POINT ( 'NONE',  ( -4.613770077645467538, 118.0656789020681998, 0.5556151127989765737 ) ) ;
#29368 = CARTESIAN_POINT ( 'NONE',  ( -5.614623559985635559, 78.91041036408817888, -5.070733448224208573 ) ) ;
#29369 = ORIENTED_EDGE ( 'NONE', *, *, #34191, .T. ) ;
#29370 = EDGE_LOOP ( 'NONE', ( #26881, #22390, #17534, #5321 ) ) ;
#29371 = CARTESIAN_POINT ( 'NONE',  ( -0.9749357855001491435, 115.6909491485452435, -1.750966270793492541 ) ) ;
#29372 = CARTESIAN_POINT ( 'NONE',  ( 5.997780686918567028, 119.2096731566373364, -1.027357156148055228 ) ) ;
#29373 = CARTESIAN_POINT ( 'NONE',  ( -4.366878780879607014, 111.2667756541687538, -3.131538613950388239 ) ) ;
#29374 = CARTESIAN_POINT ( 'NONE',  ( 4.661500840997910622, 117.9823968663990144, 0.8616593033297639259 ) ) ;
#29375 = CARTESIAN_POINT ( 'NONE',  ( -46.60530155212504155, 26.17382724835476537, -0.4656666666666756105 ) ) ;
#29376 = CARTESIAN_POINT ( 'NONE',  ( -13.09552101555883574, 130.8944540161131442, -1.428626934261719050 ) ) ;
#29377 = CARTESIAN_POINT ( 'NONE',  ( -2.395404871435389271, 115.7029496080882467, -1.700622835054004023 ) ) ;
#29378 = CARTESIAN_POINT ( 'NONE',  ( -6.059261036834476144, 56.98375738874752017, 5.016499999999999737 ) ) ;
#29379 = DIRECTION ( 'NONE',  ( -0.7308269722843410143, 0.6825627711659222330, -8.537024980200883941E-16 ) ) ;
#29380 = CARTESIAN_POINT ( 'NONE',  ( 7.643874070029819556, 124.9344662015457317, 0.1527427953284561379 ) ) ;
#29381 = CARTESIAN_POINT ( 'NONE',  ( -3.477534164838183006, 156.5024071230465097, -1.413294873543960106 ) ) ;
#29382 = CARTESIAN_POINT ( 'NONE',  ( -13.70915846191426191, 16.90875728684043011, -5.016499999999999737 ) ) ;
#29383 = CARTESIAN_POINT ( 'NONE',  ( -0.01887828017123771920, 156.5412816204240301, 0.9447463363288814975 ) ) ;
#29384 = LINE ( 'NONE', #38979, #11994 ) ;
#29385 = CARTESIAN_POINT ( 'NONE',  ( -7.778077869716700121, 154.6678004290674266, -0.09965222998851200331 ) ) ;
#29386 = CARTESIAN_POINT ( 'NONE',  ( 3.501419995798253915, -2.955197114699519734, 3.043391175950921568 ) ) ;
#29388 = EDGE_LOOP ( 'NONE', ( #27412, #9682, #22024, #7095 ) ) ;
#29387 = CARTESIAN_POINT ( 'NONE',  ( 23.06261834269074029, 146.6371693212631158, 1.324134011023373025 ) ) ;
#29389 = DIRECTION ( 'NONE',  ( -1.000000000000000000, -1.092739197465705287E-15, 0.000000000000000000 ) ) ;
#29390 = CARTESIAN_POINT ( 'NONE',  ( 3.520778385322295811, -15.02221911624387829, 1.583774285062736986 ) ) ;
#29391 = CARTESIAN_POINT ( 'NONE',  ( -18.66004122726579695, 149.2887123452801745, 1.736808470001687255 ) ) ;
#29392 = CARTESIAN_POINT ( 'NONE',  ( -0.9744428630873758213, 7.697845052497760854, 0.001242513977635927719 ) ) ;
#29393 = CARTESIAN_POINT ( 'NONE',  ( -22.44855437653378871, 150.5824416163731314, -1.170575646458954067 ) ) ;
#29394 = VECTOR ( 'NONE', #37922, 1000.000000000000000 ) ;
#29395 = CARTESIAN_POINT ( 'NONE',  ( 0.3393679441828953980, -8.777600141791896959, -0.9147772600509928020 ) ) ;
#29396 = ORIENTED_EDGE ( 'NONE', *, *, #39977, .F. ) ;
#29397 = ORIENTED_EDGE ( 'NONE', *, *, #13947, .F. ) ;
#29398 = CARTESIAN_POINT ( 'NONE',  ( -42.83068693079387401, 21.70476352389080787, 1.889833665869958157 ) ) ;
#29399 = CARTESIAN_POINT ( 'NONE',  ( 4.994922087954005718, 114.3796182124986984, 1.954983995200229030 ) ) ;
#29400 = CARTESIAN_POINT ( 'NONE',  ( -4.574562528865663502, 155.9125706774115940, 0.7527123864290743427 ) ) ;
#29401 = CARTESIAN_POINT ( 'NONE',  ( 2.780001287168888613, -14.74817992026429536, 5.465600930587551254 ) ) ;
#29402 = CARTESIAN_POINT ( 'NONE',  ( 9.357607378341723958, 155.0893615026619159, -1.530462696531121214 ) ) ;
#29403 = CARTESIAN_POINT ( 'NONE',  ( -13.64693284513013793, 123.6869008171703541, -1.914747182567867023 ) ) ;
#29404 = LINE ( 'NONE', #244, #2341 ) ;
#29405 = CARTESIAN_POINT ( 'NONE',  ( 2.858040400949144022, -14.78363303536489681, 4.300485631455113200 ) ) ;
#29406 = CARTESIAN_POINT ( 'NONE',  ( -4.993862003731174504, 32.72552215703572642, 2.980277739178222252 ) ) ;
#29407 = CARTESIAN_POINT ( 'NONE',  ( 5.925782188533577965, 121.5237468798633955, -0.003878672073842357685 ) ) ;
#29408 = ORIENTED_EDGE ( 'NONE', *, *, #19550, .T. ) ;
#29409 = DIRECTION ( 'NONE',  ( -1.000000000000000000, 0.000000000000000000, 0.000000000000000000 ) ) ;
#29410 = CARTESIAN_POINT ( 'NONE',  ( 12.21488373879589240, 55.24500000000000455, 4.381499999999999950 ) ) ;
#29411 =( BOUNDED_CURVE ( )  B_SPLINE_CURVE ( 3, ( #23294, #36332, #23720, #22870 ),
 .UNSPECIFIED., .F., .T. ) 
 B_SPLINE_CURVE_WITH_KNOTS ( ( 4, 4 ),
 ( 1.570796326794897890, 3.141592653589793116 ),
 .UNSPECIFIED. ) 
 CURVE ( )  GEOMETRIC_REPRESENTATION_ITEM ( )  RATIONAL_B_SPLINE_CURVE ( ( 1.000000000000000000, 0.8047378541243652705, 0.8047378541243652705, 1.000000000000000000 ) ) 
 REPRESENTATION_ITEM ( '' )  );
#29412 = CARTESIAN_POINT ( 'NONE',  ( -38.65395868481546415, 29.38327706004843876, -1.524000000000004906 ) ) ;
#29413 = CARTESIAN_POINT ( 'NONE',  ( -58.13403979463087268, 0.7724927387386393285, 1.216435378341239382 ) ) ;
#29414 = B_SPLINE_CURVE_WITH_KNOTS ( 'NONE', 3,
 ( #161, #9312, #12710, #35936 ),
 .UNSPECIFIED., .F., .F.,
 ( 4, 4 ),
 ( 0.0001462341759615505836, 0.0005711421393943891126 ),
 .UNSPECIFIED. ) ;
#29415 = CARTESIAN_POINT ( 'NONE',  ( 14.84180086987428382, 120.3134675335783754, 0.1939203138368898183 ) ) ;
#29416 = CARTESIAN_POINT ( 'NONE',  ( -6.742182786529062000, 121.2177056076135528, 0.07361405433131856801 ) ) ;
#29417 = AXIS2_PLACEMENT_3D ( 'NONE', #37497, #28117, #8322 ) ;
#29418 = CARTESIAN_POINT ( 'NONE',  ( -1.144953672747696993, 115.6909491485452435, 1.703244984983935506 ) ) ;
#29419 = DIRECTION ( 'NONE',  ( 0.9816537812491076265, 0.1906721105965138718, 4.769617732184456426E-16 ) ) ;
#29420 = CARTESIAN_POINT ( 'NONE',  ( 0.4700063951662839523, 38.82598460892266701, -1.223737656376347127 ) ) ;
#29421 = CARTESIAN_POINT ( 'NONE',  ( 13.39049918543318185, 121.7711344121973411, 1.690880791723282428 ) ) ;
#29422 = CARTESIAN_POINT ( 'NONE',  ( 4.233688895176465294, 13.94658232072815807, -1.861163356065342001 ) ) ;
#29423 = CARTESIAN_POINT ( 'NONE',  ( 6.528609751734300914, 25.78175851779908356, 5.377075232920663694 ) ) ;
#29424 = CARTESIAN_POINT ( 'NONE',  ( -2.168094803691708705, 116.7617983115602840, -0.5049745822317547317 ) ) ;
#29425 = CARTESIAN_POINT ( 'NONE',  ( -1.155499320159524723, 111.9985432423065959, -2.960082065640199822 ) ) ;
#29426 = CARTESIAN_POINT ( 'NONE',  ( -17.14500000000000313, 71.11999999999999034, -5.714999999999998970 ) ) ;
#29427 = DIRECTION ( 'NONE',  ( 4.017660918040594346E-17, -1.000000000000000000, -2.376309959284834438E-19 ) ) ;
#29428 = CARTESIAN_POINT ( 'NONE',  ( -2.879560631192479292, 105.1244045648011678, 4.501302620457409809 ) ) ;
#29429 = CARTESIAN_POINT ( 'NONE',  ( 4.573446973487649281, 17.56025517495590904, -0.6989348988664985107 ) ) ;
#29430 = DIRECTION ( 'NONE',  ( -0.4849315768086534528, -0.8745520943968250194, -1.030032898892974942E-16 ) ) ;
#29431 = CARTESIAN_POINT ( 'NONE',  ( -17.31377588638430964, 122.7721875394316555, -0.3459704467065360944 ) ) ;
#29432 = CARTESIAN_POINT ( 'NONE',  ( 2.664052010559913253, -13.52006206191685322, 0.08958796903007473778 ) ) ;
#29433 = ADVANCED_FACE ( 'NONE', ( #951 ), #864, .T. ) ;
#29434 = EDGE_CURVE ( 'NONE', #34925, #11069, #23257, .T. ) ;
#29435 = CARTESIAN_POINT ( 'NONE',  ( 1.751097875588997654, 120.5851793143259130, -0.4017021596164529473 ) ) ;
#29436 = CARTESIAN_POINT ( 'NONE',  ( -11.47343314416685978, 118.8698716516685465, 0.3113556051519841272 ) ) ;
#29437 = AXIS2_PLACEMENT_3D ( 'NONE', #33156, #3772, #10972 ) ;
#29438 = ORIENTED_EDGE ( 'NONE', *, *, #4529, .F. ) ;
#29439 = CARTESIAN_POINT ( 'NONE',  ( 5.664977208693799504, 77.01756249999996840, 5.033228321271210781 ) ) ;
#29440 = ORIENTED_EDGE ( 'NONE', *, *, #38665, .T. ) ;
#29441 = CARTESIAN_POINT ( 'NONE',  ( -17.64950171984354554, 84.16951713491046405, 1.269999999999996243 ) ) ;
#29442 = CARTESIAN_POINT ( 'NONE',  ( 5.792286216032899837, -14.99041835605292938, 0.9165201714659111376 ) ) ;
#29443 = CARTESIAN_POINT ( 'NONE',  ( -12.99265913520525473, 122.2940260782629451, 1.284300974089672920 ) ) ;
#29444 = CARTESIAN_POINT ( 'NONE',  ( 14.33513709641994893, 121.5541609676003389, -0.9327927267376098230 ) ) ;
#29445 = CARTESIAN_POINT ( 'NONE',  ( -0.2084201458593382406, 5.265951782950084592, 4.622859108429906883 ) ) ;
#29446 = CARTESIAN_POINT ( 'NONE',  ( -58.72763989320913680, -0.3148928600554901092, -0.2588867910284781138 ) ) ;
#29447 = ORIENTED_EDGE ( 'NONE', *, *, #38940, .F. ) ;
#29448 = LINE ( 'NONE', #29871, #41537 ) ;
#29449 = CARTESIAN_POINT ( 'NONE',  ( 0.3561418115364049508, 119.9741034315941732, 0.6738560125758275010 ) ) ;
#29450 = DIRECTION ( 'NONE',  ( -0.01731298258488003436, 0.9998501190848634312, 0.000000000000000000 ) ) ;
#29451 = CARTESIAN_POINT ( 'NONE',  ( -17.03225580939810158, 146.4457527449227143, 1.249628170391535731 ) ) ;
#29452 = CARTESIAN_POINT ( 'NONE',  ( -6.642767299088215313E-14, 101.1854662015457365, -1.199848199765585135E-18 ) ) ;
#29453 = CARTESIAN_POINT ( 'NONE',  ( 18.22015820038723533, 148.8986565181125457, -1.699282175587853327 ) ) ;
#29454 = CARTESIAN_POINT ( 'NONE',  ( -6.788760123629518972, 157.9234729166680040, -1.828055096104673538 ) ) ;
#29455 = CARTESIAN_POINT ( 'NONE',  ( -57.80205714066466527, 2.371715784325115095, -1.753227392946310470 ) ) ;
#29456 = VECTOR ( 'NONE', #66, 1000.000000000000000 ) ;
#29457 = EDGE_LOOP ( 'NONE', ( #37203, #1628 ) ) ;
#29458 = CARTESIAN_POINT ( 'NONE',  ( 4.517430400727893591, 118.1170754611382137, -0.5419986605907590738 ) ) ;
#29459 = CARTESIAN_POINT ( 'NONE',  ( 16.12610658153775489, 147.0533492130506943, -0.6457432798159421505 ) ) ;
#29460 = ORIENTED_EDGE ( 'NONE', *, *, #27896, .T. ) ;
#29461 = CARTESIAN_POINT ( 'NONE',  ( -7.341258159293269081, 120.8389031223305352, -1.207285925005196603 ) ) ;
#29462 = CARTESIAN_POINT ( 'NONE',  ( 3.752486096903807855, -15.17702595220350759, -0.4382564666907802220 ) ) ;
#29463 = CARTESIAN_POINT ( 'NONE',  ( -6.654617103318593247E-14, 104.6144662015457243, 1.534725424433578570E-31 ) ) ;
#29464 = CIRCLE ( 'NONE', #1606, 0.2540000000000000036 ) ;
#29465 = EDGE_CURVE ( 'NONE', #11359, #12283, #34844, .T. ) ;
#29466 = PLANE ( 'NONE',  #36983 ) ;
#29467 = CARTESIAN_POINT ( 'NONE',  ( -4.757398851944955709, 117.7257754445831921, 0.9114319017062125772 ) ) ;
#29468 = CARTESIAN_POINT ( 'NONE',  ( 11.08617792162969096, 123.6647009725989648, 1.535475951868171984 ) ) ;
#29469 = CARTESIAN_POINT ( 'NONE',  ( -1.209753656675892186, 31.97884461091921082, 1.539940357435441776 ) ) ;
#29470 = CARTESIAN_POINT ( 'NONE',  ( 2.889066315880882030, 25.55657059589919911, 3.609430016826872478 ) ) ;
#29471 = CARTESIAN_POINT ( 'NONE',  ( 9.045001602728808265, 123.9859359328134190, 0.2652644514531634634 ) ) ;
#29472 = DIRECTION ( 'NONE',  ( -0.9575201071113178530, 0.2883665106726683858, -8.537024980200786319E-16 ) ) ;
#29473 = CARTESIAN_POINT ( 'NONE',  ( -48.25086062633820916, 17.91646674446130305, -3.976701633436076300 ) ) ;
#29474 = CARTESIAN_POINT ( 'NONE',  ( -14.39766717389550266, 30.83083951148099189, 1.905000000000008686 ) ) ;
#29475 = DIRECTION ( 'NONE',  ( 0.4849315768086535638, 0.8745520943968251304, 1.030032898892975065E-16 ) ) ;
#29476 = CIRCLE ( 'NONE', #19958, 0.2539999999999998925 ) ;
#29477 = CARTESIAN_POINT ( 'NONE',  ( -46.77395155747410627, 25.81392106044808799, -1.433409421412224827 ) ) ;
#29478 = CARTESIAN_POINT ( 'NONE',  ( -33.42971872652992005, 49.93539301574497102, -1.270000000000005569 ) ) ;
#29479 = CARTESIAN_POINT ( 'NONE',  ( -8.547848780159753801, 118.8034570524430933, -1.212240055924699966 ) ) ;
#29480 = CARTESIAN_POINT ( 'NONE',  ( -5.177913976931283635, 53.58606250000000415, 5.372100000000000541 ) ) ;
#29481 = DIRECTION ( 'NONE',  ( 5.188838149069471174E-16, -1.699382548006136313E-16, -1.000000000000000000 ) ) ;
#29482 = DIRECTION ( 'NONE',  ( 5.188838149069472160E-16, -1.699382548006136559E-16, -1.000000000000000000 ) ) ;
#29483 = CARTESIAN_POINT ( 'NONE',  ( -56.91937565786339803, 5.591339438888828894, -1.031528444718396757E-14 ) ) ;
#29484 = ADVANCED_FACE ( 'NONE', ( #28387 ), #18574, .T. ) ;
#29485 = CARTESIAN_POINT ( 'NONE',  ( -56.22331024217277928, 5.808995339285999648, 2.850545730341239814 ) ) ;
#29486 = CARTESIAN_POINT ( 'NONE',  ( -18.64921795038435803, 125.2334963081946313, -0.1144521110716926748 ) ) ;
#29487 = CIRCLE ( 'NONE', #12493, 14.73199999999999577 ) ;
#29488 = ORIENTED_EDGE ( 'NONE', *, *, #39980, .F. ) ;
#29489 = CARTESIAN_POINT ( 'NONE',  ( -54.06930887699937216, 11.98206827348202808, -2.380698788532477295 ) ) ;
#29490 = CARTESIAN_POINT ( 'NONE',  ( 6.056944315494892983, 121.4421416482665421, 0.1030667194366131911 ) ) ;
#29491 = EDGE_LOOP ( 'NONE', ( #39721, #40809, #31680, #4918 ) ) ;
#29492 = CARTESIAN_POINT ( 'NONE',  ( -5.332909801388204585, 115.7029491485453718, -0.1078398302286824040 ) ) ;
#29493 = CARTESIAN_POINT ( 'NONE',  ( -0.6438746309741667506, 120.9974662015465867, -0.01286614746332115887 ) ) ;
#29494 = CARTESIAN_POINT ( 'NONE',  ( 4.440325138859688714, -14.57630248335078882, 4.728313687495418804 ) ) ;
#29495 = CARTESIAN_POINT ( 'NONE',  ( -21.36815210116614949, 148.0064520001644723, 1.462276224275804060 ) ) ;
#29496 = CARTESIAN_POINT ( 'NONE',  ( 10.92199999999999704, 55.24500000000000455, 0.000000000000000000 ) ) ;
#29497 = CIRCLE ( 'NONE', #27462, 0.5080000000000002292 ) ;
#29498 = CARTESIAN_POINT ( 'NONE',  ( 16.04055624107191491, 121.3766923467913585, 0.6455242483069041359 ) ) ;
#29499 = CARTESIAN_POINT ( 'NONE',  ( 2.159762389889169132, -15.63309910277781078, 5.565077868897359004 ) ) ;
#29500 = CARTESIAN_POINT ( 'NONE',  ( 4.831409462241198050, 118.5266822147775940, -0.7504941915039914369 ) ) ;
#29501 = CARTESIAN_POINT ( 'NONE',  ( -0.8226642509504364931, 2.890957568680109446, -0.5268263738024351328 ) ) ;
#29502 = CARTESIAN_POINT ( 'NONE',  ( -22.52498503541054120, 150.7873321363286152, -0.6028683204863920508 ) ) ;
#29503 = CARTESIAN_POINT ( 'NONE',  ( -15.21260244842765275, 9.026346327358517385, 1.863006489516811765E-15 ) ) ;
#29504 = EDGE_CURVE ( 'NONE', #20165, #37020, #8466, .T. ) ;
#29505 = LINE ( 'NONE', #22661, #19307 ) ;
#29506 = ORIENTED_EDGE ( 'NONE', *, *, #4770, .T. ) ;
#29507 = CARTESIAN_POINT ( 'NONE',  ( -8.743388953545744968, 118.0097374530782588, 0.4280054902111584125 ) ) ;
#29508 = ORIENTED_EDGE ( 'NONE', *, *, #38131, .T. ) ;
#29509 = CARTESIAN_POINT ( 'NONE',  ( -18.17603978048573765, 146.7121067869193496, 1.621728993581971867 ) ) ;
#29510 = CARTESIAN_POINT ( 'NONE',  ( -58.36980953069939915, -0.2915895811168507379, -0.001722197669518234003 ) ) ;
#29511 = CARTESIAN_POINT ( 'NONE',  ( 18.79035964875395237, 131.8417273817641444, 2.102833481017198469 ) ) ;
#29512 = CARTESIAN_POINT ( 'NONE',  ( 15.12798499870458535, 125.5446871707752763, -1.421763802809897115 ) ) ;
#29513 = CARTESIAN_POINT ( 'NONE',  ( -0.01718310852247704676, 5.323846764136113130, -0.9747645957998940514 ) ) ;
#29514 = CARTESIAN_POINT ( 'NONE',  ( -7.226289359486380626, 158.3006260280594404, -1.552328403643544963 ) ) ;
#29515 = CARTESIAN_POINT ( 'NONE',  ( 4.613544267573807645, 118.0656495166530817, -0.5557507275274983227 ) ) ;
#29516 = CARTESIAN_POINT ( 'NONE',  ( 7.694663930960251363, 124.9344662015457317, 0.1537576976229974857 ) ) ;
#29517 = CARTESIAN_POINT ( 'NONE',  ( 14.42666092703562875, 134.5679602169015254, -1.107736707283930810 ) ) ;
#29518 = CARTESIAN_POINT ( 'NONE',  ( -0.6418402141072927503, 156.3034662015456888, 0.01455126635812875602 ) ) ;
#29519 = ORIENTED_EDGE ( 'NONE', *, *, #5838, .F. ) ;
#29520 = CARTESIAN_POINT ( 'NONE',  ( -2.417314592637459736, 119.3768144667271542, -0.7569762546260363489 ) ) ;
#29521 = CARTESIAN_POINT ( 'NONE',  ( 3.601051898931722395, -15.74651769575186044, 4.782909482641136911 ) ) ;
#29522 = CIRCLE ( 'NONE', #28814, 3.175000000000001155 ) ;
#29523 = LINE ( 'NONE', #28578, #22417 ) ;
#29524 = CARTESIAN_POINT ( 'NONE',  ( -46.97515415817095175, 24.89137758704647396, -2.045406795549908896 ) ) ;
#29525 = VERTEX_POINT ( 'NONE', #11770 ) ;
#29526 = VECTOR ( 'NONE', #30106, 1000.000000000000000 ) ;
#29527 = CARTESIAN_POINT ( 'NONE',  ( 11.45041423386206425, 122.9335272575421669, 1.692945391654126608 ) ) ;
#29528 = CARTESIAN_POINT ( 'NONE',  ( -4.997525182441642677, 56.61525291752813160, 5.184946129310923801 ) ) ;
#29529 = ADVANCED_FACE ( 'NONE', ( #28173, #31792 ), #31365, .F. ) ;
#29530 = CARTESIAN_POINT ( 'NONE',  ( 4.799643950526473191, 115.7029491485453292, 1.472414092453835588 ) ) ;
#29531 = VECTOR ( 'NONE', #30882, 1000.000000000000000 ) ;
#29532 = CARTESIAN_POINT ( 'NONE',  ( -1.889402974298121762, 108.8931014686503289, 4.028630146538900725 ) ) ;
#29533 = ADVANCED_FACE ( 'NONE', ( #6237 ), #2631, .F. ) ;
#29534 = CARTESIAN_POINT ( 'NONE',  ( 7.497756367663003019, 26.09243224653669913, 3.946719672664338319 ) ) ;
#29535 = CARTESIAN_POINT ( 'NONE',  ( 9.301285777573523816, 153.8845013697122965, 0.8210809464416258807 ) ) ;
#29536 = CARTESIAN_POINT ( 'NONE',  ( 0.01289612358321921490, 159.5048567107479585, -0.6453747585945881493 ) ) ;
#29537 = LINE ( 'NONE', #28895, #32879 ) ;
#29538 = AXIS2_PLACEMENT_3D ( 'NONE', #36442, #27473, #10440 ) ;
#29539 = CYLINDRICAL_SURFACE ( 'NONE', #35819, 0.2540000000000051106 ) ;
#29540 = UNCERTAINTY_MEASURE_WITH_UNIT (LENGTH_MEASURE( 1.000000000000000082E-05 ), #10690, 'distance_accuracy_value', 'NONE');
#29541 = CARTESIAN_POINT ( 'NONE',  ( -4.725057015249868542, 116.7592613395855352, -0.05262260997884638664 ) ) ;
#29542 = EDGE_CURVE ( 'NONE', #33508, #35910, #16458, .T. ) ;
#29543 = ORIENTED_EDGE ( 'NONE', *, *, #23787, .F. ) ;
#29544 = CARTESIAN_POINT ( 'NONE',  ( 6.768164194442967130, 121.0451091176095559, -0.7116084776782327648 ) ) ;
#29545 = CARTESIAN_POINT ( 'NONE',  ( 5.914793047224296885, -14.26696172101640414, 2.399059881747223955 ) ) ;
#29546 = CIRCLE ( 'NONE', #24756, 0.7619999999999984563 ) ;
#29547 = CARTESIAN_POINT ( 'NONE',  ( -13.71401989163329027, 150.2158912636999730, -0.8490545446796917695 ) ) ;
#29548 = CARTESIAN_POINT ( 'NONE',  ( 3.761132227337853351, -14.12294213130394027, 4.617837385609514733 ) ) ;
#29549 = CARTESIAN_POINT ( 'NONE',  ( -2.057861540686834800, 117.3535355059730705, 0.5007145131239727487 ) ) ;
#29550 = DIRECTION ( 'NONE',  ( 4.017660918040594346E-17, -1.000000000000000000, -2.376309959284834438E-19 ) ) ;
#29551 = CARTESIAN_POINT ( 'NONE',  ( -0.0007535234283137855638, 116.4338605912342786, 0.03770939363766613595 ) ) ;
#29552 = EDGE_LOOP ( 'NONE', ( #23461, #35630, #39110, #8378 ) ) ;
#29553 = CARTESIAN_POINT ( 'NONE',  ( 1.068493265602401987, 5.690783753869971484, 4.496582723949734017 ) ) ;
#29554 = CARTESIAN_POINT ( 'NONE',  ( -3.789105058680120042, 105.1231779575318228, 3.768300612546575667 ) ) ;
#29555 = CARTESIAN_POINT ( 'NONE',  ( 9.925711944554072019, 78.55658865046544292, 5.016499999999999737 ) ) ;
#29556 = CARTESIAN_POINT ( 'NONE',  ( 1.906794157568332038, 106.4600999034464195, 4.997634466524000452 ) ) ;
#29557 = CARTESIAN_POINT ( 'NONE',  ( -8.076703871748769359, 121.3095967058478095, 0.9279539172270194758 ) ) ;
#29558 = CARTESIAN_POINT ( 'NONE',  ( -1.792273654952471595, 16.32048121479114045, -4.264856162967389785 ) ) ;
#29559 = CARTESIAN_POINT ( 'NONE',  ( 14.63850908477041202, 156.0817623197167450, 1.342817726712510540 ) ) ;
#29561 = CARTESIAN_POINT ( 'NONE',  ( 0.01051220311278149022, 117.9844940561907265, -0.5260736299896251467 ) ) ;
#29560 = CARTESIAN_POINT ( 'NONE',  ( 5.570730988718594290, 56.51499999999999346, 4.419918923950526768 ) ) ;
#29562 = CARTESIAN_POINT ( 'NONE',  ( 1.748379858460863856, 5.525481214791113871, -4.283037568778763848 ) ) ;
#29563 = CARTESIAN_POINT ( 'NONE',  ( -22.77131365710839717, 149.1304179266472261, -1.534847161028223939 ) ) ;
#29564 = ORIENTED_EDGE ( 'NONE', *, *, #11385, .F. ) ;
#29565 = CARTESIAN_POINT ( 'NONE',  ( -19.64403260974359355, 72.50569198072959409, -1.270000000000002238 ) ) ;
#29566 = ORIENTED_EDGE ( 'NONE', *, *, #22719, .T. ) ;
#29567 = EDGE_CURVE ( 'NONE', #31926, #38422, #25406, .T. ) ;
#29568 = CARTESIAN_POINT ( 'NONE',  ( -2.792630161979596348, 120.9517662584847102, 0.08501465617163909971 ) ) ;
#29569 = CARTESIAN_POINT ( 'NONE',  ( 3.633732803939692335, -15.12841498804032270, 5.400629595854979037 ) ) ;
#29570 = CARTESIAN_POINT ( 'NONE',  ( -5.078986093043186045, 79.34146620154574236, -0.1014902294541237954 ) ) ;
#29571 = CARTESIAN_POINT ( 'NONE',  ( -0.1816225517746203333, 105.8842979884732785, -5.338741224315539213 ) ) ;
#29572 = ORIENTED_EDGE ( 'NONE', *, *, #26904, .T. ) ;
#29573 = CARTESIAN_POINT ( 'NONE',  ( 15.73670139478151242, 128.5598958631237565, 2.193363351549679319 ) ) ;
#29574 = FACE_OUTER_BOUND ( 'NONE', #31201, .T. ) ;
#29575 = CARTESIAN_POINT ( 'NONE',  ( 11.03183784343224616, 128.0124916018596650, 0.2204423744267036411 ) ) ;
#29576 = CARTESIAN_POINT ( 'NONE',  ( -20.24728863611177587, 152.4988772720997190, 0.6427007754482431112 ) ) ;
#29577 = ADVANCED_FACE ( 'NONE', ( #25190 ), #37974, .T. ) ;
#29578 = CARTESIAN_POINT ( 'NONE',  ( 8.421720897435127640, 23.01747231734997357, -0.09500337383513672573 ) ) ;
#29579 = EDGE_CURVE ( 'NONE', #18130, #24697, #41604, .T. ) ;
#29580 = CARTESIAN_POINT ( 'NONE',  ( 22.41683308396147822, 150.7562895891929031, -0.1409227600426839200 ) ) ;
#29581 = CARTESIAN_POINT ( 'NONE',  ( -5.936184715466119144, 56.51499999999997925, -4.381499802639526209 ) ) ;
#29582 = CARTESIAN_POINT ( 'NONE',  ( -46.75382734339789437, 25.86353334213626098, 1.406704986510833866 ) ) ;
#29583 = CARTESIAN_POINT ( 'NONE',  ( -48.77319768356018415, 22.00425556813275563, 2.071420771163280605 ) ) ;
#29584 = CARTESIAN_POINT ( 'NONE',  ( 1.800280022787231538, -15.11108451883692894, 5.570910438324009561 ) ) ;
#29585 = CARTESIAN_POINT ( 'NONE',  ( -53.09398923718962493, 10.65108322687173548, 3.938325876039757478 ) ) ;
#29586 = DIRECTION ( 'NONE',  ( -5.188838149069472160E-16, 1.699382548006136559E-16, 1.000000000000000000 ) ) ;
#29587 = CARTESIAN_POINT ( 'NONE',  ( -4.463662862426327038, 118.1585627870778410, 0.4268197071713389912 ) ) ;
#29588 = CARTESIAN_POINT ( 'NONE',  ( -58.37241122568484286, -0.2962816677227336770, -1.028586707908061473E-14 ) ) ;
#29589 = ORIENTED_EDGE ( 'NONE', *, *, #10189, .F. ) ;
#29590 = VERTEX_POINT ( 'NONE', #9009 ) ;
#29591 = CARTESIAN_POINT ( 'NONE',  ( -4.999645142055948455, 117.4030427321881263, 0.8338872319069162709 ) ) ;
#29592 = CARTESIAN_POINT ( 'NONE',  ( 8.342983529710069845, 120.0295035570879207, -1.117190174572594730 ) ) ;
#29593 = CARTESIAN_POINT ( 'NONE',  ( -0.6634819590976430703, 105.9515744484354371, -5.309451348557705508 ) ) ;
#29594 = CARTESIAN_POINT ( 'NONE',  ( 4.478158499223182432, 118.1173218799454077, 0.7357564059813932467 ) ) ;
#29595 = CARTESIAN_POINT ( 'NONE',  ( -46.98785713747574277, 25.41845405000909253, -0.7790854875835228066 ) ) ;
#29596 = CARTESIAN_POINT ( 'NONE',  ( -4.636268038904913347, 155.9604050671876792, -1.079575001969328873 ) ) ;
#29597 = CARTESIAN_POINT ( 'NONE',  ( -3.040433582521969047, 115.7029506960217731, -1.666328479974650945 ) ) ;
#29598 = CARTESIAN_POINT ( 'NONE',  ( -3.174366308152012373, 78.32546620154573702, -0.06343139340882732180 ) ) ;
#29599 = CARTESIAN_POINT ( 'NONE',  ( 0.8750585742502747788, 105.9515744484354371, -5.278707647178442208 ) ) ;
#29600 = CARTESIAN_POINT ( 'NONE',  ( -3.490201360801296726, 120.2313485970928326, -0.6717870626964185243 ) ) ;
#29601 = DIRECTION ( 'NONE',  ( 1.776356839400250465E-15, 0.000000000000000000, 1.000000000000000000 ) ) ;
#29602 = CARTESIAN_POINT ( 'NONE',  ( -0.006534791579925431325, 156.3267223255430167, 0.3270276925529296275 ) ) ;
#29603 = CARTESIAN_POINT ( 'NONE',  ( -4.825036788391023457, 63.33946620154573282, -0.09641571798141691796 ) ) ;
#29604 = CARTESIAN_POINT ( 'NONE',  ( -15.76299236085137956, 145.9019260673938163, -0.1804967559267895705 ) ) ;
#29605 = CARTESIAN_POINT ( 'NONE',  ( -0.2095918955067871126, -8.989892990265463624, -4.636818132431064221 ) ) ;
#29606 = CARTESIAN_POINT ( 'NONE',  ( 14.89898862929382517, 156.1361208441215922, 1.045442070961571934 ) ) ;
#29607 = CARTESIAN_POINT ( 'NONE',  ( 4.722078295102365431, 104.6144662015457527, -1.046302231095662671 ) ) ;
#29608 = CARTESIAN_POINT ( 'NONE',  ( 3.096790694169950342, -14.35231825047024401, 1.054797312298405121 ) ) ;
#29609 = CARTESIAN_POINT ( 'NONE',  ( -8.556073751109543934, 120.5511696877957775, 1.121754095281913610 ) ) ;
#29610 = CARTESIAN_POINT ( 'NONE',  ( 0.5118484794875378663, 4.451237885527871363, -0.8280682483750020362 ) ) ;
#29611 = CARTESIAN_POINT ( 'NONE',  ( -5.820459347748656143, 117.1115750087645608, -0.4818200784724923635 ) ) ;
#29612 = CARTESIAN_POINT ( 'NONE',  ( -0.2306771026100957467, -3.802149480603859377, 0.9475509996518236555 ) ) ;
#29613 = VERTEX_POINT ( 'NONE', #38408 ) ;
#29614 = ORIENTED_EDGE ( 'NONE', *, *, #30969, .F. ) ;
#29615 = CARTESIAN_POINT ( 'NONE',  ( -46.29506748884626433, 20.38262349295737152, 4.279265904994557168 ) ) ;
#29616 = CARTESIAN_POINT ( 'NONE',  ( 3.549733929829893331, 110.1236525333376619, 3.577684766704721575 ) ) ;
#29617 = DIRECTION ( 'NONE',  ( -0.9999768187992256196, 0.006808954705446186584, -1.145073529768427012E-18 ) ) ;
#29618 = CARTESIAN_POINT ( 'NONE',  ( -9.647033449255159709, 123.8920215319950842, 0.4922632944252962606 ) ) ;
#29619 = CARTESIAN_POINT ( 'NONE',  ( 3.866302502687585907, -14.02971062843458228, 4.478402296968817531 ) ) ;
#29620 = CARTESIAN_POINT ( 'NONE',  ( 1.409223554827445213, 119.7856413326322667, -0.5222593444346081970 ) ) ;
#29621 = CARTESIAN_POINT ( 'NONE',  ( -1.216597929035328374, 118.5604221528582372, -0.6894197161374837624 ) ) ;
#29622 = CARTESIAN_POINT ( 'NONE',  ( -9.960492004070040650, 64.81807050032566053, -1.269999999999996021 ) ) ;
#29623 = CARTESIAN_POINT ( 'NONE',  ( 3.205191379615736746, -14.47393913169138102, 3.051678166811226500 ) ) ;
#29624 = CARTESIAN_POINT ( 'NONE',  ( -5.652088634484938368, 31.23120021444162475, -0.6296991705779479975 ) ) ;
#29625 = CARTESIAN_POINT ( 'NONE',  ( 0.6395209782508930463, 120.9735524437166561, -0.05055770394172658805 ) ) ;
#29626 = VERTEX_POINT ( 'NONE', #5825 ) ;
#29627 = CARTESIAN_POINT ( 'NONE',  ( -3.155498692175132458, 108.3452252202363724, 4.146548619333099595 ) ) ;
#29628 = FACE_OUTER_BOUND ( 'NONE', #41887, .T. ) ;
#29629 = EDGE_CURVE ( 'NONE', #40015, #2780, #36888, .T. ) ;
#29630 = CARTESIAN_POINT ( 'NONE',  ( -5.019283203953386341, 117.3993836733805693, 0.7004435676391351784 ) ) ;
#29631 = CARTESIAN_POINT ( 'NONE',  ( 9.807059279559947385, 117.9968303279965340, 0.1034500883390726267 ) ) ;
#29632 = CARTESIAN_POINT ( 'NONE',  ( -5.270289556066668268, 116.2365830367532595, 0.9655167061512666127 ) ) ;
#29633 = CARTESIAN_POINT ( 'NONE',  ( -0.4045686510384880474, 118.1564795008688407, 0.9043423984889817913 ) ) ;
#29634 = CARTESIAN_POINT ( 'NONE',  ( -5.008552712180506461, 117.3993836135855560, 0.7755994290793736257 ) ) ;
#29635 = CARTESIAN_POINT ( 'NONE',  ( 2.241275201495271929, 37.45550410866057689, -1.120274590453292030 ) ) ;
#29636 = CARTESIAN_POINT ( 'NONE',  ( 6.881618033700585890, 158.0090104422344268, 1.782742279240755678 ) ) ;
#29637 = VECTOR ( 'NONE', #32320, 1000.000000000000114 ) ;
#29638 = CARTESIAN_POINT ( 'NONE',  ( 1.653223041919489544, 21.06826514481450729, 4.324967054831568625 ) ) ;
#29639 = CARTESIAN_POINT ( 'NONE',  ( 7.747546812250076798, -14.76477644359806973, -3.309085904616556384 ) ) ;
#29640 = CARTESIAN_POINT ( 'NONE',  ( -5.484865810345498360, 117.1958023522216337, -0.7988316295375470499 ) ) ;
#29641 = CARTESIAN_POINT ( 'NONE',  ( -1.417747896749580017, 115.2915405621345144, -1.855271064302983053 ) ) ;
#29642 = CYLINDRICAL_SURFACE ( 'NONE', #38815, 0.2540000000000027236 ) ;
#29643 = CARTESIAN_POINT ( 'NONE',  ( -10.28897677580358128, 56.51499999999998636, -5.016500000000000625 ) ) ;
#29644 = CARTESIAN_POINT ( 'NONE',  ( 2.144155271412940156, 104.6144662015412905, 4.896541268869996522 ) ) ;
#29645 = CARTESIAN_POINT ( 'NONE',  ( -1.471791394198959102, 24.03230288535706549, 4.399545648925609065 ) ) ;
#29646 = CARTESIAN_POINT ( 'NONE',  ( -8.095114962461808616, 74.19100168833409725, -1.269999999999996687 ) ) ;
#29647 = DIRECTION ( 'NONE',  ( 0.7284927773988636446, 0.6850534820564666560, -1.946650227582177166E-16 ) ) ;
#29648 = CARTESIAN_POINT ( 'NONE',  ( 2.917951099372082080, -14.56804730652265434, 4.441407531948645904 ) ) ;
#29649 = CARTESIAN_POINT ( 'NONE',  ( 1.667199326422575512, 119.8612358676174949, -0.5251152081720655840 ) ) ;
#29650 = CARTESIAN_POINT ( 'NONE',  ( -17.93297959639536288, 125.1504969321615164, 0.5028613125471301792 ) ) ;
#29651 = CARTESIAN_POINT ( 'NONE',  ( 4.801298031305056391, 117.4006795940419892, -1.015947262250491478 ) ) ;
#29652 = ORIENTED_EDGE ( 'NONE', *, *, #32611, .T. ) ;
#29653 = FACE_OUTER_BOUND ( 'NONE', #34335, .T. ) ;
#29654 = VERTEX_POINT ( 'NONE', #18781 ) ;
#29655 = CARTESIAN_POINT ( 'NONE',  ( 5.552702978602249040, -15.16724029374752547, 2.010675452401557095 ) ) ;
#29656 = CARTESIAN_POINT ( 'NONE',  ( -19.62644950592621385, 149.4594839399872512, 1.701416438606882187 ) ) ;
#29657 = CARTESIAN_POINT ( 'NONE',  ( 14.62453491845899833, 121.8773232776577942, -0.9418922607927827650 ) ) ;
#29658 = CARTESIAN_POINT ( 'NONE',  ( -4.515506726787251068, -6.291224493951820484, 1.111903093310195212 ) ) ;
#29659 = LINE ( 'NONE', #3905, #42007 ) ;
#29660 = ORIENTED_EDGE ( 'NONE', *, *, #27961, .T. ) ;
#29661 = FACE_OUTER_BOUND ( 'NONE', #20989, .T. ) ;
#29662 = CARTESIAN_POINT ( 'NONE',  ( 0.7406220848564354364, 119.3684187487962305, 0.7644009012486649990 ) ) ;
#29663 = CARTESIAN_POINT ( 'NONE',  ( -3.430652046320729731, 156.3978305292817481, 1.152991164011112568 ) ) ;
#29664 = DIRECTION ( 'NONE',  ( 1.000000000000000000, -5.463695987328526437E-16, -0.000000000000000000 ) ) ;
#29665 =( BOUNDED_CURVE ( )  B_SPLINE_CURVE ( 3, ( #30203, #4244, #14008, #40023 ),
 .UNSPECIFIED., .F., .T. ) 
 B_SPLINE_CURVE_WITH_KNOTS ( ( 4, 4 ),
 ( 3.750906500318049286, 4.712388980384690562 ),
 .UNSPECIFIED. ) 
 CURVE ( )  GEOMETRIC_REPRESENTATION_ITEM ( )  RATIONAL_B_SPLINE_CURVE ( ( 1.000000000000000000, 0.9244349266169029633, 0.9244349266169029633, 1.000000000000000000 ) ) 
 REPRESENTATION_ITEM ( '' )  );
#29666 = CARTESIAN_POINT ( 'NONE',  ( 17.48755558824488787, 140.3598469681121514, -1.687825538285184557 ) ) ;
#29667 = CARTESIAN_POINT ( 'NONE',  ( -20.88630183647693173, 148.3608207065297222, -2.399927473325582650 ) ) ;
#29668 = CARTESIAN_POINT ( 'NONE',  ( -58.75009580408200094, 0.1057190229620807997, -0.6617493214611014363 ) ) ;
#29669 = ORIENTED_EDGE ( 'NONE', *, *, #19359, .T. ) ;
#29670 = CARTESIAN_POINT ( 'NONE',  ( 4.478503255188988952, 118.1112075284179923, -0.5788684376435218049 ) ) ;
#29671 = CARTESIAN_POINT ( 'NONE',  ( 1.553919893302579958, 120.7289827521893670, -0.2132023499116272869 ) ) ;
#29672 = ORIENTED_EDGE ( 'NONE', *, *, #35773, .F. ) ;
#29673 = CARTESIAN_POINT ( 'NONE',  ( -2.063908814988777873, 157.0334531201187644, -1.539797002863052988 ) ) ;
#29674 = CARTESIAN_POINT ( 'NONE',  ( 1.977593594988821479, -15.25598227308876176, 5.283756247048868815 ) ) ;
#29675 = FACE_OUTER_BOUND ( 'NONE', #29879, .T. ) ;
#29676 = CARTESIAN_POINT ( 'NONE',  ( -58.33068375617610002, -0.2093732065610448556, 0.2478323015012930397 ) ) ;
#29677 = CARTESIAN_POINT ( 'NONE',  ( 1.100877510726109954, 5.750359496286542971, -4.487862572965156005 ) ) ;
#29678 = CARTESIAN_POINT ( 'NONE',  ( 3.458815983099534197, 120.0787590019544098, 0.7189451402107608358 ) ) ;
#29679 = CARTESIAN_POINT ( 'NONE',  ( -3.151918684035726947, 30.94949030248789867, -0.3028545185056354394 ) ) ;
#29680 = CARTESIAN_POINT ( 'NONE',  ( -3.789191232057584902, 13.46218022696137773, 2.646434746401360893 ) ) ;
#29681 = CARTESIAN_POINT ( 'NONE',  ( 11.10900461081871704, 128.0707465396788507, 0.3225556591789271454 ) ) ;
#29682 = CARTESIAN_POINT ( 'NONE',  ( -10.28897677580358305, 56.51499999999998636, 5.016500000000000625 ) ) ;
#29683 = CARTESIAN_POINT ( 'NONE',  ( -55.66968704194594153, 5.419822863896792242, -2.567922718055084541 ) ) ;
#29684 = CARTESIAN_POINT ( 'NONE',  ( 2.184895159611915716, 116.1856596408759970, 0.02067325796152543957 ) ) ;
#29685 = CARTESIAN_POINT ( 'NONE',  ( 22.46755768833288158, 150.8526571111528654, 0.4489552724284878171 ) ) ;
#29686 = CARTESIAN_POINT ( 'NONE',  ( -46.70678165893853162, 25.97453801526106787, -1.349345659034532074 ) ) ;
#29687 = FACE_OUTER_BOUND ( 'NONE', #31798, .T. ) ;
#29688 = FACE_OUTER_BOUND ( 'NONE', #2885, .T. ) ;
#29689 = CARTESIAN_POINT ( 'NONE',  ( 10.92199999999999704, 55.24500000000000455, 3.904382278571533962E-15 ) ) ;
#29690 = FACE_OUTER_BOUND ( 'NONE', #9679, .T. ) ;
#29691 = CARTESIAN_POINT ( 'NONE',  ( -6.654617103318593247E-14, 104.6144662015457243, 1.534725424433578570E-31 ) ) ;
#29692 = CARTESIAN_POINT ( 'NONE',  ( -57.78866059769681129, 2.451738602565561642, 1.593934435026631347 ) ) ;
#29693 = AXIS2_PLACEMENT_3D ( 'NONE', #3683, #33702, #1326 ) ;
#29694 = CARTESIAN_POINT ( 'NONE',  ( -58.55221842960730783, 0.5754175076986972615, 0.9757793345693576148 ) ) ;
#29695 = CARTESIAN_POINT ( 'NONE',  ( -20.30088961563517458, 128.9598305440861452, -0.1271185223121272523 ) ) ;
#29696 = ORIENTED_EDGE ( 'NONE', *, *, #23992, .T. ) ;
#29697 = CARTESIAN_POINT ( 'NONE',  ( -50.94572941386617515, 18.90544291192138004, -2.223209376321594100 ) ) ;
#29698 = CARTESIAN_POINT ( 'NONE',  ( -7.793677643169202973, 122.5633063490366084, -0.3701003583587130774 ) ) ;
#29699 = ORIENTED_EDGE ( 'NONE', *, *, #8405, .T. ) ;
#29700 = DIRECTION ( 'NONE',  ( -0.6294287539884059202, -0.7770581983690814099, -1.945484789722797322E-16 ) ) ;
#29701 = CARTESIAN_POINT ( 'NONE',  ( -10.40089755570045149, 153.1126597504080280, -0.2539288847195827481 ) ) ;
#29702 = CARTESIAN_POINT ( 'NONE',  ( 2.112423120037338453, -15.42067558999450583, 5.959086572354191702 ) ) ;
#29703 = CARTESIAN_POINT ( 'NONE',  ( -7.037849409249396615, 158.0922581832940921, 1.451942896407524497 ) ) ;
#29704 = CARTESIAN_POINT ( 'NONE',  ( 2.889066315880882030, 25.55657059589919911, 3.609430016826872478 ) ) ;
#29705 = CARTESIAN_POINT ( 'NONE',  ( 3.269635511691603380, 159.4655167044000166, 0.2664280249078423424 ) ) ;
#29706 = FACE_OUTER_BOUND ( 'NONE', #28413, .T. ) ;
#29707 = CARTESIAN_POINT ( 'NONE',  ( -29.48469873830907417, 60.47150940315087553, 1.269999999999993356 ) ) ;
#29708 = CARTESIAN_POINT ( 'NONE',  ( 0.9436028068379492817, -1.428137797730904879, 0.2459283266283248115 ) ) ;
#29709 = CARTESIAN_POINT ( 'NONE',  ( -3.288660796955225951, 159.4686222989141697, -0.1587487428767532793 ) ) ;
#29710 = CARTESIAN_POINT ( 'NONE',  ( 5.664977208693820820, 57.14999999999999858, -5.033228321271210781 ) ) ;
#29711 = CYLINDRICAL_SURFACE ( 'NONE', #28841, 0.2539999999999956737 ) ;
#29712 = CARTESIAN_POINT ( 'NONE',  ( -2.264966102306270379, 116.3304222186488772, 0.1531678969014962921 ) ) ;
#29713 = ORIENTED_EDGE ( 'NONE', *, *, #15168, .T. ) ;
#29714 = CARTESIAN_POINT ( 'NONE',  ( -3.856066505249651222, 156.9018388488748883, 1.546468145409084061 ) ) ;
#29715 = CARTESIAN_POINT ( 'NONE',  ( -58.06266446028805461, 0.3686289127265512389, -0.7729225178788856621 ) ) ;
#29716 = CARTESIAN_POINT ( 'NONE',  ( 13.04750228320297367, 121.1598417376693533, 1.575122625318853053 ) ) ;
#29717 = CARTESIAN_POINT ( 'NONE',  ( 12.38900849369184520, 122.4057692182592092, -1.312116060471626211 ) ) ;
#29718 = CARTESIAN_POINT ( 'NONE',  ( -0.7897743334665792148, -0.9462621144725560374, 0.5691593732151654095 ) ) ;
#29719 = CARTESIAN_POINT ( 'NONE',  ( -7.361208496634311871, 158.3992165788449711, -1.430753602065345076 ) ) ;
#29720 = AXIS2_PLACEMENT_3D ( 'NONE', #25780, #22568, #6006 ) ;
#29721 = CARTESIAN_POINT ( 'NONE',  ( 4.618524016831645262, 118.0632027795112862, -0.5485634799004409645 ) ) ;
#29722 = CARTESIAN_POINT ( 'NONE',  ( -6.606344270946872901E-14, 95.34346620154573770, 1.014423412895214384E-29 ) ) ;
#29723 = CARTESIAN_POINT ( 'NONE',  ( 16.07945855365731092, 143.8376908863262997, -0.9680047772055856425 ) ) ;
#29724 = CARTESIAN_POINT ( 'NONE',  ( -1.617373050801775625, 120.9968702744464366, -0.03231896268895501773 ) ) ;
#29725 = ORIENTED_EDGE ( 'NONE', *, *, #39925, .T. ) ;
#29726 = CARTESIAN_POINT ( 'NONE',  ( -5.834672723501299174, 119.9178398404649926, -1.129903066036337833 ) ) ;
#29727 = CARTESIAN_POINT ( 'NONE',  ( 5.310739065812000170, -15.29705283487872691, 0.1354967992945097788 ) ) ;
#29728 = AXIS2_PLACEMENT_3D ( 'NONE', #17819, #30819, #15255 ) ;
#29729 = CARTESIAN_POINT ( 'NONE',  ( -12.21488373879589240, 55.24499999999999034, 4.381499999999999950 ) ) ;
#29730 = CARTESIAN_POINT ( 'NONE',  ( -4.542182964463529871, 118.0343140766884034, -0.8604455232648324792 ) ) ;
#29731 = ADVANCED_FACE ( 'NONE', ( #15590 ), #9219, .F. ) ;
#29732 = CARTESIAN_POINT ( 'NONE',  ( -44.96292901393739072, 21.56701576681934540, -3.486870777078513228 ) ) ;
#29733 = VECTOR ( 'NONE', #40962, 1000.000000000000000 ) ;
#29734 = CARTESIAN_POINT ( 'NONE',  ( -5.177913976931290740, 56.99702125087954130, -5.372099999999995212 ) ) ;
#29735 = CARTESIAN_POINT ( 'NONE',  ( 16.01586142131289492, 150.9843922791743296, 2.313278988710850914 ) ) ;
#29736 = CARTESIAN_POINT ( 'NONE',  ( -5.208855653336853742, 31.38455280743060527, -0.6720767434146609487 ) ) ;
#29737 = CARTESIAN_POINT ( 'NONE',  ( 3.302029177305205732, 159.4671159221996959, 0.06598240135525389183 ) ) ;
#29738 = CARTESIAN_POINT ( 'NONE',  ( -4.036547470782467784, 117.2022048034790487, 0.8857695023546175994 ) ) ;
#29739 = CARTESIAN_POINT ( 'NONE',  ( 7.747546812250076798, -14.76477644359806973, -3.309085904616556384 ) ) ;
#29740 = CARTESIAN_POINT ( 'NONE',  ( 12.37067103324079476, 130.6617397222824479, 0.9131297178954279614 ) ) ;
#29741 = ADVANCED_FACE ( 'NONE', ( #15797 ), #9417, .F. ) ;
#29742 = CARTESIAN_POINT ( 'NONE',  ( 14.14567801931314328, 120.5239346615589540, -0.5295366371686059948 ) ) ;
#29743 = CARTESIAN_POINT ( 'NONE',  ( 5.327964288879288191, 105.1224761950569331, -0.2707926473889318286 ) ) ;
#29744 = EDGE_LOOP ( 'NONE', ( #29508, #971, #7574, #41867 ) ) ;
#29745 = CARTESIAN_POINT ( 'NONE',  ( 5.535770207902783291, -15.30306967536979457, -0.4932718738389492708 ) ) ;
#29746 = TOROIDAL_SURFACE ( 'NONE', #21535, 8.794749999999998735, 0.2540000000000000036 ) ;
#29747 = CARTESIAN_POINT ( 'NONE',  ( -15.54847974360328067, 120.7212560704218589, -0.2938029371637448928 ) ) ;
#29748 = VERTEX_POINT ( 'NONE', #27957 ) ;
#29749 = EDGE_CURVE ( 'NONE', #15081, #21468, #40965, .T. ) ;
#29750 = CARTESIAN_POINT ( 'NONE',  ( -6.728599971069020746, 121.0446882272744489, -0.9798701814483349315 ) ) ;
#29751 = CARTESIAN_POINT ( 'NONE',  ( -46.72577905453591285, 25.95655153957431338, -1.270000040519894347 ) ) ;
#29752 = CARTESIAN_POINT ( 'NONE',  ( -15.44350913713192064, 147.8441550597069352, -0.7585189891071871804 ) ) ;
#29753 = CARTESIAN_POINT ( 'NONE',  ( 3.873131646279637241, -11.92617534808754165, 0.9134907789774980857 ) ) ;
#29754 = CARTESIAN_POINT ( 'NONE',  ( -20.10769848529519166, 132.0867704272472452, 0.9164310550120231547 ) ) ;
#29755 = CARTESIAN_POINT ( 'NONE',  ( -41.28107547821698375, 23.22158991241121129, 1.523999999999985366 ) ) ;
#29756 = CARTESIAN_POINT ( 'NONE',  ( 10.82257311662882948, 157.9086237439880733, 0.2761350859956696047 ) ) ;
#29757 = ORIENTED_EDGE ( 'NONE', *, *, #36023, .F. ) ;
#29758 = CARTESIAN_POINT ( 'NONE',  ( 4.574821423538755205, -2.080616851812391310, 0.6590154617212384824 ) ) ;
#29759 = ADVANCED_FACE ( 'NONE', ( #39664 ), #38813, .F. ) ;
#29760 = FACE_OUTER_BOUND ( 'NONE', #3572, .T. ) ;
#29761 = CARTESIAN_POINT ( 'NONE',  ( -41.28107547821692691, 23.22158991241129300, -1.523999999999999355 ) ) ;
#29762 = DIRECTION ( 'NONE',  ( 1.000000000000000000, -9.627370216492862708E-17, 0.000000000000000000 ) ) ;
#29763 = CIRCLE ( 'NONE', #5962, 5.080000000000006288 ) ;
#29764 = CARTESIAN_POINT ( 'NONE',  ( -8.106797866231710614, 121.1670163920446157, 0.9708022562603837446 ) ) ;
#29765 = EDGE_CURVE ( 'NONE', #4305, #21064, #30755, .T. ) ;
#29766 = CARTESIAN_POINT ( 'NONE',  ( -3.632229383214316876, 17.08265688572556584, -2.901706292871565562 ) ) ;
#29767 = CARTESIAN_POINT ( 'NONE',  ( 14.69745991766241033, 121.6338672040446767, 1.430666218478179763 ) ) ;
#29768 = CARTESIAN_POINT ( 'NONE',  ( 15.70103477329399766, 145.5797129992483292, 0.3137440411564567100 ) ) ;
#29770 = CARTESIAN_POINT ( 'NONE',  ( 17.34031924846174988, 128.5728276651957742, -1.378292450406111147 ) ) ;
#29769 = LINE ( 'NONE', #26352, #39269 ) ;
#29771 = CARTESIAN_POINT ( 'NONE',  ( 2.901706292870370518, -4.507343114274551255, -3.632229383212865592 ) ) ;
#29772 = CARTESIAN_POINT ( 'NONE',  ( -18.04579964447635376, 154.0913862843578670, -1.474566393615006632 ) ) ;
#29773 = ORIENTED_EDGE ( 'NONE', *, *, #11795, .T. ) ;
#29774 = ORIENTED_EDGE ( 'NONE', *, *, #28421, .T. ) ;
#29775 = CARTESIAN_POINT ( 'NONE',  ( -0.004910621514806326471, 156.3161161488371533, 0.2457475809811482670 ) ) ;
#29776 = CARTESIAN_POINT ( 'NONE',  ( 6.098373624802439608, -13.52034412102339012, 1.767782016118699895 ) ) ;
#29777 = DIRECTION ( 'NONE',  ( 5.188838149069472160E-16, -1.699382548006136559E-16, -1.000000000000000000 ) ) ;
#29778 = AXIS2_PLACEMENT_3D ( 'NONE', #21993, #24561, #37565 ) ;
#29779 = CARTESIAN_POINT ( 'NONE',  ( 3.212496809824684441, -14.25148094350509353, 2.370051959060230473 ) ) ;
#29780 = ORIENTED_EDGE ( 'NONE', *, *, #38069, .T. ) ;
#29781 = CARTESIAN_POINT ( 'NONE',  ( 6.675970744194591688, 119.4737997143703012, 1.289985488916530310 ) ) ;
#29782 = CARTESIAN_POINT ( 'NONE',  ( -9.094996104468895837, 78.64197151092922411, 5.392902600000138769 ) ) ;
#29783 = CARTESIAN_POINT ( 'NONE',  ( 14.91798719394653894, 12.51401280605345789, 0.000000000000000000 ) ) ;
#29784 = CARTESIAN_POINT ( 'NONE',  ( -7.717559979892335775, 158.5863655655865330, 0.7470610436598877913 ) ) ;
#29785 = CARTESIAN_POINT ( 'NONE',  ( -6.181412921142831252, 19.34218365691531361, 5.729511908899769246 ) ) ;
#29786 = CARTESIAN_POINT ( 'NONE',  ( 9.210551279805565983, 123.0263237342149978, 1.033454686166954239 ) ) ;
#29787 = CARTESIAN_POINT ( 'NONE',  ( 10.74909004363686194, 157.9381345072164038, -0.1376009798949087704 ) ) ;
#29788 = CARTESIAN_POINT ( 'NONE',  ( 11.41714695485569919, 57.15000000000000568, -5.016500000000000625 ) ) ;
#29789 = CARTESIAN_POINT ( 'NONE',  ( -48.52081263401391453, 18.50387112158377789, 5.159775967924278284 ) ) ;
#29790 = CARTESIAN_POINT ( 'NONE',  ( -48.57235503434458224, 24.64055110436136431, 0.2038152558994842933 ) ) ;
#29791 = CARTESIAN_POINT ( 'NONE',  ( -3.403764228135175429, 117.9394517900196888, 1.153273866709463302 ) ) ;
#29792 = CARTESIAN_POINT ( 'NONE',  ( -52.42133349025997546, 11.92692459785933679, 4.172736198742178715 ) ) ;
#29793 = CARTESIAN_POINT ( 'NONE',  ( -57.27125839519965922, 2.624645228885598147, 1.995972916280581710 ) ) ;
#29794 = CARTESIAN_POINT ( 'NONE',  ( -4.415952317727478871, 118.1645917943391169, 0.4804988017228924990 ) ) ;
#29795 = CARTESIAN_POINT ( 'NONE',  ( -5.177913976931298734, 78.94499979771843812, -5.372100000000003206 ) ) ;
#29796 = ADVANCED_FACE ( 'NONE', ( #6653 ), #19617, .F. ) ;
#29797 = EDGE_LOOP ( 'NONE', ( #1958, #14872, #28699, #40099 ) ) ;
#29798 = CARTESIAN_POINT ( 'NONE',  ( -3.946513987435433357, 118.7629491485454309, -1.103369079102947348 ) ) ;
#29800 = EDGE_CURVE ( 'NONE', #29525, #22768, #1531, .T. ) ;
#29799 = CARTESIAN_POINT ( 'NONE',  ( -6.098125870537236537, 119.5354672635397719, -1.256037220562212786 ) ) ;
#29801 = CARTESIAN_POINT ( 'NONE',  ( -5.349033702192389050, 117.2069880336854197, -0.8964318704791015557 ) ) ;
#29802 = CARTESIAN_POINT ( 'NONE',  ( 4.503537194581884506, 118.0666071354895053, 0.8214503418453174000 ) ) ;
#29803 = CARTESIAN_POINT ( 'NONE',  ( 0.005430166084267442142, 120.5648899400503069, -0.2717477157510628794 ) ) ;
#29804 = PRESENTATION_LAYER_ASSIGNMENT (  '', '', ( #6014 ) ) ;
#29805 = CARTESIAN_POINT ( 'NONE',  ( -0.6068508678446015159, 115.7030933504832149, -1.759829434126405356 ) ) ;
#29806 = CARTESIAN_POINT ( 'NONE',  ( 3.341374452869265710, 118.1651003929687960, -0.6417180735543650538 ) ) ;
#29807 = FACE_OUTER_BOUND ( 'NONE', #37844, .T. ) ;
#29808 = CARTESIAN_POINT ( 'NONE',  ( -16.88761465400188300, 147.3835828867039766, -1.922606999130501260 ) ) ;
#29809 = CARTESIAN_POINT ( 'NONE',  ( -0.003550357976012296669, 159.5989787797044812, 0.1776744311461875836 ) ) ;
#29810 = CARTESIAN_POINT ( 'NONE',  ( 7.886551735269857311, 122.1946728851203261, -0.4945421293698765153 ) ) ;
#29811 = CARTESIAN_POINT ( 'NONE',  ( -8.982416536893675030, 124.0550639507465291, -0.09049447817662507887 ) ) ;
#29812 = EDGE_CURVE ( 'NONE', #34762, #14687, #25213, .T. ) ;
#29813 = CARTESIAN_POINT ( 'NONE',  ( -3.416230376366909294, -5.529048218071860532, 3.121479803864907865 ) ) ;
#29814 = CARTESIAN_POINT ( 'NONE',  ( 3.159869787290094933, 159.3937097445585778, 0.6918644357365444364 ) ) ;
#29815 = CARTESIAN_POINT ( 'NONE',  ( 4.780953720317446809, 104.6144662015457669, -0.7304112483795474065 ) ) ;
#29816 = CARTESIAN_POINT ( 'NONE',  ( 3.275654002680270960, -14.73162568742410272, 0.7099577593494145189 ) ) ;
#29817 = CARTESIAN_POINT ( 'NONE',  ( -14.75721126660351601, 152.8628051715174365, 1.735400109512247102 ) ) ;
#29818 = CARTESIAN_POINT ( 'NONE',  ( -0.9353260110528880400, 8.126651709021682990, 0.2714574413461035007 ) ) ;
#29819 = CARTESIAN_POINT ( 'NONE',  ( -18.48423909989039871, 154.1703991122031994, -0.9245180971295517969 ) ) ;
#29820 = EDGE_CURVE ( 'NONE', #32583, #1712, #33899, .T. ) ;
#29821 = CARTESIAN_POINT ( 'NONE',  ( 0.4636875340052978300, -8.988401195314681402, -0.8615772474383697199 ) ) ;
#29822 = ORIENTED_EDGE ( 'NONE', *, *, #33529, .T. ) ;
#29823 = CARTESIAN_POINT ( 'NONE',  ( -47.44699234454018466, 15.94620872345373108, -6.997593760898217036E-15 ) ) ;
#29824 = CARTESIAN_POINT ( 'NONE',  ( 0.6634819590975142845, 105.9515744484354371, 5.309451348557705508 ) ) ;
#29825 = CARTESIAN_POINT ( 'NONE',  ( -16.15477348297523719, 145.8839827664328368, 0.6502963436359734395 ) ) ;
#29826 = CARTESIAN_POINT ( 'NONE',  ( 2.954207113090831616, -14.52495373116942368, 5.111795949899043734 ) ) ;
#29827 = CARTESIAN_POINT ( 'NONE',  ( 17.48603724727278674, 147.5992144370567871, -1.461888717290057871 ) ) ;
#29828 = CARTESIAN_POINT ( 'NONE',  ( -12.32670121879468716, 122.4057692182592092, -1.805994760647165354 ) ) ;
#29829 = ADVANCED_FACE ( 'NONE', ( #16855 ), #19415, .F. ) ;
#29830 = CARTESIAN_POINT ( 'NONE',  ( 0.09871621325710944195, 104.6144662015456674, 4.835249534204173472 ) ) ;
#29831 = CARTESIAN_POINT ( 'NONE',  ( 3.176652145978316355, -13.92691374863060183, 2.072386176210903486 ) ) ;
#29832 = CARTESIAN_POINT ( 'NONE',  ( -4.916573287661055502, 117.5420315621613554, -1.049119472579290058 ) ) ;
#29833 = CARTESIAN_POINT ( 'NONE',  ( 8.883181220021160840, 123.7004864364556909, 0.02116515827996235527 ) ) ;
#29834 = ORIENTED_EDGE ( 'NONE', *, *, #35443, .T. ) ;
#29835 = CARTESIAN_POINT ( 'NONE',  ( -5.114121277772293084, 113.8198996839817454, 1.623722780927329135 ) ) ;
#29836 = CARTESIAN_POINT ( 'NONE',  ( 1.769790122373364527, 106.3931338143381424, 5.031734874205501029 ) ) ;
#29837 = DIRECTION ( 'NONE',  ( -1.000000000000000000, 0.000000000000000000, 0.000000000000000000 ) ) ;
#29838 = CARTESIAN_POINT ( 'NONE',  ( 23.28495812418880462, 149.3453998935430604, 0.3112269551726871697 ) ) ;
#29839 = CIRCLE ( 'NONE', #613, 5.080000000000006288 ) ;
#29840 = CARTESIAN_POINT ( 'NONE',  ( -4.861212978143241159, 112.7561542417671916, 2.378900599183503051 ) ) ;
#29841 = VECTOR ( 'NONE', #25668, 1000.000000000000000 ) ;
#29842 = CARTESIAN_POINT ( 'NONE',  ( -2.015348138122511568, 118.7629491485454167, 1.152895576627283925 ) ) ;
#29843 = CARTESIAN_POINT ( 'NONE',  ( 11.97180806971946865, 56.20439414706014958, 5.016499999999999737 ) ) ;
#29844 = CARTESIAN_POINT ( 'NONE',  ( 2.014642110472020242, 39.20946620154573026, -1.229996183391246944 ) ) ;
#29845 = CARTESIAN_POINT ( 'NONE',  ( 13.38228307180514776, 122.0388263298542739, 1.742221313037096486 ) ) ;
#29846 = CARTESIAN_POINT ( 'NONE',  ( -2.133573495637306916, 19.78131850274109382, 4.120466288703205748 ) ) ;
#29847 = CARTESIAN_POINT ( 'NONE',  ( -5.323917895073306816, 23.39377214425099893, 6.572471397932490689 ) ) ;
#29848 = CARTESIAN_POINT ( 'NONE',  ( 8.658313298994691820, 118.4528737239894269, -0.7179955298477456171 ) ) ;
#29849 = CARTESIAN_POINT ( 'NONE',  ( -2.900991945634804114, 122.3314979878274045, -0.2533474610292539841 ) ) ;
#29850 = CARTESIAN_POINT ( 'NONE',  ( -6.059261036834082681, 78.87450423423038615, 5.016499999999999737 ) ) ;
#29851 = DIRECTION ( 'NONE',  ( -0.8745520943968229099, 0.4849315768086573386, -4.268512490100424221E-16 ) ) ;
#29852 = CARTESIAN_POINT ( 'NONE',  ( -4.540852303063954487, 104.6144662015457243, 1.644315252756900714 ) ) ;
#29853 = CARTESIAN_POINT ( 'NONE',  ( 1.893578447776079754, 19.08455809737888487, -4.224370802633358402 ) ) ;
#29854 = DIRECTION ( 'NONE',  ( -6.353134868986659519E-16, 1.000000000000000000, -0.000000000000000000 ) ) ;
#29855 = CARTESIAN_POINT ( 'NONE',  ( -4.757346424997288103, 117.3993836135861386, -1.207075064218979810 ) ) ;
#29856 = CARTESIAN_POINT ( 'NONE',  ( 2.576299636888586875, -14.89815494326314571, 4.769281578164155100 ) ) ;
#29857 = CARTESIAN_POINT ( 'NONE',  ( 2.330098105383510809, 118.9955205646042344, -0.6366692849230544127 ) ) ;
#29858 = CARTESIAN_POINT ( 'NONE',  ( -13.10540794497634565, 156.9444350391594014, 0.5617278846626186928 ) ) ;
#29859 = DIRECTION ( 'NONE',  ( 0.7548010569845216011, 0.6559537821943318692, 2.801824109679581255E-16 ) ) ;
#29860 = ORIENTED_EDGE ( 'NONE', *, *, #30470, .T. ) ;
#29861 = CARTESIAN_POINT ( 'NONE',  ( -5.578816284158369498, 56.51500000000002188, 4.418322536902429043 ) ) ;
#29862 = ORIENTED_EDGE ( 'NONE', *, *, #27378, .F. ) ;
#29863 = CARTESIAN_POINT ( 'NONE',  ( 17.14500000000001023, 57.15000000000000568, 4.381499999999999950 ) ) ;
#29864 = CARTESIAN_POINT ( 'NONE',  ( 3.308369008328103433, -15.71782228035249673, 4.479361047165574483 ) ) ;
#29865 = CARTESIAN_POINT ( 'NONE',  ( -18.88973499030882763, 150.3568762430427910, 1.706130117709411476 ) ) ;
#29866 = CARTESIAN_POINT ( 'NONE',  ( 14.39412078427922914, 121.9874158357064857, -1.026313471838276481 ) ) ;
#29867 = EDGE_CURVE ( 'NONE', #23250, #9160, #3463, .T. ) ;
#29868 = CARTESIAN_POINT ( 'NONE',  ( 4.636249899789679496, -11.37698174978397958, -0.2454043791197063895 ) ) ;
#29869 = DIRECTION ( 'NONE',  ( -5.206863593109713661E-17, 1.000000000000000000, -1.077750396879097183E-30 ) ) ;
#29870 = VERTEX_POINT ( 'NONE', #16427 ) ;
#29871 = CARTESIAN_POINT ( 'NONE',  ( 2.958531772299236362, 39.20946620154573736, 1.329372033065076453 ) ) ;
#29872 = CARTESIAN_POINT ( 'NONE',  ( 0.7524737301089851060, 120.0979018405971175, 0.6085003676253140092 ) ) ;
#29873 = CARTESIAN_POINT ( 'NONE',  ( -13.78713281179563666, 131.0408573235120571, 1.173264656791310756 ) ) ;
#29874 = CARTESIAN_POINT ( 'NONE',  ( -4.856515155028523267, 117.4075056128946386, -1.171047894592366356 ) ) ;
#29875 = CIRCLE ( 'NONE', #4715, 2.540000000000000480 ) ;
#29876 = CARTESIAN_POINT ( 'NONE',  ( 17.21863486588922143, 149.7102054596878702, -1.666570748255499002 ) ) ;
#29877 = CARTESIAN_POINT ( 'NONE',  ( -12.61233984701559407, 121.4495935343099688, -1.683034450629873557 ) ) ;
#29878 = CARTESIAN_POINT ( 'NONE',  ( -6.045080874924777230E-14, 85.18346620154574111, 1.015827583860198862E-16 ) ) ;
#29879 = EDGE_LOOP ( 'NONE', ( #6289, #32739, #34960, #10100 ) ) ;
#29880 = CARTESIAN_POINT ( 'NONE',  ( 4.476806822841735034, 118.1289215581870877, -0.5424833475171277897 ) ) ;
#29881 = CARTESIAN_POINT ( 'NONE',  ( 6.226794683659739427, 155.3658059236344684, -0.5518929715360436639 ) ) ;
#29882 = ORIENTED_EDGE ( 'NONE', *, *, #37318, .F. ) ;
#29883 = CARTESIAN_POINT ( 'NONE',  ( 3.248418650160624033, -14.57852055173261618, 2.075358651653527620 ) ) ;
#29884 = CARTESIAN_POINT ( 'NONE',  ( 3.794317479684171879, 105.1231002567820241, -3.763369276752646098 ) ) ;
#29885 = CARTESIAN_POINT ( 'NONE',  ( -51.89660998226325006, 12.88425699701002003, 4.274492870955763912 ) ) ;
#29886 = CARTESIAN_POINT ( 'NONE',  ( 2.198398128136354934, 2.077049112184502278, 4.064154346441791965 ) ) ;
#29887 = CARTESIAN_POINT ( 'NONE',  ( 16.92358334414607768, 148.6336825499269310, 2.141768463193927996 ) ) ;
#29888 = CARTESIAN_POINT ( 'NONE',  ( -2.941155235503680743, 30.72646416932365909, -0.2232678871262771536 ) ) ;
#29889 = CARTESIAN_POINT ( 'NONE',  ( 3.874746376330849618, 18.20996518813934628, -2.522041008920607563 ) ) ;
#29890 = CARTESIAN_POINT ( 'NONE',  ( 15.53993717541241359, 147.5346097818530211, 0.5395553097850843693 ) ) ;
#29891 = CARTESIAN_POINT ( 'NONE',  ( -0.3821431882137919511, 105.7852416002251204, 5.327472155929901199 ) ) ;
#29892 = CIRCLE ( 'NONE', #3387, 8.794749999999995183 ) ;
#29893 = CARTESIAN_POINT ( 'NONE',  ( -55.65298819915649631, 5.540485941798498182, -2.823722248809265256 ) ) ;
#29894 = AXIS2_PLACEMENT_3D ( 'NONE', #32159, #6185, #35991 ) ;
#29895 = CARTESIAN_POINT ( 'NONE',  ( -2.175382718649831126, 116.2302060928067675, -0.1775962133206757110 ) ) ;
#29896 = CARTESIAN_POINT ( 'NONE',  ( 3.682264917456191888, 104.1064662015457287, 0.07358041635424013294 ) ) ;
#29897 = LINE ( 'NONE', #36506, #29526 ) ;
#29898 = LINE ( 'NONE', #26909, #977 ) ;
#29899 = CARTESIAN_POINT ( 'NONE',  ( -30.84292043869464095, 55.46612528701088962, -1.524000000001431099 ) ) ;
#29900 = B_SPLINE_CURVE_WITH_KNOTS ( 'NONE', 3,
 ( #39663, #34320, #8744, #17896, #21292, #1738, #21706, #5774, #28333, #5148, #18103, #34528, #2582, #24491, #18728, #27702 ),
 .UNSPECIFIED., .F., .F.,
 ( 4, 2, 1, 1, 2, 2, 2, 2, 4 ),
 ( 0.000000000000000000, 0.06250000000000000000, 0.1250000000000000000, 0.2500000000000000000, 0.5000000000000000000, 0.6250000000000000000, 0.7500000000000000000, 0.8750000000000000000, 1.000000000000000000 ),
 .UNSPECIFIED. ) ;
#29901 = CARTESIAN_POINT ( 'NONE',  ( -26.51793118801306548, 72.98537704160715123, -1.524000000000006017 ) ) ;
#29902 = DIRECTION ( 'NONE',  ( -0.9998004120163608288, 0.000000000000000000, -0.01997839162482749342 ) ) ;
#29903 = CARTESIAN_POINT ( 'NONE',  ( -58.75091225067960465, 0.1325880516401256592, 0.03773457465073216249 ) ) ;
#29904 = CARTESIAN_POINT ( 'NONE',  ( -57.15088083682995546, 2.378576142695001838, 1.865916551128045553 ) ) ;
#29905 = CARTESIAN_POINT ( 'NONE',  ( -8.004298179822360026, 158.6817341734954425, 0.1651967042931135332 ) ) ;
#29906 = VERTEX_POINT ( 'NONE', #32845 ) ;
#29907 = CARTESIAN_POINT ( 'NONE',  ( -56.13924587166188473, 7.155854391526911051, -1.290439134121123432 ) ) ;
#29908 = CARTESIAN_POINT ( 'NONE',  ( -6.973042344651466884, 121.9479208601376286, -0.2102655371621303393 ) ) ;
#29909 = VERTEX_POINT ( 'NONE', #272 ) ;
#29910 = CARTESIAN_POINT ( 'NONE',  ( -5.332935381406168851, 115.7029491485442634, -0.1065653510733624160 ) ) ;
#29911 = CARTESIAN_POINT ( 'NONE',  ( -14.17736129766413100, 138.8817910697950140, -0.3341079978015792928 ) ) ;
#29912 = CARTESIAN_POINT ( 'NONE',  ( 6.471342906213767066, -13.19865009487615559, 0.2853922585125314715 ) ) ;
#29913 = CARTESIAN_POINT ( 'NONE',  ( -21.19479858968374941, 149.1058327099893290, 1.460163390594825028 ) ) ;
#29914 = DIRECTION ( 'NONE',  ( -4.017660918040594346E-17, 1.000000000000000000, 2.376309959284834438E-19 ) ) ;
#29915 = CARTESIAN_POINT ( 'NONE',  ( -0.003550357976009695018, 159.5989787797044812, 0.1776744311461876391 ) ) ;
#29916 = CARTESIAN_POINT ( 'NONE',  ( 9.053714358506876891, 124.2128128113216121, 0.3155815647710615846 ) ) ;
#29917 = CARTESIAN_POINT ( 'NONE',  ( 2.163044864548389956, 28.58015952483584954, -4.087059112497700042 ) ) ;
#29918 = CARTESIAN_POINT ( 'NONE',  ( -0.3362158861861603287, -7.698726726604804504, -0.9163890413163552351 ) ) ;
#29919 = CARTESIAN_POINT ( 'NONE',  ( 0.003550357975880899172, 159.5989787797044812, -0.1776744311461874171 ) ) ;
#29920 = CARTESIAN_POINT ( 'NONE',  ( -48.51966762233396935, 18.52674309225730198, -5.186066996718803779 ) ) ;
#29921 = CARTESIAN_POINT ( 'NONE',  ( -6.135835944515187101, 77.40800365160224317, -1.269999999999996243 ) ) ;
#29922 = VERTEX_POINT ( 'NONE', #29215 ) ;
#29923 = CARTESIAN_POINT ( 'NONE',  ( 2.196830523109587929, 116.2217898966666638, 0.1075589129066046312 ) ) ;
#29924 = CARTESIAN_POINT ( 'NONE',  ( -2.165411683282754574, 157.1282018749678002, 1.500011447693321287 ) ) ;
#29925 = CARTESIAN_POINT ( 'NONE',  ( -57.89986051506333098, 0.7216312584049938694, -0.9866875624993080018 ) ) ;
#29926 = CARTESIAN_POINT ( 'NONE',  ( 4.923251988582125982, 158.4862278396301178, 1.623903838676621580 ) ) ;
#29927 = CARTESIAN_POINT ( 'NONE',  ( 14.84283187390155589, 125.6006210965460781, -1.448481940162723136 ) ) ;
#29928 = CARTESIAN_POINT ( 'NONE',  ( 0.7725151586569730666, -15.29989167607388900, -0.5872501270430795506 ) ) ;
#29929 = CARTESIAN_POINT ( 'NONE',  ( 0.02156508032615568615, 159.2730288250082538, -1.079204802879467406 ) ) ;
#29930 = CARTESIAN_POINT ( 'NONE',  ( 4.656685402655694972, 118.0313236345014758, -0.5883047702015815617 ) ) ;
#29931 = AXIS2_PLACEMENT_3D ( 'NONE', #15465, #9300, #35286 ) ;
#29932 = CARTESIAN_POINT ( 'NONE',  ( 16.33516936551314558, 148.1602266505728380, -1.109112510451941702 ) ) ;
#29933 = CARTESIAN_POINT ( 'NONE',  ( -7.552512487614272629, 122.4261604937442485, -0.1509171734833087142 ) ) ;
#29934 = ORIENTED_EDGE ( 'NONE', *, *, #9933, .T. ) ;
#29935 = CARTESIAN_POINT ( 'NONE',  ( -12.63334184343655586, 124.0847267554996591, -1.843480660383216563 ) ) ;
#29936 = CARTESIAN_POINT ( 'NONE',  ( 4.901850132730561249, -15.30225767492697564, -0.5056678198325348372 ) ) ;
#29937 = DIRECTION ( 'NONE',  ( -1.000000000000000000, 1.288607544181256449E-16, 0.000000000000000000 ) ) ;
#29938 = CARTESIAN_POINT ( 'NONE',  ( -4.642601932456255298, 117.9634981682017383, -0.9174702582142799656 ) ) ;
#29939 = CARTESIAN_POINT ( 'NONE',  ( -49.39021242113546606, 17.77731941784099234, -5.290631085210052653 ) ) ;
#29940 = CARTESIAN_POINT ( 'NONE',  ( 4.105367864036007397, 118.2429491485453354, 0.3529617804329867603 ) ) ;
#29941 = CARTESIAN_POINT ( 'NONE',  ( 12.85862358090719404, 153.8477531742089468, 2.225956515383983092 ) ) ;
#29942 = DIRECTION ( 'NONE',  ( -0.8745520943968235761, 0.4849315768086558398, -5.691349986800547879E-16 ) ) ;
#29943 = CARTESIAN_POINT ( 'NONE',  ( 8.217147260422391852, 117.5004391570743394, 0.1493243188240319652 ) ) ;
#29944 = CARTESIAN_POINT ( 'NONE',  ( 5.540715274600516160, 6.338079305180906786, 6.343128766557815545 ) ) ;
#29945 = CARTESIAN_POINT ( 'NONE',  ( 9.627236290563381260, 124.2480737032941533, 0.7173579674491836755 ) ) ;
#29946 = CARTESIAN_POINT ( 'NONE',  ( 9.536130858165876134, 118.4542681464805298, -0.5810392422064987183 ) ) ;
#29947 = EDGE_CURVE ( 'NONE', #5326, #16499, #2366, .T. ) ;
#29948 = CARTESIAN_POINT ( 'NONE',  ( -42.19606231239111338, 22.08888036620076889, -1.545000424059316924 ) ) ;
#29949 = ORIENTED_EDGE ( 'NONE', *, *, #8453, .F. ) ;
#29950 = CARTESIAN_POINT ( 'NONE',  ( 0.7729263974008259153, 115.6909491485452719, 1.757288066092038914 ) ) ;
#29951 = CARTESIAN_POINT ( 'NONE',  ( -2.757293845589700698, 116.5489981622532127, 0.01971897987843778538 ) ) ;
#29952 = EDGE_LOOP ( 'NONE', ( #21076, #39262, #41206, #28189, #4788 ) ) ;
#29953 = CARTESIAN_POINT ( 'NONE',  ( 5.365375985982141493, 120.5163311419836134, -0.5829208649569685985 ) ) ;
#29954 = CARTESIAN_POINT ( 'NONE',  ( -8.675687895398477067, 118.3610464811752081, 0.6699752535086661576 ) ) ;
#29955 = CARTESIAN_POINT ( 'NONE',  ( 0.003052472355820575779, 120.8426702770480148, -0.1527581987772197447 ) ) ;
#29956 = CARTESIAN_POINT ( 'NONE',  ( 4.137648320759505616, -13.26899632091267733, 3.249298663494996298 ) ) ;
#29957 = CARTESIAN_POINT ( 'NONE',  ( -22.12005076447816876, 142.1041199125429557, 1.010629163944517739 ) ) ;
#29958 = CARTESIAN_POINT ( 'NONE',  ( -27.97106122948731155, 77.87043919753004673, -1.270000000000007345 ) ) ;
#29959 = CARTESIAN_POINT ( 'NONE',  ( 0.8904708500336536714, 116.4394364983335493, 0.05634004476769405995 ) ) ;
#29960 = EDGE_CURVE ( 'NONE', #2316, #16908, #36219, .T. ) ;
#29961 = ORIENTED_EDGE ( 'NONE', *, *, #15150, .F. ) ;
#29962 = CARTESIAN_POINT ( 'NONE',  ( 4.224370802630715183, -2.505441902618962935, 1.893578447770203566 ) ) ;
#29963 = CARTESIAN_POINT ( 'NONE',  ( 5.326133827267389265, 105.1224662015456772, 0.4469431379364897094 ) ) ;
#29964 = DIRECTION ( 'NONE',  ( 0.9998004120163608288, 0.000000000000000000, 0.01997839162482762526 ) ) ;
#29965 = DIRECTION ( 'NONE',  ( 0.1469470846586743706, 0.000000000000000000, 0.9891443546370348727 ) ) ;
#29966 = CARTESIAN_POINT ( 'NONE',  ( 8.032877371522001653, 121.3111410846650244, 1.249454745935258071 ) ) ;
#29967 = CARTESIAN_POINT ( 'NONE',  ( -4.449009123739010363, -11.09185097514761331, -1.246716907482375847 ) ) ;
#29968 = CARTESIAN_POINT ( 'NONE',  ( 22.31562366552497068, 146.3189071340513294, 1.902122558187540280 ) ) ;
#29969 = CARTESIAN_POINT ( 'NONE',  ( -55.81791661756539469, 5.217579515133088819, -2.786573170153239243 ) ) ;
#29971 = CARTESIAN_POINT ( 'NONE',  ( 11.66006228966214486, 156.3395478113760362, -1.582478695429108129 ) ) ;
#29970 = DIRECTION ( 'NONE',  ( -0.8745520943968245753, 0.4849315768086539524, -5.691349986800526185E-16 ) ) ;
#29972 = CARTESIAN_POINT ( 'NONE',  ( -1.290833045837797455, 0.8901568857254957834, 4.466177308409287505 ) ) ;
#29973 = CARTESIAN_POINT ( 'NONE',  ( -20.52999062792650165, 132.2049894596293313, -1.489094535601872993 ) ) ;
#29974 = TOROIDAL_SURFACE ( 'NONE', #37444, 0.3809999999999999498, 0.2540000000000000036 ) ;
#29975 = ORIENTED_EDGE ( 'NONE', *, *, #27204, .F. ) ;
#29976 = CARTESIAN_POINT ( 'NONE',  ( -0.6667004703452847902, 156.3175253132196190, 0.2457982560305636555 ) ) ;
#29977 = CARTESIAN_POINT ( 'NONE',  ( 5.913917015499376539, -14.05268412609835060, 2.470677959447274308 ) ) ;
#29978 = VECTOR ( 'NONE', #8095, 1000.000000000000000 ) ;
#29979 = CARTESIAN_POINT ( 'NONE',  ( -44.21430376968325504, 21.24218795319830022, 2.931160726117570725 ) ) ;
#29980 = B_SPLINE_CURVE_WITH_KNOTS ( 'NONE', 3,
 ( #36510, #1156, #24128, #30945, #21129, #11141 ),
 .UNSPECIFIED., .F., .F.,
 ( 4, 2, 4 ),
 ( 0.000000000000000000, 0.5000000000000000000, 0.5009815572441199683 ),
 .UNSPECIFIED. ) ;
#29981 = CARTESIAN_POINT ( 'NONE',  ( 1.589478822742971683E-15, 16.51000000000000156, 0.000000000000000000 ) ) ;
#29982 = VERTEX_POINT ( 'NONE', #485 ) ;
#29983 = CARTESIAN_POINT ( 'NONE',  ( 12.11054887026057081, 155.0146010091537221, 2.232606363771872715 ) ) ;
#29984 = CARTESIAN_POINT ( 'NONE',  ( -4.883848590450072358, 117.7607009110569862, 0.7127853619805604168 ) ) ;
#29985 = DIRECTION ( 'NONE',  ( -5.188838149069471174E-16, 1.699382548006136313E-16, 1.000000000000000000 ) ) ;
#29986 = CARTESIAN_POINT ( 'NONE',  ( -22.60445334873329415, 148.5212373274837319, 0.8566365145943201087 ) ) ;
#29988 = ADVANCED_FACE ( 'NONE', ( #7078 ), #33060, .F. ) ;
#29987 = CARTESIAN_POINT ( 'NONE',  ( 6.778223571145144177, 14.38247674671404752, -5.057098040585858989 ) ) ;
#29989 = CARTESIAN_POINT ( 'NONE',  ( 10.17133788503921110, 124.0743415861677903, 1.120692231141951156 ) ) ;
#29990 = FACE_OUTER_BOUND ( 'NONE', #34748, .T. ) ;
#29991 = CARTESIAN_POINT ( 'NONE',  ( 15.13173320725175763, 120.7387302883610118, -0.2100629019518969742 ) ) ;
#29992 = CYLINDRICAL_SURFACE ( 'NONE', #32172, 7.461249999999999716 ) ;
#29993 = CARTESIAN_POINT ( 'NONE',  ( -57.93112410002309787, 0.6539490773164662318, 0.9478910564283531404 ) ) ;
#29994 = CARTESIAN_POINT ( 'NONE',  ( -49.15418877470109749, 24.05022684412165646, 0.2550087576077032514 ) ) ;
#29995 = AXIS2_PLACEMENT_3D ( 'NONE', #32440, #35227, #25425 ) ;
#29996 = CARTESIAN_POINT ( 'NONE',  ( 2.483772768628635497, 106.8193809087893271, -4.725234424128872845 ) ) ;
#29997 = CARTESIAN_POINT ( 'NONE',  ( -56.82628769568140115, 4.502340570254503405, 2.499646007873237430 ) ) ;
#29998 = CARTESIAN_POINT ( 'NONE',  ( -56.63941872605137462, 3.954178040575838882, 2.419973308390618527 ) ) ;
#29999 = CARTESIAN_POINT ( 'NONE',  ( -4.459999047083514689, 118.1598764511204536, 0.4313593223247962349 ) ) ;
#30000 = DIRECTION ( 'NONE',  ( -5.188838149069472160E-16, 1.699382548006136559E-16, 1.000000000000000000 ) ) ;
#30001 = PRODUCT ( 'Corkscrew Body', 'Corkscrew Body', '', ( #32814 ) ) ;
#30002 = ORIENTED_EDGE ( 'NONE', *, *, #21370, .T. ) ;
#30003 = CARTESIAN_POINT ( 'NONE',  ( -41.18107378286554621, 22.95619949144852967, 1.523999999999987143 ) ) ;
#30004 = CARTESIAN_POINT ( 'NONE',  ( -3.682509200627861468, 118.8507421139248379, -0.9352261960797142448 ) ) ;
#30005 = CARTESIAN_POINT ( 'NONE',  ( -4.381926848744128300, 111.2539628214143903, -3.135495374750700392 ) ) ;
#30007 = CARTESIAN_POINT ( 'NONE',  ( 4.451861420862569751, 118.1112095268316011, 0.7573049349207229275 ) ) ;
#30006 = VECTOR ( 'NONE', #9147, 1000.000000000000227 ) ;
#30008 = CARTESIAN_POINT ( 'NONE',  ( -0.5945828676176249106, 120.5739061664170606, -0.2962085107056580680 ) ) ;
#30009 = CARTESIAN_POINT ( 'NONE',  ( -1.214571177347494313, 115.7029375466994736, -1.741462126173494385 ) ) ;
#30010 = CARTESIAN_POINT ( 'NONE',  ( 1.005691866306313464, 118.1651004085809831, -0.8396654685810295282 ) ) ;
#30011 = CARTESIAN_POINT ( 'NONE',  ( 5.434281097240408087, 117.1681999988027911, -0.6838767007579789059 ) ) ;
#30012 = CARTESIAN_POINT ( 'NONE',  ( -5.844382469225037902, 120.7327493588883840, -0.8888191899821258346 ) ) ;
#30013 = CARTESIAN_POINT ( 'NONE',  ( 15.50061618130081165, 62.14374591690594940, 1.904999999999990035 ) ) ;
#30014 = CARTESIAN_POINT ( 'NONE',  ( -0.002459401150367294953, 159.6023738651833810, 0.1230784904792620454 ) ) ;
#30015 = CARTESIAN_POINT ( 'NONE',  ( 8.348968351561811829, 120.0002459142761921, -1.116349756213213640 ) ) ;
#30016 = CARTESIAN_POINT ( 'NONE',  ( -4.205176885578073787, 155.8715900735512605, 0.01157140856383978393 ) ) ;
#30017 = CARTESIAN_POINT ( 'NONE',  ( 5.008145224984434485, 117.3993836135855418, -0.7758584094373792706 ) ) ;
#30018 = CARTESIAN_POINT ( 'NONE',  ( 10.49915001570426476, 157.9057380314836223, 0.9855651801815568103 ) ) ;
#30019 = CARTESIAN_POINT ( 'NONE',  ( 5.177913976931216133, 53.58606249999999704, -5.372100000000000541 ) ) ;
#30020 = CARTESIAN_POINT ( 'NONE',  ( 2.678036876842718517, -15.12020262989130437, 4.533791366373512766 ) ) ;
#30021 = CARTESIAN_POINT ( 'NONE',  ( -12.95103886519486558, 123.9867020804889961, 1.362965731555215054 ) ) ;
#30022 = CARTESIAN_POINT ( 'NONE',  ( -0.4041098725243945644, -13.24273492701920141, -0.8882236940730178221 ) ) ;
#30023 = CARTESIAN_POINT ( 'NONE',  ( -16.70755423740151713, 155.2649736186859570, -0.8698744534657079086 ) ) ;
#30024 = CARTESIAN_POINT ( 'NONE',  ( -0.5845540250341307864, -7.254922367050685494, -0.7839501960785225654 ) ) ;
#30025 = VERTEX_POINT ( 'NONE', #32215 ) ;
#30026 = ADVANCED_FACE ( 'NONE', ( #34111 ), #41663, .T. ) ;
#30027 = CARTESIAN_POINT ( 'NONE',  ( -47.25474348537468927, 18.41641806589853303, 3.087470713317412851 ) ) ;
#30028 = CARTESIAN_POINT ( 'NONE',  ( 3.975629016401896809, 111.5999093057820772, 3.028662833142258037 ) ) ;
#30029 = CARTESIAN_POINT ( 'NONE',  ( -5.210205730215736963, 121.0352659167314755, 0.3424523703800272934 ) ) ;
#30030 = CARTESIAN_POINT ( 'NONE',  ( 2.939725130288969979, -14.94165859211278580, 5.651657094137466864 ) ) ;
#30031 = CARTESIAN_POINT ( 'NONE',  ( 17.81274246965180197, 147.0764175921665640, -1.531068679518140518 ) ) ;
#30032 = CARTESIAN_POINT ( 'NONE',  ( -15.73670139478164387, 128.5598958631237565, -2.193363351549679319 ) ) ;
#30033 = CARTESIAN_POINT ( 'NONE',  ( -2.049604525191627502, 104.6144662015457243, 4.378607431551252205 ) ) ;
#30034 = AXIS2_PLACEMENT_3D ( 'NONE', #19635, #3487, #38213 ) ;
#30035 = CARTESIAN_POINT ( 'NONE',  ( 3.162791966164926638, -14.44121541014482801, 3.416220915275241854 ) ) ;
#30036 = CARTESIAN_POINT ( 'NONE',  ( -4.784543075752243801, 117.4060574113812265, -1.200192385861798883 ) ) ;
#30037 = CARTESIAN_POINT ( 'NONE',  ( 9.177823364990439714, 124.0935018032023436, 0.02293427522457985521 ) ) ;
#30038 = EDGE_LOOP ( 'NONE', ( #34557, #11207, #14896, #6679 ) ) ;
#30039 = ADVANCED_FACE ( 'NONE', ( #37095 ), #36827, .F. ) ;
#30040 = EDGE_CURVE ( 'NONE', #2591, #17780, #6965, .T. ) ;
#30041 = CARTESIAN_POINT ( 'NONE',  ( -5.150313346575406293, 114.9389534560005472, 1.533160836946849459 ) ) ;
#30042 = CARTESIAN_POINT ( 'NONE',  ( 3.279000889525665485, 108.1634925278680868, 4.199033572238965561 ) ) ;
#30043 = AXIS2_PLACEMENT_3D ( 'NONE', #38063, #31668, #8880 ) ;
#30044 = CARTESIAN_POINT ( 'NONE',  ( 0.7701797417504300247, 117.3993836066060226, 1.486317275820449257 ) ) ;
#30045 = LINE ( 'NONE', #33255, #20496 ) ;
#30046 = CARTESIAN_POINT ( 'NONE',  ( 23.33610279681219879, 149.0590277239482475, 0.3121099645145855028 ) ) ;
#30047 = EDGE_CURVE ( 'NONE', #11064, #29909, #33511, .T. ) ;
#30048 = DIRECTION ( 'NONE',  ( -0.9336303900108815501, -0.3582377630124009560, -4.235673982319039874E-16 ) ) ;
#30049 = CIRCLE ( 'NONE', #21843, 0.6350000000000014522 ) ;
#30050 = EDGE_CURVE ( 'NONE', #17039, #22739, #41523, .T. ) ;
#30051 = CARTESIAN_POINT ( 'NONE',  ( 1.877814291165026628, -15.55177680042434041, 5.422881654991738465 ) ) ;
#30052 = DIRECTION ( 'NONE',  ( 5.188838149069472160E-16, -1.699382548006136559E-16, -1.000000000000000000 ) ) ;
#30053 = CARTESIAN_POINT ( 'NONE',  ( 7.783141725463699423, 119.0983413489662297, 1.312215641098252172 ) ) ;
#30054 = VERTEX_POINT ( 'NONE', #33695 ) ;
#30055 = CARTESIAN_POINT ( 'NONE',  ( 6.775881838314501415, 16.25650946394821617, 5.045332117489572887 ) ) ;
#30056 = CARTESIAN_POINT ( 'NONE',  ( -5.497210702263359394, 117.7329109126123967, -1.024491283099325356 ) ) ;
#30057 = CARTESIAN_POINT ( 'NONE',  ( -2.331513492273154853, 111.1666841684333633, -3.236375129800145967 ) ) ;
#30058 = CARTESIAN_POINT ( 'NONE',  ( -5.565035070531761718, 78.91452218770618288, 5.089667964246479492 ) ) ;
#30059 = CIRCLE ( 'NONE', #1504, 0.5080000000000000071 ) ;
#30060 = CARTESIAN_POINT ( 'NONE',  ( -2.565436166410399288, 107.6373832812085425, -4.562490956761092953 ) ) ;
#30061 = CARTESIAN_POINT ( 'NONE',  ( -4.815265214305837205, 105.1215022376130150, 2.303391734824050463 ) ) ;
#30062 = CIRCLE ( 'NONE', #10337, 1.000000000000000000 ) ;
#30063 = CARTESIAN_POINT ( 'NONE',  ( -3.426874451426485724, 1.805113900313119357, -3.130497002818263930 ) ) ;
#30064 = CARTESIAN_POINT ( 'NONE',  ( -4.416771755448872128, 71.99420641645033925, -1.523999999999994248 ) ) ;
#30065 = DIRECTION ( 'NONE',  ( -0.000000000000000000, -0.000000000000000000, 1.000000000000000000 ) ) ;
#30066 = CARTESIAN_POINT ( 'NONE',  ( 1.985452195540454934, -15.12483337350742296, 5.348831821476924375 ) ) ;
#30067 = CARTESIAN_POINT ( 'NONE',  ( 5.575611629171946859, 123.3023672762779910, 0.03632235649590544874 ) ) ;
#30068 = CARTESIAN_POINT ( 'NONE',  ( -22.99243123797629096, 146.5883926500602001, 0.5216133500896585895 ) ) ;
#30069 = EDGE_CURVE ( 'NONE', #3380, #5970, #14562, .T. ) ;
#30070 = CARTESIAN_POINT ( 'NONE',  ( -10.04123483169954234, 65.65183074430956367, 1.270000000000002904 ) ) ;
#30071 = DIRECTION ( 'NONE',  ( 0.7770581983690836303, -0.6294287539884032556, 5.101669463485833779E-16 ) ) ;
#30072 = ORIENTED_EDGE ( 'NONE', *, *, #30873, .F. ) ;
#30073 = CARTESIAN_POINT ( 'NONE',  ( -3.151918684035726947, 30.94949030248789157, -0.3028545185056354394 ) ) ;
#30074 = CARTESIAN_POINT ( 'NONE',  ( 5.204094786718133747, -15.42339607600888485, 1.288180339967581967 ) ) ;
#30075 = CARTESIAN_POINT ( 'NONE',  ( -7.743227489916900907, 119.4405053107883958, 1.058161572703685938 ) ) ;
#30076 = CARTESIAN_POINT ( 'NONE',  ( 4.349802767100347189, -10.92635770930747796, -1.576909098649299512 ) ) ;
#30077 = EDGE_LOOP ( 'NONE', ( #38666, #40993, #34886, #25659 ) ) ;
#30078 = DIRECTION ( 'NONE',  ( -0.8745520943968250194, 0.4849315768086532863, -5.361993529360574930E-16 ) ) ;
#30079 = CARTESIAN_POINT ( 'NONE',  ( 1.682799138809720096, 120.1914007830323214, 0.5335993566373052888 ) ) ;
#30080 = CARTESIAN_POINT ( 'NONE',  ( -1.968159265821259218, 156.7095495334699535, 1.232728320231047059 ) ) ;
#30081 = CARTESIAN_POINT ( 'NONE',  ( 0.3680926247507866900, 118.1564734711614904, 0.9197955535796807913 ) ) ;
#30082 = AXIS2_PLACEMENT_3D ( 'NONE', #8795, #35002, #2417 ) ;
#30083 = CARTESIAN_POINT ( 'NONE',  ( 8.398523874639428399, 120.8878392079396065, -1.065324388190682647 ) ) ;
#30084 = CARTESIAN_POINT ( 'NONE',  ( -20.26628159282173414, 149.4216517587604756, -2.427422966980313124 ) ) ;
#30085 = DIRECTION ( 'NONE',  ( 5.188838149069472160E-16, -1.699382548006136559E-16, -1.000000000000000000 ) ) ;
#30086 = ORIENTED_EDGE ( 'NONE', *, *, #21990, .T. ) ;
#30087 = CARTESIAN_POINT ( 'NONE',  ( 4.118047298989734095, 118.2429491485453354, -0.1865688736171002005 ) ) ;
#30088 = EDGE_CURVE ( 'NONE', #30817, #36646, #2154, .T. ) ;
#30089 = CARTESIAN_POINT ( 'NONE',  ( 15.99593626731837048, 146.6619865182943272, -0.4079709740032105847 ) ) ;
#30090 = ORIENTED_EDGE ( 'NONE', *, *, #12295, .T. ) ;
#30091 = CARTESIAN_POINT ( 'NONE',  ( 3.065366080762625955, -14.95244456720379311, 3.762810261076596330 ) ) ;
#30092 = CARTESIAN_POINT ( 'NONE',  ( -1.828502361677136534, 105.1241263439060418, -5.020304316456576821 ) ) ;
#30093 = AXIS2_PLACEMENT_3D ( 'NONE', #31310, #18944, #34321 ) ;
#30094 = CARTESIAN_POINT ( 'NONE',  ( -50.51080154062190530, 15.37413104945128595, 4.759117110738762868 ) ) ;
#30095 = CARTESIAN_POINT ( 'NONE',  ( -4.623654898565560778, 8.549082320728111029, 0.09932813335659773646 ) ) ;
#30096 = CARTESIAN_POINT ( 'NONE',  ( 10.57849499609981514, 123.4307455932968765, 1.421577474458307400 ) ) ;
#30097 = CARTESIAN_POINT ( 'NONE',  ( 2.933835436169716537, 38.64483070579829871, -0.5563684569531323065 ) ) ;
#30098 = EDGE_CURVE ( 'NONE', #6334, #926, #19194, .T. ) ;
#30099 = CARTESIAN_POINT ( 'NONE',  ( -3.453265078539333288, 21.00871511114837276, -3.102408547967784092 ) ) ;
#30100 = CARTESIAN_POINT ( 'NONE',  ( 9.115475939616047185, 153.9201329141909866, 0.2944159349489394728 ) ) ;
#30101 = CYLINDRICAL_SURFACE ( 'NONE', #24953, 16.60960244842765832 ) ;
#30102 = VECTOR ( 'NONE', #42004, 1000.000000000000227 ) ;
#30103 = CARTESIAN_POINT ( 'NONE',  ( -55.69906247323991266, 5.207560852731635492, -2.143283491784350403 ) ) ;
#30104 = CARTESIAN_POINT ( 'NONE',  ( 2.170524884126211251, 116.2984658183265623, -0.1645159270875201085 ) ) ;
#30105 = CARTESIAN_POINT ( 'NONE',  ( -8.095114962461808616, 74.19100168833409725, 1.524000000000002686 ) ) ;
#30106 = DIRECTION ( 'NONE',  ( 5.188838149069472160E-16, -1.699382548006136559E-16, -1.000000000000000000 ) ) ;
#30107 = DIRECTION ( 'NONE',  ( -5.188838149069471174E-16, 1.699382548006136313E-16, 1.000000000000000000 ) ) ;
#30108 = CARTESIAN_POINT ( 'NONE',  ( -32.57812072122469260, 51.47121137444911199, -1.524000000004977373 ) ) ;
#30109 = CARTESIAN_POINT ( 'NONE',  ( 8.218723488459346527, -2.309819447571417772, 1.932697321913255717 ) ) ;
#30110 = CARTESIAN_POINT ( 'NONE',  ( -46.64075290549589425, 25.58044659150066735, 1.617434478680441767 ) ) ;
#30111 = DIRECTION ( 'NONE',  ( -0.8745520943968249084, 0.4849315768086533418, -5.271987356194193006E-16 ) ) ;
#30112 = CARTESIAN_POINT ( 'NONE',  ( -58.03428750496626520, 2.144022121626010247, -1.041663317983060951E-14 ) ) ;
#30113 = FACE_OUTER_BOUND ( 'NONE', #8551, .T. ) ;
#30114 = CARTESIAN_POINT ( 'NONE',  ( -1.406537315630193463, 159.5914066142653098, 0.2310332007158444334 ) ) ;
#30115 = ORIENTED_EDGE ( 'NONE', *, *, #32944, .T. ) ;
#30116 = CARTESIAN_POINT ( 'NONE',  ( -55.80532936045742787, 9.325833942462050885, -0.2199084463661266087 ) ) ;
#30117 = CARTESIAN_POINT ( 'NONE',  ( -7.788296088720038313, 122.5980079112661940, -0.2833033014985410492 ) ) ;
#30118 = ORIENTED_EDGE ( 'NONE', *, *, #8613, .T. ) ;
#30119 = CARTESIAN_POINT ( 'NONE',  ( 3.646513112444593752, 115.7029492782878037, -1.479418030874811052 ) ) ;
#30120 = CARTESIAN_POINT ( 'NONE',  ( -10.40832821182528001, 153.0987333575537548, -0.3246753324606910796 ) ) ;
#30121 = CARTESIAN_POINT ( 'NONE',  ( 6.419191409189793696, -13.32337952207179832, 0.5587850172365541601 ) ) ;
#30122 = CARTESIAN_POINT ( 'NONE',  ( -21.09608681602927760, 148.7375953542188256, 1.514114011542639693 ) ) ;
#30123 = CARTESIAN_POINT ( 'NONE',  ( -0.9950013725589796909, 29.65466048987409309, -4.513790593961638287 ) ) ;
#30124 = TOROIDAL_SURFACE ( 'NONE', #9719, 8.794749999999996959, 0.2540000000000000036 ) ;
#30125 = CARTESIAN_POINT ( 'NONE',  ( 20.61342602778648825, 152.5829384802601396, 0.8505107393516945224 ) ) ;
#30126 = CARTESIAN_POINT ( 'NONE',  ( 15.52406135986475277, 147.5381818669338827, 0.5105160171526207380 ) ) ;
#30127 = CARTESIAN_POINT ( 'NONE',  ( -29.24627908556541200, 62.62042691902884428, 1.269999999999994467 ) ) ;
#30128 = CARTESIAN_POINT ( 'NONE',  ( 0.8486417380921021936, -9.850041244260159701, -0.4793021190969105616 ) ) ;
#30129 = CARTESIAN_POINT ( 'NONE',  ( -15.16003043525278215, 156.1230782244120121, -0.5028385762316637253 ) ) ;
#30130 = DIRECTION ( 'NONE',  ( -0.9998004120163609398, 0.000000000000000000, -0.01997839162482749689 ) ) ;
#30131 = CARTESIAN_POINT ( 'NONE',  ( 4.756879258228443597, 117.4006795747281586, 1.206942419589918991 ) ) ;
#30132 = VERTEX_POINT ( 'NONE', #41764 ) ;
#30133 = CARTESIAN_POINT ( 'NONE',  ( 5.546876812502214982, 116.7824702235449621, 0.3920729990857263481 ) ) ;
#30134 = CARTESIAN_POINT ( 'NONE',  ( -5.507840079722835291, 156.5946142756450570, 1.582329182567088210 ) ) ;
#30135 = CARTESIAN_POINT ( 'NONE',  ( -57.92524306007030077, 0.6666591521451983304, -0.9550055539480221123 ) ) ;
#30136 = CARTESIAN_POINT ( 'NONE',  ( 12.12330053995811774, 120.5818589831333441, 1.513795679345424583 ) ) ;
#30137 = CARTESIAN_POINT ( 'NONE',  ( 19.45999741125991989, 148.3988719805327037, -1.735632530687203356 ) ) ;
#30138 = CARTESIAN_POINT ( 'NONE',  ( -0.8818152078519037040, -12.16566588317193265, -0.4137299969793124532 ) ) ;
#30139 = CARTESIAN_POINT ( 'NONE',  ( -5.844449987888692633, 118.2031694463412634, -1.045635565433329361 ) ) ;
#30140 = CARTESIAN_POINT ( 'NONE',  ( -43.87210973174860129, 22.05421410453335795, -2.454571855453439255 ) ) ;
#30141 = CIRCLE ( 'NONE', #21964, 0.2539999999999931202 ) ;
#30142 = CARTESIAN_POINT ( 'NONE',  ( 4.505160425060487306, 105.1215147309967080, 2.878549663133488590 ) ) ;
#30143 = CIRCLE ( 'NONE', #10398, 0.2539999999999973390 ) ;
#30144 = CARTESIAN_POINT ( 'NONE',  ( 8.566376370482780445, 122.4751019636825049, -0.6322842599711310241 ) ) ;
#30145 = CARTESIAN_POINT ( 'NONE',  ( -9.163388821854908883, 124.2347608867413413, -0.1831063163140473071 ) ) ;
#30146 = EDGE_LOOP ( 'NONE', ( #12554, #2359, #14711, #27403 ) ) ;
#30147 = CARTESIAN_POINT ( 'NONE',  ( -11.17842967653879249, 122.9575399027323073, -1.639653439019827186 ) ) ;
#30148 = CARTESIAN_POINT ( 'NONE',  ( 3.739721301978734314, -15.76301488427489517, 4.305968564470687987 ) ) ;
#30149 = CARTESIAN_POINT ( 'NONE',  ( -4.557225192774990497, 118.0384377347435958, -0.8496051783353677500 ) ) ;
#30150 = CARTESIAN_POINT ( 'NONE',  ( -49.93490050754573417, 16.96705409125581099, -5.170188367178254474 ) ) ;
#30151 = DIRECTION ( 'NONE',  ( 5.188838149069472160E-16, -1.699382548006136559E-16, -1.000000000000000000 ) ) ;
#30152 = CARTESIAN_POINT ( 'NONE',  ( 4.261081698622550817, 119.8084884740358547, 0.9035344350157261673 ) ) ;
#30153 = CARTESIAN_POINT ( 'NONE',  ( -7.994219716368544226, 68.36415334912796027, -1.523999999999995580 ) ) ;
#30154 = CIRCLE ( 'NONE', #13154, 14.73199999999999577 ) ;
#30155 = CARTESIAN_POINT ( 'NONE',  ( 6.896656464550490639, 117.1676486657671177, 0.1232935741316918549 ) ) ;
#30156 = CARTESIAN_POINT ( 'NONE',  ( 2.469379016249674486, 9.589258615745848147, -8.089366445887874235 ) ) ;
#30157 = CARTESIAN_POINT ( 'NONE',  ( 7.076231864619158429, 121.9239394581621809, 0.5528764260536548347 ) ) ;
#30158 = CARTESIAN_POINT ( 'NONE',  ( 14.01781138111942404, 120.5923583732999873, -0.6175494627556293858 ) ) ;
#30159 = CARTESIAN_POINT ( 'NONE',  ( -43.93237127071142822, 21.31409657049219675, -2.696834577195023286 ) ) ;
#30160 = CARTESIAN_POINT ( 'NONE',  ( 5.177913976931212581, 57.15000000000004832, -5.372100000000001430 ) ) ;
#30161 = CIRCLE ( 'NONE', #13164, 6.350000000000004974 ) ;
#30162 = CARTESIAN_POINT ( 'NONE',  ( -23.21350185287846912, 149.6290410902582551, -0.3868015801638792772 ) ) ;
#30163 = ORIENTED_EDGE ( 'NONE', *, *, #22929, .F. ) ;
#30164 = CARTESIAN_POINT ( 'NONE',  ( 8.121995431296815227, 121.0945329078791843, -0.9875153719367453231 ) ) ;
#30165 = CARTESIAN_POINT ( 'NONE',  ( -6.538176131568015962E-14, 82.13546620154573930, -1.207165459078370276E-19 ) ) ;
#30166 = ORIENTED_EDGE ( 'NONE', *, *, #2434, .T. ) ;
#30167 = DIRECTION ( 'NONE',  ( -1.000000000000000000, 1.140319995778305956E-16, 0.000000000000000000 ) ) ;
#30168 = CARTESIAN_POINT ( 'NONE',  ( -6.044022022451821741, 155.3491655920357459, -0.4731370799734935795 ) ) ;
#30169 = CARTESIAN_POINT ( 'NONE',  ( 4.970078376064472003, -11.71998231623441100, 0.7442660586517341192 ) ) ;
#30170 = CARTESIAN_POINT ( 'NONE',  ( -6.877630800715581749, 117.9658002137636856, 0.6876290806823444068 ) ) ;
#30171 = CARTESIAN_POINT ( 'NONE',  ( -46.38316532014830074, 26.05065462784526176, 1.523999999999997357 ) ) ;
#30172 = CARTESIAN_POINT ( 'NONE',  ( -0.0002734175339891707266, 159.6054662015457382, 0.01368293144939998138 ) ) ;
#30173 = VERTEX_POINT ( 'NONE', #5981 ) ;
#30174 = CARTESIAN_POINT ( 'NONE',  ( 1.686640475165922748, -9.627085671684914914, -4.319569293544198274 ) ) ;
#30175 = CARTESIAN_POINT ( 'NONE',  ( -23.44919332464161599, 146.8469795362756258, -0.4944523877934683953 ) ) ;
#30176 = CARTESIAN_POINT ( 'NONE',  ( -14.60499999999999865, 71.11999999999999034, 5.714999999999998970 ) ) ;
#30177 = CARTESIAN_POINT ( 'NONE',  ( -46.60530155212503445, 26.17382724835477958, -1.524000000000008459 ) ) ;
#30178 = VERTEX_POINT ( 'NONE', #31950 ) ;
#30179 = CARTESIAN_POINT ( 'NONE',  ( -8.304993556123838161, 120.2147940885562889, 1.117492704526953817 ) ) ;
#30180 = CARTESIAN_POINT ( 'NONE',  ( 0.8067276567327370529, -3.745225398377231674, -4.556403025205434609 ) ) ;
#30181 = CARTESIAN_POINT ( 'NONE',  ( 14.73734951358248857, 121.3346631531286164, 1.319546682830233797 ) ) ;
#30182 = CARTESIAN_POINT ( 'NONE',  ( -58.81784827865733689, -0.2724209480201578160, -0.09409996577202993373 ) ) ;
#30184 = CARTESIAN_POINT ( 'NONE',  ( 13.31748376333897532, 121.6721647909590303, -1.150164054616430453 ) ) ;
#30183 = DIRECTION ( 'NONE',  ( -0.9998004120163608288, 0.000000000000000000, -0.01997839162482749342 ) ) ;
#30185 = CARTESIAN_POINT ( 'NONE',  ( 4.628409624684510781, -5.919234854628785847, 0.1277143096542201761 ) ) ;
#30186 = CARTESIAN_POINT ( 'NONE',  ( -22.31420326625529782, 142.2114994846844240, -1.760598597564681622 ) ) ;
#30187 = ORIENTED_EDGE ( 'NONE', *, *, #30555, .T. ) ;
#30188 = CARTESIAN_POINT ( 'NONE',  ( -8.883181220021290514, 123.7004864364556909, -0.02116515827996221996 ) ) ;
#30189 = CARTESIAN_POINT ( 'NONE',  ( 5.719270376754757912, -14.62604927220606577, 2.811085246033490304 ) ) ;
#30190 = FACE_OUTER_BOUND ( 'NONE', #16881, .T. ) ;
#30191 = VECTOR ( 'NONE', #11081, 1000.000000000000000 ) ;
#30192 = CARTESIAN_POINT ( 'NONE',  ( -4.038290521723881810, 111.0900967538891564, -3.207870893326146167 ) ) ;
#30193 = ORIENTED_EDGE ( 'NONE', *, *, #34997, .F. ) ;
#30194 = CARTESIAN_POINT ( 'NONE',  ( 11.06681148537619563, 121.4866960210745503, 1.697623966824489683 ) ) ;
#30195 = CARTESIAN_POINT ( 'NONE',  ( 4.962772945303370875, 117.4661736183843317, 0.9732638675253090232 ) ) ;
#30196 = AXIS2_PLACEMENT_3D ( 'NONE', #26627, #4493, #10225 ) ;
#30197 = CARTESIAN_POINT ( 'NONE',  ( -32.58208212396117176, 51.46406716590541919, -1.270000000000005347 ) ) ;
#30198 = CARTESIAN_POINT ( 'NONE',  ( -0.01645572339173941370, 159.4324016994384010, 0.8235116888278194436 ) ) ;
#30199 = CARTESIAN_POINT ( 'NONE',  ( 7.912908961612729719, 12.87109176889305928, 2.878135455392844655 ) ) ;
#30200 = CARTESIAN_POINT ( 'NONE',  ( 16.40115699206375410, 147.1833543704171348, 1.602497317185074710 ) ) ;
#30201 = LINE ( 'NONE', #1041, #21269 ) ;
#30202 = CARTESIAN_POINT ( 'NONE',  ( 22.47739742037821031, 150.5824416163731314, -0.2728482117335694346 ) ) ;
#30203 = CARTESIAN_POINT ( 'NONE',  ( -14.39766717389552397, 60.02151067229126369, -1.904999999999999805 ) ) ;
#30204 = AXIS2_PLACEMENT_3D ( 'NONE', #8946, #18510, #2146 ) ;
#30205 = CARTESIAN_POINT ( 'NONE',  ( -57.59772826146109281, 1.374066163636324056, 1.306202371370214443 ) ) ;
#30206 = CARTESIAN_POINT ( 'NONE',  ( -48.05877817626803505, 25.10121868647436472, -8.674011749334489717E-15 ) ) ;
#30207 = CARTESIAN_POINT ( 'NONE',  ( -4.829600922136632946, 117.3993836135881423, 1.010428145333803540 ) ) ;
#30208 = CARTESIAN_POINT ( 'NONE',  ( -55.73247374733729487, 5.492406230130003841, 2.854677165782097514 ) ) ;
#30209 = CARTESIAN_POINT ( 'NONE',  ( -58.64175687851415830, -0.3079593361096647497, 0.3457559927878634531 ) ) ;
#30210 = CARTESIAN_POINT ( 'NONE',  ( -4.421375971199002386, 118.1651973794024855, 0.4750358156669655663 ) ) ;
#30211 = CARTESIAN_POINT ( 'NONE',  ( -3.630816577625875226E-14, 57.14999999999999147, 0.000000000000000000 ) ) ;
#30212 = ORIENTED_EDGE ( 'NONE', *, *, #2932, .F. ) ;
#30213 = CARTESIAN_POINT ( 'NONE',  ( -46.60530155212503445, 26.17382724835477958, 1.523999999999991140 ) ) ;
#30214 = CARTESIAN_POINT ( 'NONE',  ( 4.007742253885239414, 119.1179171808522312, -0.7639785333703686954 ) ) ;
#30215 = CARTESIAN_POINT ( 'NONE',  ( -7.613751273744924219, 124.2930771091975117, -0.1610855651276038303 ) ) ;
#30216 = CARTESIAN_POINT ( 'NONE',  ( 4.578501332539032909, 118.0757660871476986, 0.7069378206079117710 ) ) ;
#30217 = CARTESIAN_POINT ( 'NONE',  ( -16.29504633872605268, 146.4745453488731357, -1.441742819671184561 ) ) ;
#30218 = CARTESIAN_POINT ( 'NONE',  ( -0.7365778754629619396, 115.7029383710874839, -1.756171452946359013 ) ) ;
#30219 = CARTESIAN_POINT ( 'NONE',  ( -33.42971872652992005, 49.93539301574497102, 1.269999999999992690 ) ) ;
#30220 = CARTESIAN_POINT ( 'NONE',  ( 4.503688181905097565, 111.2539628214143903, -2.957939639849824331 ) ) ;
#30221 = CARTESIAN_POINT ( 'NONE',  ( -15.56955422694819902, 149.1167355181319181, -1.737459915651670128 ) ) ;
#30222 = FACE_OUTER_BOUND ( 'NONE', #35479, .T. ) ;
#30223 = FACE_OUTER_BOUND ( 'NONE', #29221, .T. ) ;
#30224 = DIRECTION ( 'NONE',  ( 0.7445787077807144438, 0.6675346791887304398, 0.000000000000000000 ) ) ;
#30225 = CARTESIAN_POINT ( 'NONE',  ( -0.001967380068485734355, 120.9974662015458620, 0.09845574358318300023 ) ) ;
#30226 = CARTESIAN_POINT ( 'NONE',  ( 4.529186081025091681, -11.15152372915077095, -0.9203776863585164669 ) ) ;
#30227 = CARTESIAN_POINT ( 'NONE',  ( 15.06876432237280206, 120.9194639129320734, 0.9861043747356995626 ) ) ;
#30228 = CARTESIAN_POINT ( 'NONE',  ( 5.241362157049035631, 77.01756249999996840, -5.310945289804168468 ) ) ;
#30229 = CARTESIAN_POINT ( 'NONE',  ( 2.368424984008928202, -15.31393412036581658, 4.927583237414308037 ) ) ;
#30230 = CARTESIAN_POINT ( 'NONE',  ( -17.82416131750972355, 140.4837523222294351, 1.726486987461786082 ) ) ;
#30231 = CARTESIAN_POINT ( 'NONE',  ( -0.8818152078519037040, -12.16566588317193265, -0.4137299969793124532 ) ) ;
#30232 = CARTESIAN_POINT ( 'NONE',  ( -15.11126220171611045, 120.7387302883610118, -0.8143899245520163088 ) ) ;
#30233 = CARTESIAN_POINT ( 'NONE',  ( -0.4283232389533950801, 25.18001705023179326, -0.8778289364919926729 ) ) ;
#30234 = ORIENTED_EDGE ( 'NONE', *, *, #18395, .T. ) ;
#30235 = CARTESIAN_POINT ( 'NONE',  ( -48.30662019010082986, 17.20352665082216248, 3.142973069415112786 ) ) ;
#30236 = CARTESIAN_POINT ( 'NONE',  ( 7.618479139564603209, 124.7215218652630710, 0.1522353441811852559 ) ) ;
#30237 = CARTESIAN_POINT ( 'NONE',  ( -3.624202338748801377, 120.7384399880717467, 0.3073100964232673427 ) ) ;
#30238 = CARTESIAN_POINT ( 'NONE',  ( 2.037655544652288597, -15.20941935993469585, 5.943311982828837436 ) ) ;
#30239 = CARTESIAN_POINT ( 'NONE',  ( 17.81417655509802955, 146.7645792007554633, -1.532459167469646388 ) ) ;
#30240 = ORIENTED_EDGE ( 'NONE', *, *, #13172, .F. ) ;
#30241 = CARTESIAN_POINT ( 'NONE',  ( -6.675970744194720474, 119.4737997143703012, -1.289985488916530088 ) ) ;
#30242 = CARTESIAN_POINT ( 'NONE',  ( 3.722615052411291980, 115.7030845075131964, 1.610880590277100621 ) ) ;
#30243 = CARTESIAN_POINT ( 'NONE',  ( 3.216700609619024931, -14.42020774479446921, 2.887214088933996337 ) ) ;
#30244 = DIRECTION ( 'NONE',  ( -5.188838149069472160E-16, 1.699382548006136559E-16, 1.000000000000000000 ) ) ;
#30245 = CARTESIAN_POINT ( 'NONE',  ( 4.254723467274340365, 155.8413357349917021, -0.07908073517333519264 ) ) ;
#30246 = ORIENTED_EDGE ( 'NONE', *, *, #35994, .F. ) ;
#30247 = CARTESIAN_POINT ( 'NONE',  ( -4.076413542934153256, 109.5187692929430483, 3.449420018115528563 ) ) ;
#30248 = CARTESIAN_POINT ( 'NONE',  ( 0.9487982336569755759, 106.1808064897677468, 5.207608974602796259 ) ) ;
#30249 = CARTESIAN_POINT ( 'NONE',  ( -2.094298925633724995, 29.77768649804257350, -0.07299356519333505267 ) ) ;
#30250 = EDGE_CURVE ( 'NONE', #17866, #37655, #15786, .T. ) ;
#30251 = DIRECTION ( 'NONE',  ( -1.000000000000000000, -1.004817652842027660E-15, -1.776356839400250465E-15 ) ) ;
#30252 = CARTESIAN_POINT ( 'NONE',  ( 20.68286957925295511, 152.5754960671270055, 0.1900957434528340873 ) ) ;
#30253 = DIRECTION ( 'NONE',  ( -0.8745520943968241312, 0.4849315768086548406, -5.691349986800536046E-16 ) ) ;
#30254 = CARTESIAN_POINT ( 'NONE',  ( 1.790609531311249336, -15.35462110475191366, 5.967943360138708186 ) ) ;
#30255 = CARTESIAN_POINT ( 'NONE',  ( -23.24761240069422286, 77.83567810938664877, -1.524000000000005128 ) ) ;
#30256 = CARTESIAN_POINT ( 'NONE',  ( -2.960856320778833872, 31.17411798999470918, 0.6378382452821288462 ) ) ;
#30257 = EDGE_CURVE ( 'NONE', #5241, #4233, #21891, .T. ) ;
#30258 = CARTESIAN_POINT ( 'NONE',  ( 11.75177080394823825, 120.8928578745602209, 1.619740935434792473 ) ) ;
#30259 = ORIENTED_EDGE ( 'NONE', *, *, #19599, .T. ) ;
#30260 = CARTESIAN_POINT ( 'NONE',  ( 2.561087359964590249, 24.90515699240134495, 8.022552078460996938 ) ) ;
#30261 = CARTESIAN_POINT ( 'NONE',  ( 8.651708239172382520, 118.4867078446797564, -0.7346615941013865392 ) ) ;
#30262 = CARTESIAN_POINT ( 'NONE',  ( -0.2359694434510269667, 106.4201689084969047, -5.118158396747612748 ) ) ;
#30263 = CARTESIAN_POINT ( 'NONE',  ( 4.918189655395446280, 117.4102201643931664, 1.103006975100219167 ) ) ;
#30264 = DIRECTION ( 'NONE',  ( 0.9998004120163610509, 4.016384292689131511E-17, 0.01997839162482749689 ) ) ;
#30265 = DIRECTION ( 'NONE',  ( -0.8745520943968240202, 0.4849315768086551737, -5.361993529360572958E-16 ) ) ;
#30266 = CARTESIAN_POINT ( 'NONE',  ( 0.7336086519982951692, 0.2932837538699786251, -4.563195415240439701 ) ) ;
#30267 = CARTESIAN_POINT ( 'NONE',  ( -4.416771755448872128, 71.99420641645033925, -1.269999999999994245 ) ) ;
#30268 = CARTESIAN_POINT ( 'NONE',  ( -0.9670243388409863750, 105.9610423702829962, -5.250383317772386427 ) ) ;
#30269 = CARTESIAN_POINT ( 'NONE',  ( 3.073681112652024261, -14.41515119294017921, 4.164397941202722109 ) ) ;
#30270 = CARTESIAN_POINT ( 'NONE',  ( 5.284455934299999491, 122.2451909684448310, -0.05007199584899529876 ) ) ;
#30271 = CARTESIAN_POINT ( 'NONE',  ( -21.54968253652557664, 151.3526640061693342, 0.5241015958777710537 ) ) ;
#30272 = CARTESIAN_POINT ( 'NONE',  ( 2.866728174840395216, 37.98889525090484653, 1.397978221435858703 ) ) ;
#30273 = CIRCLE ( 'NONE', #12607, 3.175000000000001155 ) ;
#30274 = CARTESIAN_POINT ( 'NONE',  ( -27.97106122948731510, 77.87043919753004673, -1.524000000000007571 ) ) ;
#30275 = EDGE_LOOP ( 'NONE', ( #709, #10167 ) ) ;
#30276 = CARTESIAN_POINT ( 'NONE',  ( -4.507527029703037869, 105.1215318987586187, -2.874941136914541229 ) ) ;
#30277 = CARTESIAN_POINT ( 'NONE',  ( 4.580902669819289841, -15.62468711146633460, 2.622166941725792899 ) ) ;
#30278 = CARTESIAN_POINT ( 'NONE',  ( -0.03212618750959882197, 158.2819368290249713, 1.607725792532325393 ) ) ;
#30279 = CARTESIAN_POINT ( 'NONE',  ( -4.637963820743935983, -6.603494994175692412, 0.1710436084038768345 ) ) ;
#30280 = EDGE_CURVE ( 'NONE', #3167, #11643, #38352, .T. ) ;
#30281 = VERTEX_POINT ( 'NONE', #11721 ) ;
#30282 = CARTESIAN_POINT ( 'NONE',  ( 3.009276887026298031, 39.20946620154573736, -1.210121013456480599 ) ) ;
#30283 = CARTESIAN_POINT ( 'NONE',  ( 0.7855309748068020070, 120.8419495465347069, 0.4764688261655856683 ) ) ;
#30284 = CARTESIAN_POINT ( 'NONE',  ( -13.22964523056198161, 152.2904283036577908, 1.375236710735038281 ) ) ;
#30285 = CARTESIAN_POINT ( 'NONE',  ( 4.227135066434014377, 117.9852780145697011, 0.9714402365040194498 ) ) ;
#30286 = EDGE_CURVE ( 'NONE', #30808, #19349, #26689, .T. ) ;
#30287 = CARTESIAN_POINT ( 'NONE',  ( 1.346530140708997347, 119.3298839580929638, -0.5995503221117500781 ) ) ;
#30288 = CARTESIAN_POINT ( 'NONE',  ( -15.63125989577342878, 125.4375369430449609, -1.961567602338091243 ) ) ;
#30289 = DIRECTION ( 'NONE',  ( -5.188838149069472160E-16, 1.699382548006136559E-16, 1.000000000000000000 ) ) ;
#30290 = ADVANCED_FACE ( 'NONE', ( #37713 ), #27361, .T. ) ;
#30291 = CARTESIAN_POINT ( 'NONE',  ( 4.158644871452826131, 118.2391781275531883, -0.2328945661949778645 ) ) ;
#30292 = CARTESIAN_POINT ( 'NONE',  ( 15.96529520877005481, 145.8030804522035737, -0.4114451159501716360 ) ) ;
#30293 = ORIENTED_EDGE ( 'NONE', *, *, #1643, .T. ) ;
#30294 = CARTESIAN_POINT ( 'NONE',  ( 3.071204355543858178, -15.18643405355604692, 3.901769932616943493 ) ) ;
#30295 = CARTESIAN_POINT ( 'NONE',  ( 11.66725022231030984, 55.24499999999999744, -5.016500000000003290 ) ) ;
#30296 = CARTESIAN_POINT ( 'NONE',  ( -58.34386316732113897, -0.2371896724559785508, 0.2005938501613158675 ) ) ;
#30297 = CIRCLE ( 'NONE', #11271, 0.3810000000000015041 ) ;
#30298 = CARTESIAN_POINT ( 'NONE',  ( -4.609865753310859127, 8.349128549105346409, -0.5081561704775721111 ) ) ;
#30299 = CARTESIAN_POINT ( 'NONE',  ( 6.520514997712263394, 120.9817801663137971, 0.9553606176145343909 ) ) ;
#30300 = CARTESIAN_POINT ( 'NONE',  ( 2.870896314602991328, 37.68923040074404440, 0.3265960267205035295 ) ) ;
#30301 = B_SPLINE_CURVE_WITH_KNOTS ( 'NONE', 3,
 ( #12364, #34955, #15118, #28121, #41131, #2373, #24928, #15332 ),
 .UNSPECIFIED., .F., .F.,
 ( 4, 2, 2, 4 ),
 ( 1.176555559258168665E-05, 0.0004666053235290343283, 0.0006940252074972603916, 0.0009214450914654865633 ),
 .UNSPECIFIED. ) ;
#30302 = CARTESIAN_POINT ( 'NONE',  ( 4.458631606973747274, 16.91056413504885825, 1.251853190366734259 ) ) ;
#30303 = CARTESIAN_POINT ( 'NONE',  ( 11.83578944268984934, 152.0103986367769551, 0.2843524715992695739 ) ) ;
#30304 = DIRECTION ( 'NONE',  ( 0.3213437296502684171, -0.9469626219732514283, 0.000000000000000000 ) ) ;
#30305 = CARTESIAN_POINT ( 'NONE',  ( -50.34589867275522579, 15.36027825638806910, -4.364407372394879303 ) ) ;
#30306 = CARTESIAN_POINT ( 'NONE',  ( -5.556137103167946734, 116.7241256494533275, -0.2898596823833969882 ) ) ;
#30307 = DIRECTION ( 'NONE',  ( -0.6294287539884060312, -0.7770581983690815209, -1.945484789722797568E-16 ) ) ;
#30308 = DIRECTION ( 'NONE',  ( 3.035386659626960118E-16, -0.000000000000000000, 1.000000000000000000 ) ) ;
#30309 = CARTESIAN_POINT ( 'NONE',  ( 2.079616623477895221, -15.54617723206732371, 5.925385729176053218 ) ) ;
#30310 = CARTESIAN_POINT ( 'NONE',  ( -29.37490963522909482, 66.57792725179109539, -1.270000000000101714 ) ) ;
#30311 = CARTESIAN_POINT ( 'NONE',  ( 8.331117840153179799, 7.414970825009634225, 1.249357972265521255 ) ) ;
#30312 = FACE_BOUND ( 'NONE', #2237, .T. ) ;
#30313 = CARTESIAN_POINT ( 'NONE',  ( -58.55612285180489351, 0.6590214021355567109, -1.048931848374691032E-14 ) ) ;
#30314 = CARTESIAN_POINT ( 'NONE',  ( 6.057513928997552810, 83.56599999999998829, 1.904999999999996030 ) ) ;
#30315 = CARTESIAN_POINT ( 'NONE',  ( -22.98897055778776632, 149.8455236008688303, 0.1339715990509171561 ) ) ;
#30316 = EDGE_CURVE ( 'NONE', #1745, #22781, #6295, .T. ) ;
#30317 = ORIENTED_EDGE ( 'NONE', *, *, #30088, .T. ) ;
#30318 = CARTESIAN_POINT ( 'NONE',  ( -57.43227285409300009, 3.226759729073131133, -2.064049688025099361 ) ) ;
#30319 = CARTESIAN_POINT ( 'NONE',  ( 6.992757797159352862, 121.9549134519901656, 0.1079654902816031131 ) ) ;
#30320 = EDGE_CURVE ( 'NONE', #31705, #5725, #34952, .T. ) ;
#30321 = ORIENTED_EDGE ( 'NONE', *, *, #35539, .T. ) ;
#30322 = DIRECTION ( 'NONE',  ( 0.01731298258488772612, -0.9998501190848634312, 1.788962107505314851E-16 ) ) ;
#30323 = CARTESIAN_POINT ( 'NONE',  ( -2.828086164579570294, 121.0305217392013759, -0.08274239724663733087 ) ) ;
#30324 = CARTESIAN_POINT ( 'NONE',  ( 6.240488881946434141, -13.64759869265259873, 1.419018975165988294 ) ) ;
#30325 = CARTESIAN_POINT ( 'NONE',  ( -13.94573646207672013, 122.0315337860429423, 1.127490061167130797 ) ) ;
#30326 = CARTESIAN_POINT ( 'NONE',  ( 3.254034125433558522, 159.4600617640778353, 0.3425454502237992860 ) ) ;
#30327 = CARTESIAN_POINT ( 'NONE',  ( 0.6391523125838497466, 156.3034662015460583, 0.1199623171637351216 ) ) ;
#30328 = CARTESIAN_POINT ( 'NONE',  ( 0.03652159268533760467, -3.380040448513521589, 0.9750733386546841519 ) ) ;
#30329 = CARTESIAN_POINT ( 'NONE',  ( -23.29193865421797938, 149.0397177335360652, -0.7969840597304522767 ) ) ;
#30330 = CARTESIAN_POINT ( 'NONE',  ( 4.862311738186619436, 117.4092090646522308, 1.165993606892455903 ) ) ;
#30331 = AXIS2_PLACEMENT_3D ( 'NONE', #24375, #21169, #5026 ) ;
#30332 = CARTESIAN_POINT ( 'NONE',  ( -2.204606251742418088, 116.2294481778856152, 0.03196190806868362544 ) ) ;
#30333 = CARTESIAN_POINT ( 'NONE',  ( -18.18950303832469828, 147.2296321676236062, 1.619102437044615428 ) ) ;
#30334 = CARTESIAN_POINT ( 'NONE',  ( -57.41341003177868885, 1.770451042089750793, -1.474359099879954282 ) ) ;
#30335 = CARTESIAN_POINT ( 'NONE',  ( 16.12894526037916521, 128.5601350900737998, -1.548733376446669086 ) ) ;
#30336 = CARTESIAN_POINT ( 'NONE',  ( 0.4015916885733669117, -14.54189033959780808, -0.8905040343298938899 ) ) ;
#30337 = CARTESIAN_POINT ( 'NONE',  ( -9.605778978211169772, 157.4977751962898083, -1.777432263976032489 ) ) ;
#30338 = CARTESIAN_POINT ( 'NONE',  ( -47.43570116002440784, 20.37060963802031566, -5.342502768866047802 ) ) ;
#30339 = EDGE_CURVE ( 'NONE', #1088, #27648, #33482, .T. ) ;
#30340 = CARTESIAN_POINT ( 'NONE',  ( 4.756737841188980020, 105.1215164090288425, 2.421843111834511397 ) ) ;
#30341 = CARTESIAN_POINT ( 'NONE',  ( 16.75300165896958404, 146.9696287467501179, -1.108775417838742783 ) ) ;
#30342 = CARTESIAN_POINT ( 'NONE',  ( -4.936883229164080511, 117.6536490159478774, 0.7443082606323431216 ) ) ;
#30343 = ORIENTED_EDGE ( 'NONE', *, *, #28269, .F. ) ;
#30344 = CARTESIAN_POINT ( 'NONE',  ( -7.396903380747485102, 120.6159063994810055, -1.271367681336521782 ) ) ;
#30345 = CARTESIAN_POINT ( 'NONE',  ( 4.698461193529555935, -15.58032547337365159, 2.177983573914926030 ) ) ;
#30346 = CARTESIAN_POINT ( 'NONE',  ( -4.801729350823258358, 117.4006813127757027, 1.015859690946131932 ) ) ;
#30347 = CARTESIAN_POINT ( 'NONE',  ( -4.489008837794409956, 118.1174813940656492, -0.7254504362431349884 ) ) ;
#30348 = CARTESIAN_POINT ( 'NONE',  ( -51.58367816905025194, 14.91232437457545146, -4.609044670965841917 ) ) ;
#30349 = CARTESIAN_POINT ( 'NONE',  ( 4.065926199369043204, 118.2429491485453354, 0.3080910687088499467 ) ) ;
#30350 = B_SPLINE_SURFACE_WITH_KNOTS ( 'NONE', 1, 3, ( 
 ( #4975, #15728, #40338, #25537, #9353, #12547 ),
 ( #24119, #35138, #28317, #18502, #7949, #12129 ) ),
 .UNSPECIFIED., .F., .F., .F.,
 ( 2, 2 ),
 ( 4, 2, 4 ),
 ( 0.000000000000000000, 1.000000000000000000 ),
 ( 0.000000000000000000, 0.5000000000000000000, 1.000000000000000000 ),
 .UNSPECIFIED. ) ;
#30351 = CARTESIAN_POINT ( 'NONE',  ( 9.271712722858115541, 121.5662863950884400, 1.459403803239323727 ) ) ;
#30352 = DIRECTION ( 'NONE',  ( 0.003125310045138050483, -0.9876883405951376593, -0.1564032425800216952 ) ) ;
#30353 = CARTESIAN_POINT ( 'NONE',  ( 15.97340373827820947, 121.0409387471171101, 0.3191866212789525314 ) ) ;
#30354 = AXIS2_PLACEMENT_3D ( 'NONE', #34067, #31477, #30642 ) ;
#30355 = CARTESIAN_POINT ( 'NONE',  ( 3.617035938018385632, 9.361278981710560387, -7.607506385697127449 ) ) ;
#30356 = CARTESIAN_POINT ( 'NONE',  ( 13.71401989163316237, 150.2158912636999730, 0.8490545446796919915 ) ) ;
#30357 = AXIS2_PLACEMENT_3D ( 'NONE', #5445, #3092, #24807 ) ;
#30358 = CARTESIAN_POINT ( 'NONE',  ( 22.75813664408058301, 148.5871737753741115, -0.7284712318767730954 ) ) ;
#30359 = TOROIDAL_SURFACE ( 'NONE', #22857, 0.7620000000000000107, 0.2540000000000000036 ) ;
#30360 = CARTESIAN_POINT ( 'NONE',  ( 5.177913976931214357, 57.15000000000004832, 5.372099999999999653 ) ) ;
#30361 = CARTESIAN_POINT ( 'NONE',  ( -6.606029807653651701E-14, 92.04146620154574521, -3.372746026535634231E-18 ) ) ;
#30362 = CARTESIAN_POINT ( 'NONE',  ( -58.12768216001780530, 0.1527613808938732554, 0.09815255304908361567 ) ) ;
#30363 = CARTESIAN_POINT ( 'NONE',  ( -11.72569139212704137, 118.7251779360019270, -0.1869994294823656700 ) ) ;
#30364 = ORIENTED_EDGE ( 'NONE', *, *, #14365, .T. ) ;
#30365 = CARTESIAN_POINT ( 'NONE',  ( -47.42394374581075311, 23.94708628835674702, -1.773793246466847773 ) ) ;
#30366 = CARTESIAN_POINT ( 'NONE',  ( -8.033132201554776586, 121.3102024099959380, -1.246334813644621953 ) ) ;
#30367 = CARTESIAN_POINT ( 'NONE',  ( -46.58649794690502688, 25.68081001442151035, -1.571531081469065283 ) ) ;
#30368 = ORIENTED_EDGE ( 'NONE', *, *, #20371, .F. ) ;
#30369 = CARTESIAN_POINT ( 'NONE',  ( -10.75478607932181241, 82.07015292912137738, -1.269999999999999130 ) ) ;
#30370 = CARTESIAN_POINT ( 'NONE',  ( -13.11017186724486372, 133.9996589410087324, -0.6993036124459156566 ) ) ;
#30371 = CARTESIAN_POINT ( 'NONE',  ( 2.708195657389492084, -14.88772387794683105, 5.660366118324242635 ) ) ;
#30372 = CARTESIAN_POINT ( 'NONE',  ( -11.01560508856928067, 119.3804150619309468, 0.7804404673305009865 ) ) ;
#30373 = CARTESIAN_POINT ( 'NONE',  ( -6.517733866319332394E-14, 78.32546620154573702, 2.848871684924056535E-29 ) ) ;
#30374 = CARTESIAN_POINT ( 'NONE',  ( 23.40402153822879683, 142.8142681763856388, 0.5431523703306526674 ) ) ;
#30375 = ORIENTED_EDGE ( 'NONE', *, *, #13703, .T. ) ;
#30376 = CARTESIAN_POINT ( 'NONE',  ( -2.948169924849943335, 1.592661447142720732, -3.562413953034572867 ) ) ;
#30377 = CARTESIAN_POINT ( 'NONE',  ( -21.90559427349704080, 151.4293160993575498, -0.4377259060014663805 ) ) ;
#30378 = DIRECTION ( 'NONE',  ( 4.017660918040594346E-17, -1.000000000000000000, -2.376309959284834438E-19 ) ) ;
#30379 = LINE ( 'NONE', #14394, #36052 ) ;
#30380 = ORIENTED_EDGE ( 'NONE', *, *, #28217, .T. ) ;
#30381 = CARTESIAN_POINT ( 'NONE',  ( 5.000577394074683824, 119.1797654937509492, 1.102527082765531352 ) ) ;
#30382 = EDGE_CURVE ( 'NONE', #26767, #33803, #5775, .T. ) ;
#30383 = CARTESIAN_POINT ( 'NONE',  ( -0.05192310401019068627, -8.293124787585329116, 4.627658001227512585 ) ) ;
#30384 = CARTESIAN_POINT ( 'NONE',  ( 4.872874520552131550, 117.5843641943970681, 0.8145397704027566022 ) ) ;
#30385 = CARTESIAN_POINT ( 'NONE',  ( -48.15927431543178727, 19.02058896284062683, -5.220430799464820915 ) ) ;
#30386 = AXIS2_PLACEMENT_3D ( 'NONE', #4864, #18026, #11862 ) ;
#30387 = CARTESIAN_POINT ( 'NONE',  ( 13.13885824085852860, 121.7804325175133755, -1.194399340605180049 ) ) ;
#30388 = CARTESIAN_POINT ( 'NONE',  ( -4.360315236241580017, -1.596229544307166348, -1.535301415559372940 ) ) ;
#30389 = CARTESIAN_POINT ( 'NONE',  ( -3.876365344914242783, 117.1932757116604762, -0.6224469224293305292 ) ) ;
#30390 = ADVANCED_FACE ( 'NONE', ( #12564 ), #14452, .T. ) ;
#30391 = ORIENTED_EDGE ( 'NONE', *, *, #24786, .T. ) ;
#30392 = ORIENTED_EDGE ( 'NONE', *, *, #40949, .F. ) ;
#30393 = AXIS2_PLACEMENT_3D ( 'NONE', #12711, #2930, #162 ) ;
#30394 = CARTESIAN_POINT ( 'NONE',  ( -14.28939804845289707, 138.9852717218771261, 0.04639197223238064605 ) ) ;
#30395 = CARTESIAN_POINT ( 'NONE',  ( 5.121635214396401459, -14.94813357331645243, 3.889196783476005059 ) ) ;
#30396 = CARTESIAN_POINT ( 'NONE',  ( -46.91190649557855608, 20.26356613537080165, 4.963267847375941955 ) ) ;
#30397 = FACE_OUTER_BOUND ( 'NONE', #104, .T. ) ;
#30398 = EDGE_LOOP ( 'NONE', ( #11428, #1647, #19332, #21911 ) ) ;
#30399 = CARTESIAN_POINT ( 'NONE',  ( 12.88625155327537541, 123.9867020804889961, 1.879256283450041254 ) ) ;
#30400 = CARTESIAN_POINT ( 'NONE',  ( -3.174366308152013705, 104.6144662015457243, -0.06343139340882732180 ) ) ;
#30401 = DIRECTION ( 'NONE',  ( -0.9998004120163608288, 0.000000000000000000, -0.01997839162482747608 ) ) ;
#30402 = AXIS2_PLACEMENT_3D ( 'NONE', #19590, #22989, #35597 ) ;
#30403 = AXIS2_PLACEMENT_3D ( 'NONE', #9897, #39736, #23504 ) ;
#30404 = CARTESIAN_POINT ( 'NONE',  ( -22.12956052442025978, 150.1365687424457178, 0.8564216397177744078 ) ) ;
#30405 = CARTESIAN_POINT ( 'NONE',  ( -8.372926607701892010, 8.771278641329313785, 0.9163881402227073147 ) ) ;
#30406 = CARTESIAN_POINT ( 'NONE',  ( 9.931348751161650057, 124.0638329749226330, 0.9965119107524912367 ) ) ;
#30407 = DIRECTION ( 'NONE',  ( 0.7770581983690896255, -0.6294287539883961502, 3.619230632976993155E-16 ) ) ;
#30408 = CARTESIAN_POINT ( 'NONE',  ( 23.09710566998031922, 146.6371693212631158, -0.4017528712124324164 ) ) ;
#30409 = DIRECTION ( 'NONE',  ( -0.9816537812491090698, -0.1906721105965062946, 1.718035779124596298E-15 ) ) ;
#30410 = AXIS2_PLACEMENT_3D ( 'NONE', #18444, #9506, #6321 ) ;
#30411 = CARTESIAN_POINT ( 'NONE',  ( -54.18067209322861544, 8.473630613757585195, 3.385134444937044407 ) ) ;
#30412 = CARTESIAN_POINT ( 'NONE',  ( -29.05311006279642427, 61.33684941842457050, -1.524000000000005128 ) ) ;
#30413 = CARTESIAN_POINT ( 'NONE',  ( -58.20820809768403592, 1.420579653404085985, 1.355822160094593443 ) ) ;
#30414 = CARTESIAN_POINT ( 'NONE',  ( -57.74402180800798590, 1.613328144073144177, 1.607698224923606034 ) ) ;
#30415 = CARTESIAN_POINT ( 'NONE',  ( -4.401147469462643791, 118.1832779091558905, 0.4087992378694457751 ) ) ;
#30416 = CARTESIAN_POINT ( 'NONE',  ( 0.6996515051864370394, 105.8266127453863987, -5.294619967806604599 ) ) ;
#30417 = AXIS2_PLACEMENT_3D ( 'NONE', #25403, #15587, #29001 ) ;
#30418 = ORIENTED_EDGE ( 'NONE', *, *, #34464, .F. ) ;
#30419 = FACE_OUTER_BOUND ( 'NONE', #2716, .T. ) ;
#30420 = CARTESIAN_POINT ( 'NONE',  ( 8.337297254786394163, 120.0572855657016049, -1.117728404394529917 ) ) ;
#30421 = CARTESIAN_POINT ( 'NONE',  ( -0.1515127994570748815, 105.8822825325953261, -5.338933990912773098 ) ) ;
#30422 = CARTESIAN_POINT ( 'NONE',  ( 4.534812482471024531, 118.1057876144154193, 0.6733639414384589017 ) ) ;
#30423 = CARTESIAN_POINT ( 'NONE',  ( -4.456531362648609829, 120.8671296916768227, -0.5026912216012410228 ) ) ;
#30424 = CARTESIAN_POINT ( 'NONE',  ( -0.2925749420451331240, 115.7029491485453150, -1.764546101263113398 ) ) ;
#30426 = CARTESIAN_POINT ( 'NONE',  ( 1.972857920798343212, 118.1651004355878456, -0.7713121312975299571 ) ) ;
#30425 = B_SPLINE_CURVE_WITH_KNOTS ( 'NONE', 3,
 ( #9156, #11707, #24479, #12347, #8523, #34514 ),
 .UNSPECIFIED., .F., .F.,
 ( 4, 2, 4 ),
 ( 0.000000000000000000, 0.5000000000000000000, 1.000000000000000000 ),
 .UNSPECIFIED. ) ;
#30427 = CARTESIAN_POINT ( 'NONE',  ( 5.379991719817613038, 116.9256180743815179, -0.7442756809649815342 ) ) ;
#30428 = CARTESIAN_POINT ( 'NONE',  ( -10.39772550536733675, 123.9810924921358151, -1.245468829273463252 ) ) ;
#30429 = DIRECTION ( 'NONE',  ( -0.8745520943968235761, 0.4849315768086558398, -4.268512490100410909E-16 ) ) ;
#30430 = CARTESIAN_POINT ( 'NONE',  ( -47.34495446287813536, 19.93462121982016200, 5.151308439916634008 ) ) ;
#30431 = CARTESIAN_POINT ( 'NONE',  ( -30.09725872720941808, 70.36776381375389633, 1.269999999999992024 ) ) ;
#30432 = CARTESIAN_POINT ( 'NONE',  ( -2.874620413851559420, 156.1036891334628933, 0.02956450310463179867 ) ) ;
#30433 = FACE_OUTER_BOUND ( 'NONE', #17799, .T. ) ;
#30434 = CARTESIAN_POINT ( 'NONE',  ( 8.117713882137667980, 117.8329967196738153, 0.7633534655057000462 ) ) ;
#30435 = DIRECTION ( 'NONE',  ( -0.01997839162482737546, -1.040247600000940825E-18, 0.9998004120163610509 ) ) ;
#30436 = CARTESIAN_POINT ( 'NONE',  ( 3.259035188333455846, -14.62011735832338744, 2.262668647611313588 ) ) ;
#30437 = CARTESIAN_POINT ( 'NONE',  ( -18.44328704050468914, 144.7751241387205425, 1.717333923880829838 ) ) ;
#30438 = CARTESIAN_POINT ( 'NONE',  ( 0.1324238259082184954, -4.506001423838159603, -0.9708255322318050107 ) ) ;
#30439 = CARTESIAN_POINT ( 'NONE',  ( -4.801439827634331081, 117.0090399748681875, -0.4924919612534519042 ) ) ;
#30440 = CIRCLE ( 'NONE', #8003, 0.5080000000000000071 ) ;
#30441 = CARTESIAN_POINT ( 'NONE',  ( 0.8415213475290624912, 13.30065917492326122, -0.4928529130785159751 ) ) ;
#30442 = VERTEX_POINT ( 'NONE', #41553 ) ;
#30443 = ADVANCED_FACE ( 'NONE', ( #5149 ), #8351, .F. ) ;
#30444 = CARTESIAN_POINT ( 'NONE',  ( -47.93564525088164885, 15.36257551998183857, -7.016440965503648149E-15 ) ) ;
#30445 = CARTESIAN_POINT ( 'NONE',  ( 3.406460098309076923, 108.6786390861269922, 4.123178694279357792 ) ) ;
#30446 = CARTESIAN_POINT ( 'NONE',  ( -15.67979071779219602, 147.9168465093495399, 0.5330609057418903562 ) ) ;
#30447 = CARTESIAN_POINT ( 'NONE',  ( 4.676120195389507295, -12.14821529611620576, 1.449936329584695649 ) ) ;
#30448 = CARTESIAN_POINT ( 'NONE',  ( 15.03323000681557708, 150.5987129668814077, -1.374706190065595468 ) ) ;
#30449 = EDGE_LOOP ( 'NONE', ( #7185, #41313, #11109, #14301, #29780, #14726 ) ) ;
#30450 = CARTESIAN_POINT ( 'NONE',  ( -11.61050889437352751, 122.1450671466348439, -1.749762830748087694 ) ) ;
#30451 = EDGE_CURVE ( 'NONE', #11376, #36618, #24924, .T. ) ;
#30452 = CARTESIAN_POINT ( 'NONE',  ( 4.303750855783647467, 104.6144662015457953, 2.191315715000266895 ) ) ;
#30453 = CARTESIAN_POINT ( 'NONE',  ( 3.073681112652024261, -14.41515119294017921, 4.164397941202722109 ) ) ;
#30454 = CARTESIAN_POINT ( 'NONE',  ( -4.918661145027864556, 117.4102335145295370, -1.102851133234106662 ) ) ;
#30455 = CARTESIAN_POINT ( 'NONE',  ( 9.568355480995425211, 124.8108731098830049, 0.1557749891131964270 ) ) ;
#30456 = EDGE_LOOP ( 'NONE', ( #14587, #5245, #38780, #19672 ) ) ;
#30457 = CARTESIAN_POINT ( 'NONE',  ( 2.213841846844817329, 118.2767885243204944, 0.7726204694312127641 ) ) ;
#30458 = CARTESIAN_POINT ( 'NONE',  ( 3.611552524025655853, 109.1680412998471610, 3.931639664578665982 ) ) ;
#30459 = CARTESIAN_POINT ( 'NONE',  ( -8.798071503382049130, 117.6842349159514640, -0.1758064068840608507 ) ) ;
#30460 = CARTESIAN_POINT ( 'NONE',  ( -4.864318412922314039, 27.89189352517958298, 0.5016899395801051043 ) ) ;
#30461 = CARTESIAN_POINT ( 'NONE',  ( 0.3092006194327232005, 116.5226405152084652, -0.1184213420814130696 ) ) ;
#30462 = FACE_OUTER_BOUND ( 'NONE', #40684, .T. ) ;
#30463 =( GEOMETRIC_REPRESENTATION_CONTEXT ( 3 ) GLOBAL_UNCERTAINTY_ASSIGNED_CONTEXT ( ( #20142 ) ) GLOBAL_UNIT_ASSIGNED_CONTEXT ( ( #38995, #35375, #9387 ) ) REPRESENTATION_CONTEXT ( 'NONE', 'WORKASPACE' ) );
#30464 = CARTESIAN_POINT ( 'NONE',  ( 1.773284331787727819, -15.30902614633587788, 5.947961136908312518 ) ) ;
#30465 = CARTESIAN_POINT ( 'NONE',  ( -3.671158984043940170E-14, 57.78499999999999659, 0.000000000000000000 ) ) ;
#30466 = DIRECTION ( 'NONE',  ( -0.8745520943968249084, 0.4849315768086533418, -5.311926654347176508E-16 ) ) ;
#30467 = CARTESIAN_POINT ( 'NONE',  ( 20.33492986670560043, 149.7738053052645171, 2.379138827545466128 ) ) ;
#30468 = EDGE_LOOP ( 'NONE', ( #26997, #12795, #21611, #7596 ) ) ;
#30469 = CARTESIAN_POINT ( 'NONE',  ( -7.836836066720379357, 21.45871166075947656, -3.113543590022962881 ) ) ;
#30470 = EDGE_CURVE ( 'NONE', #1690, #13978, #34529, .T. ) ;
#30471 = CARTESIAN_POINT ( 'NONE',  ( 2.436681026199804201, 117.3681707349357879, -0.6167178112848459293 ) ) ;
#30472 = CARTESIAN_POINT ( 'NONE',  ( -2.562387952376977029, 120.6526784328644339, -0.4448203013800773875 ) ) ;
#30473 = CARTESIAN_POINT ( 'NONE',  ( 4.966734726183148041, 117.4023932319876877, 1.002418842663953980 ) ) ;
#30474 = DIRECTION ( 'NONE',  ( -5.188838149069472160E-16, 1.699382548006136559E-16, 1.000000000000000000 ) ) ;
#30475 = CARTESIAN_POINT ( 'NONE',  ( -5.220201361148701480, 105.1221159690571056, 1.151354633625773394 ) ) ;
#30476 = CARTESIAN_POINT ( 'NONE',  ( 4.627880361116947228, 7.839802885307131319, -0.3238752845059330032 ) ) ;
#30477 = CYLINDRICAL_SURFACE ( 'NONE', #23745, 0.5080000000000007843 ) ;
#30478 = CARTESIAN_POINT ( 'NONE',  ( -5.241362157049126225, 57.14999999999997016, -5.310945289804168468 ) ) ;
#30479 = CARTESIAN_POINT ( 'NONE',  ( 2.356490753556696571, -15.00856118213019030, 5.009515689243722925 ) ) ;
#30480 = CARTESIAN_POINT ( 'NONE',  ( 4.551932963793348108, 124.4408722044843927, 0.07212455616362449529 ) ) ;
#30481 = EDGE_CURVE ( 'NONE', #33118, #19034, #4965, .T. ) ;
#30482 = CARTESIAN_POINT ( 'NONE',  ( -3.918109666403713831, 29.36550307138034910, 3.251447169634396062 ) ) ;
#30483 = CARTESIAN_POINT ( 'NONE',  ( -4.345705637489792217, 70.43763872253876457, -1.269999999999994023 ) ) ;
#30484 = VERTEX_POINT ( 'NONE', #12767 ) ;
#30485 = CARTESIAN_POINT ( 'NONE',  ( -3.896500353948071815, 104.6144662015455253, -2.865913902984364103 ) ) ;
#30486 = CARTESIAN_POINT ( 'NONE',  ( 1.975136073220363553, -15.70315947173593685, 5.621751108460156132 ) ) ;
#30487 = CARTESIAN_POINT ( 'NONE',  ( -13.91587783890489760, 154.2684476645699760, 1.737230819368874579 ) ) ;
#30488 = CARTESIAN_POINT ( 'NONE',  ( -1.825063964020108065, -4.879331645356781877, 4.256838567046823840 ) ) ;
#30489 = EDGE_CURVE ( 'NONE', #13569, #37741, #9034, .T. ) ;
#30490 = EDGE_LOOP ( 'NONE', ( #11496, #11275, #34747, #16301 ) ) ;
#30491 = VERTEX_POINT ( 'NONE', #25966 ) ;
#30492 = CYLINDRICAL_SURFACE ( 'NONE', #11002, 2.857500000000000817 ) ;
#30493 = CARTESIAN_POINT ( 'NONE',  ( 1.451835205608120294, 110.3135721340718334, 3.567596948272937940 ) ) ;
#30494 = FILL_AREA_STYLE ('',( #20262 ) ) ;
#30495 = CARTESIAN_POINT ( 'NONE',  ( -0.01887828017123771920, 156.5412816204240301, 0.9447463363288814975 ) ) ;
#30496 = CARTESIAN_POINT ( 'NONE',  ( 5.382937502775954980E-14, 83.56599999999998829, -1.904999999999999805 ) ) ;
#30497 = CARTESIAN_POINT ( 'NONE',  ( 2.489404145489803266, 119.6096776070104681, -0.6201668936895530226 ) ) ;
#30498 = CARTESIAN_POINT ( 'NONE',  ( -3.119203903361180252, 118.1710492231644736, -0.8508709904442464111 ) ) ;
#30499 = FACE_BOUND ( 'NONE', #17844, .T. ) ;
#30500 = CARTESIAN_POINT ( 'NONE',  ( 4.303426754916820585, 118.2142125059335456, -0.3398192420404221314 ) ) ;
#30501 = EDGE_CURVE ( 'NONE', #33914, #29626, #32160, .T. ) ;
#30502 = CARTESIAN_POINT ( 'NONE',  ( 15.94455450784139749, 146.9815093338748966, -0.4077454470555674781 ) ) ;
#30503 = EDGE_LOOP ( 'NONE', ( #14794, #8630, #38992, #16147 ) ) ;
#30504 = CARTESIAN_POINT ( 'NONE',  ( 2.913544029416218262, -15.22775915604775143, 4.213357497968500454 ) ) ;
#30505 = AXIS2_PLACEMENT_3D ( 'NONE', #29896, #13285, #26270 ) ;
#30506 = CARTESIAN_POINT ( 'NONE',  ( 10.94257363143046291, 56.35470871607773802, -4.428493390991016021 ) ) ;
#30507 = CARTESIAN_POINT ( 'NONE',  ( -57.16742739522810979, 2.298121588018744887, 1.685181603002217310 ) ) ;
#30508 = CARTESIAN_POINT ( 'NONE',  ( 4.615940417482057967, 3.801270455692813410, -0.2501868467277520436 ) ) ;
#30510 = ADVANCED_FACE ( 'NONE', ( #16374 ), #2924, .T. ) ;
#30509 = CARTESIAN_POINT ( 'NONE',  ( 9.541807374902186112, 122.7780075402122151, 1.248600054375463619 ) ) ;
#30511 = CARTESIAN_POINT ( 'NONE',  ( 2.935476374454474513, 38.79430649453939850, 1.140240003322550155 ) ) ;
#30512 = CARTESIAN_POINT ( 'NONE',  ( -1.980640663884833064, 106.8720524443079967, 4.823141945187445323 ) ) ;
#30513 = AXIS2_PLACEMENT_3D ( 'NONE', #13241, #13019, #26013 ) ;
#30514 = CARTESIAN_POINT ( 'NONE',  ( 4.203610184846851894, 17.99761390031315500, -1.968029828111186319 ) ) ;
#30515 = CARTESIAN_POINT ( 'NONE',  ( 5.974701571114410470, 155.3719879121972838, 0.2191910023528571561 ) ) ;
#30516 = CARTESIAN_POINT ( 'NONE',  ( -46.80150442283247259, 25.73581779614771747, 1.479909221305397704 ) ) ;
#30517 = EDGE_CURVE ( 'NONE', #24344, #13695, #33544, .T. ) ;
#30518 = CARTESIAN_POINT ( 'NONE',  ( -53.01551111795199489, 8.729259440421063942, -9.365303671399559428E-15 ) ) ;
#30519 = CARTESIAN_POINT ( 'NONE',  ( -5.551613292181984072, 116.7425018655093396, -0.3404755252327396065 ) ) ;
#30520 = FACE_OUTER_BOUND ( 'NONE', #7976, .T. ) ;
#30521 = CARTESIAN_POINT ( 'NONE',  ( -46.82521090855301082, 25.66317510763838072, -1.525079970390816664 ) ) ;
#30522 = CARTESIAN_POINT ( 'NONE',  ( -1.392417755420867209, 106.2993931590560237, 5.100690970918774880 ) ) ;
#30523 = CARTESIAN_POINT ( 'NONE',  ( -31.81160528045694846, 53.04071001996608459, -1.269999999999624984 ) ) ;
#30524 = CARTESIAN_POINT ( 'NONE',  ( -7.020956707233273697, 3.738713905105897517, 4.673168047251142099 ) ) ;
#30525 = EDGE_CURVE ( 'NONE', #1729, #29613, #6626, .T. ) ;
#30526 = CARTESIAN_POINT ( 'NONE',  ( 3.682264917456193221, 76.29346620154572634, 0.07358041635423968885 ) ) ;
#30527 = DIRECTION ( 'NONE',  ( -0.01997839790104462970, 0.000000000000000000, 0.9998004118909472604 ) ) ;
#30528 = CARTESIAN_POINT ( 'NONE',  ( -58.83227707057486811, -0.08366279997995551554, -1.527689555265638282E-14 ) ) ;
#30529 = CARTESIAN_POINT ( 'NONE',  ( 0.005880675322188773195, 122.2435587914035295, -0.2942930402745068674 ) ) ;
#30530 = CARTESIAN_POINT ( 'NONE',  ( -4.789291700406336005, 116.8922783744782379, 0.1888386708474940334 ) ) ;
#30531 = ORIENTED_EDGE ( 'NONE', *, *, #9457, .F. ) ;
#30532 = CARTESIAN_POINT ( 'NONE',  ( -58.13344828981739454, 1.721081384412917359, -0.8123818723938636133 ) ) ;
#30533 = CARTESIAN_POINT ( 'NONE',  ( -6.994921376011119740, 121.9522545830452458, -0.1472782700081636809 ) ) ;
#30534 = AXIS2_PLACEMENT_3D ( 'NONE', #590, #20557, #16955 ) ;
#30535 = ORIENTED_EDGE ( 'NONE', *, *, #5534, .F. ) ;
#30536 = CARTESIAN_POINT ( 'NONE',  ( -46.48963984823998175, 20.58996865087576111, -4.821990630912100784 ) ) ;
#30537 = CARTESIAN_POINT ( 'NONE',  ( -8.463766287105334740, 123.3219012665576315, -0.1265466038023452533 ) ) ;
#30538 = CARTESIAN_POINT ( 'NONE',  ( 5.379112111825198106, -14.48849916137785776, 3.594839802689186570 ) ) ;
#30539 = CIRCLE ( 'NONE', #12179, 13.46199999999999619 ) ;
#30540 = CARTESIAN_POINT ( 'NONE',  ( -9.409928955097594638, 157.3305555497073271, 1.526371511294253525 ) ) ;
#30541 = CARTESIAN_POINT ( 'NONE',  ( 13.35680032055081057, 119.7032035076741465, 0.7543780172957895713 ) ) ;
#30542 = CARTESIAN_POINT ( 'NONE',  ( 22.36672427266394791, 142.2114994846844240, -0.8677673306393176578 ) ) ;
#30543 = CARTESIAN_POINT ( 'NONE',  ( 1.580769961479467911, 28.79261460129497863, -4.363931058323818668 ) ) ;
#30544 = CARTESIAN_POINT ( 'NONE',  ( -20.65160272637294625, 152.5811724025633112, -0.7328296130731978275 ) ) ;
#30545 = CARTESIAN_POINT ( 'NONE',  ( -53.34828122837022590, 10.48226620245167773, -3.972818369368981806 ) ) ;
#30546 = CARTESIAN_POINT ( 'NONE',  ( 4.812176722015626851, 117.4067824616802511, 1.197034441852249609 ) ) ;
#30547 = ORIENTED_EDGE ( 'NONE', *, *, #1457, .T. ) ;
#30548 = CARTESIAN_POINT ( 'NONE',  ( 2.192666673048648818, 116.2158040591487804, 0.09658723973292125675 ) ) ;
#30549 = CARTESIAN_POINT ( 'NONE',  ( -17.34190353359467451, 148.5513402141484391, 1.530992562556359182 ) ) ;
#30550 = CARTESIAN_POINT ( 'NONE',  ( -57.55150406752473913, 1.473613606789017316, -1.350324376427143980 ) ) ;
#30551 = CARTESIAN_POINT ( 'NONE',  ( 14.55733092780580051, 125.6573275863457866, -1.461954306844538642 ) ) ;
#30552 = CARTESIAN_POINT ( 'NONE',  ( 0.7703063551133444431, -5.692625084440793515, -0.5956917769006077057 ) ) ;
#30553 = CARTESIAN_POINT ( 'NONE',  ( -21.23477820244549363, 149.4807732621110006, -2.233729070194449218 ) ) ;
#30554 = CARTESIAN_POINT ( 'NONE',  ( -48.59875010875282442, 18.41211343146811785, -5.165832069028398088 ) ) ;
#30555 = EDGE_CURVE ( 'NONE', #20294, #25746, #20437, .T. ) ;
#30556 = CARTESIAN_POINT ( 'NONE',  ( 0.5902664527119602100, 120.3589971203204669, -0.3461335206401334186 ) ) ;
#30557 = CARTESIAN_POINT ( 'NONE',  ( -28.42835727709238114, 77.69497285144578314, -1.270000000000007567 ) ) ;
#30558 = ORIENTED_EDGE ( 'NONE', *, *, #26070, .T. ) ;
#30559 = CARTESIAN_POINT ( 'NONE',  ( -14.20821676177101267, 128.5469532985352714, -2.008711173933038996 ) ) ;
#30560 = CARTESIAN_POINT ( 'NONE',  ( 3.609959606426583978, -15.77075149864894144, 4.467226954163184161 ) ) ;
#30561 = CYLINDRICAL_SURFACE ( 'NONE', #697, 0.2539999999999992819 ) ;
#30562 = CARTESIAN_POINT ( 'NONE',  ( -4.504028277950688164, 118.0871507785312815, -0.7872802139486386741 ) ) ;
#30563 = CARTESIAN_POINT ( 'NONE',  ( -51.09990735641632398, 14.52648110433587370, -4.713018929684125169 ) ) ;
#30564 = CYLINDRICAL_SURFACE ( 'NONE', #16352, 2.540000000000000480 ) ;
#30565 = CARTESIAN_POINT ( 'NONE',  ( 0.8698789912701805349, 157.1975648536147787, 1.511617766987151557 ) ) ;
#30566 = CARTESIAN_POINT ( 'NONE',  ( -24.50334120614357403, 81.61487340491997600, 1.269999999999991802 ) ) ;
#30567 = AXIS2_PLACEMENT_3D ( 'NONE', #15488, #21438, #25076 ) ;
#30568 = VECTOR ( 'NONE', #36465, 1000.000000000000000 ) ;
#30569 = CARTESIAN_POINT ( 'NONE',  ( 6.894732321505262718, 117.1676844715483270, 0.1377731603346603051 ) ) ;
#30570 = CARTESIAN_POINT ( 'NONE',  ( 4.698174212119619497, 9.136213905105968536, -7.004248122051734526 ) ) ;
#30571 = CARTESIAN_POINT ( 'NONE',  ( 6.481656071630105487, 121.7133186976561205, 0.3761587846782802891 ) ) ;
#30572 = CARTESIAN_POINT ( 'NONE',  ( 12.94589274040318472, 156.9034992427187376, -0.7570359663163892527 ) ) ;
#30573 = EDGE_CURVE ( 'NONE', #1213, #35331, #1218, .T. ) ;
#30574 = DIRECTION ( 'NONE',  ( 5.188838149069472160E-16, -1.699382548006136559E-16, -1.000000000000000000 ) ) ;
#30575 = CARTESIAN_POINT ( 'NONE',  ( 9.132817075745611705E-16, 9.026346327358515609, 0.000000000000000000 ) ) ;
#30576 = EDGE_CURVE ( 'NONE', #5052, #20172, #25757, .T. ) ;
#30577 = CARTESIAN_POINT ( 'NONE',  ( -57.72731561024293967, 0.8685078910841970146, -1.031171003586682213E-14 ) ) ;
#30578 = CARTESIAN_POINT ( 'NONE',  ( -13.67717291712373751, 119.6429072192227494, -0.2244666789651031946 ) ) ;
#30579 = VERTEX_POINT ( 'NONE', #9369 ) ;
#30580 = CARTESIAN_POINT ( 'NONE',  ( -47.06635113313992491, 25.00568333085942996, -1.230463370088899389 ) ) ;
#30581 = CARTESIAN_POINT ( 'NONE',  ( 5.882867916042628487, 121.3061504640725587, -0.1808544764108790948 ) ) ;
#30582 = CYLINDRICAL_SURFACE ( 'NONE', #22362, 2.857500000000000817 ) ;
#30583 = ORIENTED_EDGE ( 'NONE', *, *, #26007, .F. ) ;
#30584 = CARTESIAN_POINT ( 'NONE',  ( 2.811900354768880117, 118.7629491485453883, -1.088252837335328627 ) ) ;
#30585 = CARTESIAN_POINT ( 'NONE',  ( -0.6512579105866077578, 156.3106852680424765, -0.2006220687487342003 ) ) ;
#30586 = CARTESIAN_POINT ( 'NONE',  ( 4.342152980699533593, -13.79257992285246104, 4.116713196511041950 ) ) ;
#30587 = CARTESIAN_POINT ( 'NONE',  ( -14.62453491845912623, 121.8773232776577942, 0.9418922607927827650 ) ) ;
#30588 = CARTESIAN_POINT ( 'NONE',  ( -9.104209967888042598, 153.9432936505793066, -0.1819237819739442652 ) ) ;
#30589 = CARTESIAN_POINT ( 'NONE',  ( 14.83769995734835412, 120.3134675335783754, 0.3991467459773894166 ) ) ;
#30590 = ORIENTED_EDGE ( 'NONE', *, *, #4240, .T. ) ;
#30591 = CARTESIAN_POINT ( 'NONE',  ( 4.529186081025091681, -11.15152372915077095, -0.9203776863585164669 ) ) ;
#30592 = CARTESIAN_POINT ( 'NONE',  ( -16.86202032626315628, 155.2029898760372646, -0.3369432954968343275 ) ) ;
#30593 = CARTESIAN_POINT ( 'NONE',  ( -47.61268981845987014, 19.67534100020180077, -5.209569013876577337 ) ) ;
#30594 = AXIS2_PLACEMENT_3D ( 'NONE', #11174, #10964, #31772 ) ;
#30595 = DIRECTION ( 'NONE',  ( 0.000000000000000000, 0.000000000000000000, 1.000000000000000000 ) ) ;
#30596 = ORIENTED_EDGE ( 'NONE', *, *, #2746, .F. ) ;
#30597 = CARTESIAN_POINT ( 'NONE',  ( 8.253395472087738938, 120.2163864936747331, 1.448344939060297154 ) ) ;
#30598 = VECTOR ( 'NONE', #26139, 1000.000000000000000 ) ;
#30599 = CARTESIAN_POINT ( 'NONE',  ( -4.567530434605131084, -10.44214056487004250, 0.7003524306260878740 ) ) ;
#30600 = CARTESIAN_POINT ( 'NONE',  ( 11.09758427587538954, 119.2389763063149388, 1.130321237809625456 ) ) ;
#30601 = CARTESIAN_POINT ( 'NONE',  ( -58.71347258052157514, -0.3150591082025228085, -0.2754856216375807243 ) ) ;
#30602 = CARTESIAN_POINT ( 'NONE',  ( 13.44735859403575873, 121.7711344121973411, -1.154596522737721953 ) ) ;
#30603 = CARTESIAN_POINT ( 'NONE',  ( -3.942997264624582776, -11.51663297089948479, -2.426127359622226809 ) ) ;
#30604 = CARTESIAN_POINT ( 'NONE',  ( -22.22261828963542740, 149.8733841865972920, -1.744734864234218863 ) ) ;
#30605 = ORIENTED_EDGE ( 'NONE', *, *, #33709, .F. ) ;
#30606 = CARTESIAN_POINT ( 'NONE',  ( -15.76950829013782496, 146.9135488020124001, 0.01503653553346940078 ) ) ;
#30607 = CARTESIAN_POINT ( 'NONE',  ( 6.371418708240476292, -13.42079056852439578, 0.8326245159988630018 ) ) ;
#30608 = CARTESIAN_POINT ( 'NONE',  ( 4.911219615879212519, 115.6909491485453145, 1.456365542632356513 ) ) ;
#30609 = CARTESIAN_POINT ( 'NONE',  ( -4.438458786732819128, 110.9173261775273716, -3.021370786321469382 ) ) ;
#30610 = VERTEX_POINT ( 'NONE', #32366 ) ;
#30611 = CARTESIAN_POINT ( 'NONE',  ( 18.57576200519309495, 149.2887123452801745, 2.480868434872863570 ) ) ;
#30612 = DIRECTION ( 'NONE',  ( 1.000000000000000000, 0.000000000000000000, -6.146657985744592735E-16 ) ) ;
#30613 = CARTESIAN_POINT ( 'NONE',  ( -30.03765869224011453, 57.96144573378211362, -1.270000000000005347 ) ) ;
#30614 = CARTESIAN_POINT ( 'NONE',  ( -14.01781138111955194, 120.5923583732999873, 0.6175494627556293858 ) ) ;
#30615 = CARTESIAN_POINT ( 'NONE',  ( -7.798946185677827714, 9.198776092563324625, 3.184250115244839030 ) ) ;
#30616 = CARTESIAN_POINT ( 'NONE',  ( 15.88363809060971654, 147.6644253265642135, 1.281895537487840686 ) ) ;
#30617 = DIRECTION ( 'NONE',  ( 9.627370216492862708E-17, 1.000000000000000000, -0.000000000000000000 ) ) ;
#30618 = AXIS2_PLACEMENT_3D ( 'NONE', #8302, #21898, #38328 ) ;
#30619 = CARTESIAN_POINT ( 'NONE',  ( 15.42235106321962768, 121.0727120035890323, -0.2994195231956989778 ) ) ;
#30620 = DIRECTION ( 'NONE',  ( 6.353134868986659519E-16, -1.000000000000000000, 0.000000000000000000 ) ) ;
#30621 = CARTESIAN_POINT ( 'NONE',  ( -56.42582858034832327, 3.870711698533446210, 2.205403966022755124 ) ) ;
#30622 = SURFACE_STYLE_USAGE ( .BOTH. , #8049 ) ;
#30623 = EDGE_CURVE ( 'NONE', #9160, #40785, #36916, .T. ) ;
#30624 = CARTESIAN_POINT ( 'NONE',  ( -58.23017998949752183, 0.6774554162835566551, 1.209604144815701554 ) ) ;
#30625 = CARTESIAN_POINT ( 'NONE',  ( -58.64599579737798507, -0.3125068858902338431, 0.3366065011986605349 ) ) ;
#30626 = CARTESIAN_POINT ( 'NONE',  ( -4.163803051339170835, 118.2394256923515172, 0.2270854623594056043 ) ) ;
#30627 = FACE_OUTER_BOUND ( 'NONE', #22284, .T. ) ;
#30628 = EDGE_LOOP ( 'NONE', ( #14600, #2145, #17696, #15386, #35843 ) ) ;
#30629 = CARTESIAN_POINT ( 'NONE',  ( -52.06546789126484498, 13.38259882428268632, 4.575081192416372566 ) ) ;
#30630 = CARTESIAN_POINT ( 'NONE',  ( -4.001816602806133716, 119.1496993116277423, -0.9235019185135577846 ) ) ;
#30631 = CARTESIAN_POINT ( 'NONE',  ( -4.396974916608651363, 111.2411499886600268, -3.139452135551013434 ) ) ;
#30632 = CARTESIAN_POINT ( 'NONE',  ( 4.154030820756847930, 118.2394444196112175, 0.3904055952957847242 ) ) ;
#30633 = CARTESIAN_POINT ( 'NONE',  ( -0.7026863963000727908, 156.4221767039705071, -0.7130674712139343230 ) ) ;
#30634 = CARTESIAN_POINT ( 'NONE',  ( -1.287351889385697445, 115.7028695692513622, -1.739237698640231145 ) ) ;
#30635 = AXIS2_PLACEMENT_3D ( 'NONE', #18688, #25514, #12523 ) ;
#30636 = CARTESIAN_POINT ( 'NONE',  ( 0.5993613099093353380, 117.9496052370437837, -1.382670436843215889 ) ) ;
#30637 = VERTEX_POINT ( 'NONE', #6391 ) ;
#30638 = CARTESIAN_POINT ( 'NONE',  ( 5.634266555046360203, 117.9149360781225937, -0.5245629147119164060 ) ) ;
#30639 = CARTESIAN_POINT ( 'NONE',  ( -1.480437121830183278, 120.3785564700922492, -0.4209679054048330316 ) ) ;
#30640 = CARTESIAN_POINT ( 'NONE',  ( 5.329260751456349254, 104.6144662015457527, 0.2904590649852882289 ) ) ;
#30641 = CARTESIAN_POINT ( 'NONE',  ( -45.03191848990698531, 21.16108440570966209, 3.788620003472263242 ) ) ;
#30642 = DIRECTION ( 'NONE',  ( 0.9998004120163609398, 0.000000000000000000, 0.01997839162482749689 ) ) ;
#30643 = CARTESIAN_POINT ( 'NONE',  ( -0.6547363933663787883, 120.9971525928537801, 0.08613384396314510694 ) ) ;
#30644 = CARTESIAN_POINT ( 'NONE',  ( 5.010184479710102501, 117.3993854065330851, 0.7504461923096029663 ) ) ;
#30645 = CARTESIAN_POINT ( 'NONE',  ( 14.90772019895836742, 120.8072429308574414, 0.9794594453158805836 ) ) ;
#30646 = CARTESIAN_POINT ( 'NONE',  ( 5.305748947172191698, 77.01756249999996840, -5.247078976224250013 ) ) ;
#30648 = CARTESIAN_POINT ( 'NONE',  ( 0.4065252312483833563, 117.6538564835029206, -0.4930844833531825566 ) ) ;
#30647 = CARTESIAN_POINT ( 'NONE',  ( 1.978641239374031136, -15.23252017110923795, 5.293569756250467329 ) ) ;
#30649 = CARTESIAN_POINT ( 'NONE',  ( -2.416701088390952101, 119.2205458019918751, 0.6800916218662637069 ) ) ;
#30650 = CARTESIAN_POINT ( 'NONE',  ( -0.4837089014371968032, -0.2951250844416551944, 0.8451309203121293301 ) ) ;
#30651 = CARTESIAN_POINT ( 'NONE',  ( -0.3303419930535180238, 116.8490449975401617, -0.2909865916005162645 ) ) ;
#30652 = CARTESIAN_POINT ( 'NONE',  ( -0.9201843903949125103, 16.76996313919548598, -0.3265437062991076722 ) ) ;
#30653 = ORIENTED_EDGE ( 'NONE', *, *, #22449, .F. ) ;
#30654 = CARTESIAN_POINT ( 'NONE',  ( -49.53550897992070645, 16.97828837979668748, 4.976283659310158924 ) ) ;
#30655 = CARTESIAN_POINT ( 'NONE',  ( -15.56233417011326914, 148.0963874134046705, 0.5341686659567149720 ) ) ;
#30656 = CARTESIAN_POINT ( 'NONE',  ( 3.467186027297813666, -14.69398785160878873, 5.340258725024584763 ) ) ;
#30657 = CARTESIAN_POINT ( 'NONE',  ( 2.594326071755596264, 120.1437993944865354, -0.4899928688880347272 ) ) ;
#30658 = ORIENTED_EDGE ( 'NONE', *, *, #13641, .T. ) ;
#30659 = DIRECTION ( 'NONE',  ( -0.9998004120163608288, 0.000000000000000000, -0.01997839162482749342 ) ) ;
#30660 = CARTESIAN_POINT ( 'NONE',  ( 3.361318737587208005, -13.21634134694392415, 1.934622048986600840 ) ) ;
#30661 = CARTESIAN_POINT ( 'NONE',  ( -13.15921246430372449, 51.38419125632634632, -1.269999999999995355 ) ) ;
#30662 = CARTESIAN_POINT ( 'NONE',  ( 1.612929917264537716, 120.9971453638330985, 0.006532979378300353239 ) ) ;
#30663 = ORIENTED_EDGE ( 'NONE', *, *, #33664, .F. ) ;
#30664 = CARTESIAN_POINT ( 'NONE',  ( 2.584978638890189195, 158.3255140430775043, 1.682483135129623220 ) ) ;
#30665 = CARTESIAN_POINT ( 'NONE',  ( 3.100266737524950855, 108.5668738132174980, 4.179634342183701001 ) ) ;
#30666 = CARTESIAN_POINT ( 'NONE',  ( -6.650126595083637682, 78.47834120613788400, 1.270000000000001572 ) ) ;
#30667 = AXIS2_PLACEMENT_3D ( 'NONE', #1649, #1851, #18012 ) ;
#30668 = CARTESIAN_POINT ( 'NONE',  ( 0.02874440110933761117, 158.8294072187990196, -1.438487372358303151 ) ) ;
#30669 = CARTESIAN_POINT ( 'NONE',  ( 16.06481930096618527, 121.2308719818149712, 0.1605585295567895088 ) ) ;
#30670 = FACE_OUTER_BOUND ( 'NONE', #24991, .T. ) ;
#30671 = AXIS2_PLACEMENT_3D ( 'NONE', #9967, #6572, #35334 ) ;
#30672 = CARTESIAN_POINT ( 'NONE',  ( 1.867637906597176212, -15.52365582206542705, 5.409599005316564124 ) ) ;
#30673 = CARTESIAN_POINT ( 'NONE',  ( 4.973152232786927307, 117.3993868326352015, 0.9753084504214339923 ) ) ;
#30674 = LINE ( 'NONE', #14478, #29356 ) ;
#30675 = CARTESIAN_POINT ( 'NONE',  ( -4.750738626650226948, 117.8973642380069009, 0.7609203212133225369 ) ) ;
#30676 = ORIENTED_EDGE ( 'NONE', *, *, #37510, .T. ) ;
#30677 = CARTESIAN_POINT ( 'NONE',  ( 5.158690622980511620, 18.63085216599767691, -6.696816702733363158 ) ) ;
#30678 = CARTESIAN_POINT ( 'NONE',  ( 3.286808489197310390, 118.4247336556115755, -0.7816159185997836323 ) ) ;
#30679 = CARTESIAN_POINT ( 'NONE',  ( -4.364892838101932071, 123.4689364668338385, -0.1663115080531033796 ) ) ;
#30680 = CARTESIAN_POINT ( 'NONE',  ( 4.771985164551651337, 117.7362450968562513, 1.071331016765174393 ) ) ;
#30681 = CARTESIAN_POINT ( 'NONE',  ( -17.14500000000466784, 71.11999999999886768, -1.270000000000000684 ) ) ;
#30682 = CARTESIAN_POINT ( 'NONE',  ( -0.005099097579550932770, 122.5569158606516993, 0.2551796940111170642 ) ) ;
#30683 = CARTESIAN_POINT ( 'NONE',  ( -4.627450822138572839, 2.892058097378844117, -0.1328416527703782657 ) ) ;
#30684 = CARTESIAN_POINT ( 'NONE',  ( -5.277062234826722431, 115.6909491485453003, 0.8093865127289260331 ) ) ;
#30685 = CARTESIAN_POINT ( 'NONE',  ( 3.041920762657289057, -14.42862556718194078, 4.364129476586208867 ) ) ;
#30686 = CARTESIAN_POINT ( 'NONE',  ( 4.148164184366611273, 118.0988315448752530, -0.6394906134413953502 ) ) ;
#30687 = CARTESIAN_POINT ( 'NONE',  ( 1.995069716065772658, 37.04168019532015421, 1.843784556858777846 ) ) ;
#30688 = CARTESIAN_POINT ( 'NONE',  ( -0.9905630945189539682, 115.7029491485453576, 1.712266955583646721 ) ) ;
#30689 = ORIENTED_EDGE ( 'NONE', *, *, #22903, .F. ) ;
#30690 = CARTESIAN_POINT ( 'NONE',  ( -4.306318207249558938, 105.1217634520768343, -3.167947131901895030 ) ) ;
#30691 = CARTESIAN_POINT ( 'NONE',  ( 3.858334187661429215, -15.75373651934012997, 4.144460154494749915 ) ) ;
#30692 = CARTESIAN_POINT ( 'NONE',  ( -1.243168248769069617, 118.5604221528582372, 0.6402677339867958173 ) ) ;
#30693 = VECTOR ( 'NONE', #34882, 1000.000000000000114 ) ;
#30694 = CARTESIAN_POINT ( 'NONE',  ( -0.7403349074254782503, 24.03625360216656404, 0.6378939806667418555 ) ) ;
#30695 = ORIENTED_EDGE ( 'NONE', *, *, #7627, .F. ) ;
#30696 = ORIENTED_EDGE ( 'NONE', *, *, #35994, .T. ) ;
#30697 = DIRECTION ( 'NONE',  ( -4.017660918040594346E-17, 1.000000000000000000, 2.376309959284834438E-19 ) ) ;
#30698 = CARTESIAN_POINT ( 'NONE',  ( 1.417747896749451231, 115.2915405621345144, 1.855271064302983275 ) ) ;
#30699 = SURFACE_SIDE_STYLE ('',( #27518 ) ) ;
#30700 = CARTESIAN_POINT ( 'NONE',  ( -0.7813136802280215010, 156.5584078035761593, 0.9574549430346845913 ) ) ;
#30701 = CARTESIAN_POINT ( 'NONE',  ( 16.42052266156670726, 59.67959903468464233, 5.072843609925764774 ) ) ;
#30702 = CARTESIAN_POINT ( 'NONE',  ( 4.577529327193063935, 118.0358422625909327, -0.6747486238782739454 ) ) ;
#30703 = CARTESIAN_POINT ( 'NONE',  ( 17.70889067045657228, 148.6960320134204210, -1.618934763233637497 ) ) ;
#30704 = AXIS2_PLACEMENT_3D ( 'NONE', #19335, #12746, #9548 ) ;
#30705 = CARTESIAN_POINT ( 'NONE',  ( -20.10333444936999214, 149.6821479856479300, -2.421853341415478145 ) ) ;
#30706 = DIRECTION ( 'NONE',  ( -1.000000000000000000, 0.000000000000000000, 0.000000000000000000 ) ) ;
#30707 = CARTESIAN_POINT ( 'NONE',  ( 4.166221732904972441, 118.2394651950648097, -0.2241750351714766332 ) ) ;
#30708 = CARTESIAN_POINT ( 'NONE',  ( 10.55375732331616767, 153.0603347025997323, -0.3251829154788380416 ) ) ;
#30709 = VERTEX_POINT ( 'NONE', #9782 ) ;
#30710 = CARTESIAN_POINT ( 'NONE',  ( 2.460727335429193197, -15.06314154744310585, 4.845259171755021299 ) ) ;
#30711 = CIRCLE ( 'NONE', #19150, 14.73199999999999577 ) ;
#30712 = CARTESIAN_POINT ( 'NONE',  ( 11.47253659098496925, 56.76836532675937974, -5.016500000000000625 ) ) ;
#30713 = CARTESIAN_POINT ( 'NONE',  ( -57.21909960283011287, 2.250382150482001187, 1.879871960359134286 ) ) ;
#30714 = CARTESIAN_POINT ( 'NONE',  ( 1.294644163514462987, -7.843371450943685375, 4.453423563430108700 ) ) ;
#30715 = CARTESIAN_POINT ( 'NONE',  ( 13.21686059441242911, 128.5100244389050204, 1.738961528769450648 ) ) ;
#30716 = CARTESIAN_POINT ( 'NONE',  ( 1.747231708741132872, 35.57765484641747378, 2.108037137287274820 ) ) ;
#30717 = CARTESIAN_POINT ( 'NONE',  ( -6.300951452924162588, 121.9812576474260055, 0.03014847038595266579 ) ) ;
#30718 = AXIS2_PLACEMENT_3D ( 'NONE', #34938, #41540, #8309 ) ;
#30719 = CIRCLE ( 'NONE', #6267, 9.048749999999998295 ) ;
#30720 = CARTESIAN_POINT ( 'NONE',  ( -1.214995109038484067, 0.9429784454696930052, -4.460028654918597901 ) ) ;
#30721 = CARTESIAN_POINT ( 'NONE',  ( 8.053145991180159058, 122.8529229587361442, 0.1924930237977969527 ) ) ;
#30722 = CARTESIAN_POINT ( 'NONE',  ( -10.79307885933852340, 57.10041794475175436, 5.016499999999999737 ) ) ;
#30723 = EDGE_CURVE ( 'NONE', #25607, #37389, #22750, .T. ) ;
#30724 = CIRCLE ( 'NONE', #23135, 5.588000000000006295 ) ;
#30725 = CARTESIAN_POINT ( 'NONE',  ( -58.22824150656796860, 0.01698906185855497686, -0.5964212723216403278 ) ) ;
#30726 = CARTESIAN_POINT ( 'NONE',  ( 2.165901765101517107, 116.3326876175183600, -0.1937117289139740073 ) ) ;
#30727 = CARTESIAN_POINT ( 'NONE',  ( 0.005880675324072524163, 122.2435587914035295, -0.2942930402744691754 ) ) ;
#30728 = DIRECTION ( 'NONE',  ( 0.9816537812491077375, 0.1906721105965138996, 4.769617732184456426E-16 ) ) ;
#30729 = CARTESIAN_POINT ( 'NONE',  ( 1.822811606207358492, -15.29362660170948374, 5.402418844745950466 ) ) ;
#30730 = DIRECTION ( 'NONE',  ( -5.188838149069471174E-16, 1.699382548006136313E-16, 1.000000000000000000 ) ) ;
#30731 = CARTESIAN_POINT ( 'NONE',  ( 2.430217625452450569, 5.689826410578260329, 8.062849060857743666 ) ) ;
#30732 = DIRECTION ( 'NONE',  ( 0.01997839162482749689, 1.040247600000945640E-18, -0.9998004120163610509 ) ) ;
#30733 = CARTESIAN_POINT ( 'NONE',  ( -15.19943428492320869, 148.1072807477730748, -0.3037208696559880461 ) ) ;
#30734 = CARTESIAN_POINT ( 'NONE',  ( -58.19197273006702886, 1.486408586729007109, 1.232490673556611016 ) ) ;
#30735 = CARTESIAN_POINT ( 'NONE',  ( 0.004379098344251805552, 122.8649044353672934, -0.2191479880734040764 ) ) ;
#30736 = CARTESIAN_POINT ( 'NONE',  ( -2.823947636868171074, 116.6946238705719594, 0.1909394059425172097 ) ) ;
#30737 = EDGE_LOOP ( 'NONE', ( #27202, #15763, #2173, #16579, #12161 ) ) ;
#30738 = CARTESIAN_POINT ( 'NONE',  ( -56.10358335640970751, 6.949471795635917104, -1.762666882438596261 ) ) ;
#30739 = EDGE_LOOP ( 'NONE', ( #39821, #14204, #8287, #23444 ) ) ;
#30740 = DIRECTION ( 'NONE',  ( -0.9998004120163608288, 0.000000000000000000, -0.01997839162482750383 ) ) ;
#30741 = CARTESIAN_POINT ( 'NONE',  ( -7.552512487614272629, 122.4261604937442485, -0.1509171734833087142 ) ) ;
#30742 = CARTESIAN_POINT ( 'NONE',  ( 5.719270376754757912, -14.62604927220606577, 2.811085246033490304 ) ) ;
#30743 = CARTESIAN_POINT ( 'NONE',  ( -0.01051220311291028477, 117.9844940561907265, 0.5260736299896252577 ) ) ;
#30744 = CARTESIAN_POINT ( 'NONE',  ( 22.28974849274159453, 149.2301036976659816, -0.9981255638314733281 ) ) ;
#30745 = CARTESIAN_POINT ( 'NONE',  ( -4.636761822055341042, 12.60011390031314349, 0.2095705037016724059 ) ) ;
#30746 = CARTESIAN_POINT ( 'NONE',  ( -10.77008264951280836, 157.9328640892066460, -0.4716003899658737786 ) ) ;
#30747 = CARTESIAN_POINT ( 'NONE',  ( -52.27215747984514138, 12.44583702737001829, -4.333897384857193558 ) ) ;
#30748 = ORIENTED_EDGE ( 'NONE', *, *, #6109, .F. ) ;
#30749 = CARTESIAN_POINT ( 'NONE',  ( 5.562477116651607822, 116.6983427989447648, 0.1303901686245120817 ) ) ;
#30750 = CARTESIAN_POINT ( 'NONE',  ( -11.15120438727553420, 123.3376105302527037, 1.132373765670515509 ) ) ;
#30751 = CARTESIAN_POINT ( 'NONE',  ( -51.93264227491449248, 12.78224484401628303, -4.246411715856839741 ) ) ;
#30752 = CARTESIAN_POINT ( 'NONE',  ( 8.255438862926419930, 156.5149677146980309, -1.736665298733278684 ) ) ;
#30753 = CARTESIAN_POINT ( 'NONE',  ( -21.09420047167898460, 149.7512365312068709, -2.228874019815534346 ) ) ;
#30754 = CARTESIAN_POINT ( 'NONE',  ( -46.97515415817095175, 24.89137758704647396, -2.045406795549908896 ) ) ;
#30755 = CIRCLE ( 'NONE', #34184, 12.69999999999999751 ) ;
#30756 = ADVANCED_FACE ( 'NONE', ( #23550 ), #1008, .T. ) ;
#30757 = CARTESIAN_POINT ( 'NONE',  ( 9.877746432283215583, 123.9483309312939099, -0.5948279539607076449 ) ) ;
#30758 = ORIENTED_EDGE ( 'NONE', *, *, #7844, .F. ) ;
#30759 = CARTESIAN_POINT ( 'NONE',  ( -5.054692016413513400, 119.8577235299091228, -1.014870397641471689 ) ) ;
#30760 = CARTESIAN_POINT ( 'NONE',  ( 2.350550293776238586, -15.63281720864678803, 5.143235457246400522 ) ) ;
#30761 = CARTESIAN_POINT ( 'NONE',  ( -4.478377892402201077, 118.1173504798736644, -0.7356672007679183611 ) ) ;
#30762 = CARTESIAN_POINT ( 'NONE',  ( -55.73247374733729487, 5.492406230130003841, -2.854677165782116610 ) ) ;
#30763 = VECTOR ( 'NONE', #28420, 1000.000000000000000 ) ;
#30764 = CARTESIAN_POINT ( 'NONE',  ( 19.68500000000000227, 71.11999999999999034, 5.016499999999999737 ) ) ;
#30765 = CARTESIAN_POINT ( 'NONE',  ( 18.11030164959022670, 147.2296321676236062, 2.344458923443068610 ) ) ;
#30766 = DIRECTION ( 'NONE',  ( -5.188838149069472160E-16, 1.699382548006136559E-16, 1.000000000000000000 ) ) ;
#30767 = SHAPE_REPRESENTATION ( 'MAS-162', ( #8728, #38658, #5338, #12108, #3297, #25723, #20268, #40696 ), #16190 ) ;
#30768 = CARTESIAN_POINT ( 'NONE',  ( 22.53594553814337687, 150.7843406352268687, 0.4248312833800683141 ) ) ;
#30769 = ADVANCED_FACE ( 'NONE', ( #22333 ), #39648, .T. ) ;
#30770 = CARTESIAN_POINT ( 'NONE',  ( -2.728255833603390190, 14.33847684266025801, 7.992727065595903291 ) ) ;
#30771 = CARTESIAN_POINT ( 'NONE',  ( 15.59067940631263482, 147.5518517437054982, 0.7624272054715746094 ) ) ;
#30772 = CARTESIAN_POINT ( 'NONE',  ( -58.83227707057486811, -0.08366279997995551554, -1.529465441686574059E-14 ) ) ;
#30773 = CARTESIAN_POINT ( 'NONE',  ( -42.09164859969784089, 21.98995510696678934, -0.2271816505417319221 ) ) ;
#30774 = CARTESIAN_POINT ( 'NONE',  ( 0.07232897131671378599, 118.7629491485454025, 1.278895008221504037 ) ) ;
#30775 = AXIS2_PLACEMENT_3D ( 'NONE', #16272, #16909, #13085 ) ;
#30776 = CARTESIAN_POINT ( 'NONE',  ( -57.71946847630993460, 1.146847591362354368, 1.351507486235933975 ) ) ;
#30777 = EDGE_CURVE ( 'NONE', #15033, #15131, #23288, .T. ) ;
#30778 = CARTESIAN_POINT ( 'NONE',  ( -8.216694157412884891, 117.5064756823292385, -0.07510791844681385943 ) ) ;
#30779 = VERTEX_POINT ( 'NONE', #3194 ) ;
#30780 = CARTESIAN_POINT ( 'NONE',  ( -46.72476011081990066, 26.09744872113180847, -0.08471799968940613157 ) ) ;
#30781 = CARTESIAN_POINT ( 'NONE',  ( -7.857536959375756247, 122.2102078284459310, -0.7978630961384953757 ) ) ;
#30782 = DIRECTION ( 'NONE',  ( -0.8745520943968243532, 0.4849315768086547296, -6.829619984160642269E-16 ) ) ;
#30783 = ORIENTED_EDGE ( 'NONE', *, *, #19947, .F. ) ;
#30784 = CARTESIAN_POINT ( 'NONE',  ( 0.6338829882054587417, 115.7029520802098688, -1.736985041732382440 ) ) ;
#30785 = CARTESIAN_POINT ( 'NONE',  ( -8.124409605001968515, 122.8458379852381910, -0.3720714147651331127 ) ) ;
#30786 = CARTESIAN_POINT ( 'NONE',  ( 2.266344692909419312, -15.23424214381746644, 5.932772278557574275 ) ) ;
#30787 = CARTESIAN_POINT ( 'NONE',  ( -13.98214753592677795, 155.8415165211600595, 1.292431576881029054 ) ) ;
#30788 = CARTESIAN_POINT ( 'NONE',  ( 5.540303739757897361, 78.91648400349126291, -5.100389098699506185 ) ) ;
#30789 = CARTESIAN_POINT ( 'NONE',  ( 8.209937203459256594, 117.5146787832509858, 0.2970838962712568088 ) ) ;
#30790 = CARTESIAN_POINT ( 'NONE',  ( 8.462070910903001675, 123.3219020322049460, 0.2116625524504351652 ) ) ;
#30791 = ORIENTED_EDGE ( 'NONE', *, *, #41566, .F. ) ;
#30792 = CARTESIAN_POINT ( 'NONE',  ( -0.2901879621234837447, 21.01165217803846730, -0.9340445150429393939 ) ) ;
#30793 = CARTESIAN_POINT ( 'NONE',  ( -21.67415503129015164, 132.7302833492884417, -0.4548691923922797420 ) ) ;
#30794 = CARTESIAN_POINT ( 'NONE',  ( -47.73411473560602047, 19.53609853455933631, -5.217284324479045665 ) ) ;
#30795 = AXIS2_PLACEMENT_3D ( 'NONE', #41271, #5287, #18031 ) ;
#30796 = EDGE_LOOP ( 'NONE', ( #11599, #19575, #23679, #27465, #38431, #40274, #11876, #20238, #21762, #15508, #5634, #19856 ) ) ;
#30797 = DIRECTION ( 'NONE',  ( 0.8572391118119521147, 0.5149185422762083686, 3.573031421855339458E-16 ) ) ;
#30798 = ORIENTED_EDGE ( 'NONE', *, *, #4010, .T. ) ;
#30799 = CARTESIAN_POINT ( 'NONE',  ( -3.652649686639886095, 117.9385129362550231, 0.7594146576452507347 ) ) ;
#30800 = CARTESIAN_POINT ( 'NONE',  ( -4.503669762702418033, -0.7216326387320324276, 1.072590735790061922 ) ) ;
#30801 = CARTESIAN_POINT ( 'NONE',  ( 15.42726980375949175, 123.0316835747794642, 1.591438994230371051 ) ) ;
#30802 = CARTESIAN_POINT ( 'NONE',  ( -58.08606908514132527, 0.8771027734565672862, -1.270208019422474743 ) ) ;
#30803 = CARTESIAN_POINT ( 'NONE',  ( 14.64490033095721344, 154.5799843816573684, -1.633817034445553817 ) ) ;
#30804 = CARTESIAN_POINT ( 'NONE',  ( 2.362155674307470310, -13.89060443905824371, -3.983575812745122846 ) ) ;
#30805 = CARTESIAN_POINT ( 'NONE',  ( -8.039955067133034206, 118.1206512225135015, -0.9611422114813541473 ) ) ;
#30806 = CARTESIAN_POINT ( 'NONE',  ( 4.841609353578014918, 117.6754506260240731, -0.8982756364806089300 ) ) ;
#30807 = EDGE_CURVE ( 'NONE', #26988, #36287, #6186, .T. ) ;
#30808 = VERTEX_POINT ( 'NONE', #15954 ) ;
#30809 = CARTESIAN_POINT ( 'NONE',  ( -15.30649785019675768, 148.0176312819745874, 0.02196777213629045461 ) ) ;
#30810 = EDGE_CURVE ( 'NONE', #12622, #27053, #31502, .T. ) ;
#30811 = CARTESIAN_POINT ( 'NONE',  ( 6.400388595320081642, -14.10124341269280990, -0.01754875274584842895 ) ) ;
#30812 = AXIS2_PLACEMENT_3D ( 'NONE', #34268, #1889, #34470 ) ;
#30813 = DIRECTION ( 'NONE',  ( 0.9998004120163609398, 0.000000000000000000, 0.01997839162482749689 ) ) ;
#30814 = AXIS2_PLACEMENT_3D ( 'NONE', #10426, #15963, #28961 ) ;
#30815 = ADVANCED_FACE ( 'NONE', ( #28950 ), #38833, .F. ) ;
#30816 = CARTESIAN_POINT ( 'NONE',  ( -4.605933908340293925, 113.9922470800784424, -2.135287817726405191 ) ) ;
#30817 = VERTEX_POINT ( 'NONE', #40400 ) ;
#30818 = CARTESIAN_POINT ( 'NONE',  ( 16.38264815551527320, 131.4813445454897192, 2.297577408150382805 ) ) ;
#30819 = DIRECTION ( 'NONE',  ( 5.188838149069472160E-16, -1.699382548006136559E-16, -1.000000000000000000 ) ) ;
#30820 = DIRECTION ( 'NONE',  ( 1.000000000000000000, 6.353134868986659519E-16, 0.000000000000000000 ) ) ;
#30821 = AXIS2_PLACEMENT_3D ( 'NONE', #10595, #20376, #20585 ) ;
#30822 = CARTESIAN_POINT ( 'NONE',  ( -1.702772465368850519, 120.1914007830323214, 0.4659475787731968133 ) ) ;
#30823 = CARTESIAN_POINT ( 'NONE',  ( 7.903470162808407196, 13.94468365673557742, -2.927854470364564587 ) ) ;
#30824 = CARTESIAN_POINT ( 'NONE',  ( 16.25331603292275418, 145.9442052555630767, 1.443193537303810281 ) ) ;
#30825 = DIRECTION ( 'NONE',  ( 0.3582377630123915746, -0.9336303900108851028, 3.445432962228667069E-16 ) ) ;
#30826 = CARTESIAN_POINT ( 'NONE',  ( 7.924482676426827688, 158.6683511845044734, -0.3722227806660350358 ) ) ;
#30827 = CARTESIAN_POINT ( 'NONE',  ( -26.37263903973852663, 72.23735686029533554, -1.270000000000005791 ) ) ;
#30828 = CARTESIAN_POINT ( 'NONE',  ( -56.16899616883418389, 4.407705243674411300, 2.360363118971548158 ) ) ;
#30829 = DIRECTION ( 'NONE',  ( -0.9998004120163609398, 0.000000000000000000, -0.01997839162482749689 ) ) ;
#30830 = CARTESIAN_POINT ( 'NONE',  ( -50.36571775388629391, 15.70662508241784927, 4.844678386991165375 ) ) ;
#30831 = DIRECTION ( 'NONE',  ( -4.017660918040594346E-17, 1.000000000000000000, 2.376309959284834438E-19 ) ) ;
#30832 = CARTESIAN_POINT ( 'NONE',  ( -4.292345225184465818, 118.2141485745093803, 0.3519745603735880413 ) ) ;
#30833 = CARTESIAN_POINT ( 'NONE',  ( 3.563749620457647538, 109.2372012348777304, -3.773699991306081802 ) ) ;
#30834 = VERTEX_POINT ( 'NONE', #2045 ) ;
#30835 = CARTESIAN_POINT ( 'NONE',  ( -55.03109054507046238, 6.816801101491506643, 3.135084751894912980 ) ) ;
#30836 = CARTESIAN_POINT ( 'NONE',  ( -6.193434541464478471, 119.7369822425514343, -1.238341368285690303 ) ) ;
#30837 = CARTESIAN_POINT ( 'NONE',  ( -3.418449710216219906, 108.6681208952157078, -4.126741282752677265 ) ) ;
#30838 = AXIS2_PLACEMENT_3D ( 'NONE', #36785, #27185, #10575 ) ;
#30839 = CARTESIAN_POINT ( 'NONE',  ( 4.262834682690650467, 118.2124901016074432, 0.5347958070508012085 ) ) ;
#30840 = CARTESIAN_POINT ( 'NONE',  ( -10.66982511086002994, 153.0728289088170300, -0.9866062039827815378 ) ) ;
#30841 = CARTESIAN_POINT ( 'NONE',  ( -29.78720458899295664, 57.91457584460150088, 1.523999999999994692 ) ) ;
#30842 = DIRECTION ( 'NONE',  ( 0.000000000000000000, 0.000000000000000000, -1.000000000000000000 ) ) ;
#30843 = EDGE_LOOP ( 'NONE', ( #9859, #12333, #38016, #13719 ) ) ;
#30844 = CARTESIAN_POINT ( 'NONE',  ( 4.619096255015035624, 27.05588869245799089, -0.3994036469054788596 ) ) ;
#30845 = CARTESIAN_POINT ( 'NONE',  ( -9.825947633753887800, 123.3250567171901082, -1.189973159844530892 ) ) ;
#30846 = CARTESIAN_POINT ( 'NONE',  ( -30.09725872720941808, 70.36776381375389633, -1.524000000000007349 ) ) ;
#30847 = AXIS2_PLACEMENT_3D ( 'NONE', #34238, #4649, #11427 ) ;
#30848 = CARTESIAN_POINT ( 'NONE',  ( -47.35734194465046443, 19.95394279972230578, 5.176037500974643102 ) ) ;
#30849 = EDGE_CURVE ( 'NONE', #5326, #3642, #36046, .T. ) ;
#30850 = DIRECTION ( 'NONE',  ( -0.1469470846586743706, 0.000000000000000000, 0.9891443546370348727 ) ) ;
#30851 = CARTESIAN_POINT ( 'NONE',  ( -7.802235114625140966, 122.5634249805564338, 0.05936801018636322924 ) ) ;
#30852 = CARTESIAN_POINT ( 'NONE',  ( 3.682264917456193665, 65.62546620154573418, 0.07358041635424013294 ) ) ;
#30853 = CARTESIAN_POINT ( 'NONE',  ( 14.69808362324402395, 120.8948172685174001, 1.121060376578428386 ) ) ;
#30854 = CARTESIAN_POINT ( 'NONE',  ( 5.475330206976777525, 88.73331249999999670, -5.107412922131463695 ) ) ;
#30856 = CARTESIAN_POINT ( 'NONE',  ( 5.880040083609218371, 118.0670013439590491, -0.7714800252663617242 ) ) ;
#30855 = CARTESIAN_POINT ( 'NONE',  ( 3.220330141560203696, -14.30903721375789317, 2.546581355196453345 ) ) ;
#30857 = CARTESIAN_POINT ( 'NONE',  ( -13.69950719238985393, 125.8243951943327517, 1.418320022125399316 ) ) ;
#30858 = CARTESIAN_POINT ( 'NONE',  ( -0.9317526520580600158, -11.96253880033681050, -0.2928614735302202954 ) ) ;
#30859 = CARTESIAN_POINT ( 'NONE',  ( -15.60190333658779771, 121.2802728028965475, -0.9237637308081628751 ) ) ;
#30860 = CARTESIAN_POINT ( 'NONE',  ( 0.9071407760921452734, 21.51634675185595924, 0.3571511405359465430 ) ) ;
#30861 = EDGE_LOOP ( 'NONE', ( #27554, #24865, #33075, #40054 ) ) ;
#30862 = CARTESIAN_POINT ( 'NONE',  ( -49.14072577824711630, 13.89916973120783972, -7.393049121003753577E-15 ) ) ;
#30863 = CARTESIAN_POINT ( 'NONE',  ( -15.82779737147856025, 147.6293441119438512, 0.5318544519934518267 ) ) ;
#30864 = CARTESIAN_POINT ( 'NONE',  ( 4.721845526343314781, -13.23797770169883670, 3.222865150663026590 ) ) ;
#30865 = CARTESIAN_POINT ( 'NONE',  ( 5.134369219807886964, 120.3680889145531552, -0.6721547394862479319 ) ) ;
#30866 = CIRCLE ( 'NONE', #36340, 0.2540000000000013913 ) ;
#30867 = ORIENTED_EDGE ( 'NONE', *, *, #19889, .F. ) ;
#30868 = CARTESIAN_POINT ( 'NONE',  ( 0.5151297239306589226, 115.7029491485453434, 1.762079848971026763 ) ) ;
#30869 = EDGE_CURVE ( 'NONE', #19961, #6241, #6323, .T. ) ;
#30870 = CARTESIAN_POINT ( 'NONE',  ( 3.254806331274714637, -13.89383896039994504, 2.504907480430248246 ) ) ;
#30871 = CARTESIAN_POINT ( 'NONE',  ( -4.767505756759218727, 117.8468658059388900, -0.9622486164732443337 ) ) ;
#30872 = CARTESIAN_POINT ( 'NONE',  ( 9.048378227557773101, 123.9859359328134190, 0.09628433740681516251 ) ) ;
#30873 = EDGE_CURVE ( 'NONE', #18999, #12743, #4079, .T. ) ;
#30874 = ORIENTED_EDGE ( 'NONE', *, *, #1682, .T. ) ;
#30875 = CARTESIAN_POINT ( 'NONE',  ( 15.34515231418505365, 125.4902479783272184, 1.998699669873516882 ) ) ;
#30876 = CARTESIAN_POINT ( 'NONE',  ( -17.14499999999999957, 71.11999999999999034, 5.079999999999997407 ) ) ;
#30877 = APPLICATION_CONTEXT ( 'automotive_design' ) ;
#30878 = CIRCLE ( 'NONE', #9808, 18.32410244842765934 ) ;
#30879 = DIRECTION ( 'NONE',  ( -5.188838149069472160E-16, 1.699382548006136559E-16, 1.000000000000000000 ) ) ;
#30880 = CARTESIAN_POINT ( 'NONE',  ( 0.02156534543286487207, 156.6359106937186709, -1.079218069903262300 ) ) ;
#30881 = CARTESIAN_POINT ( 'NONE',  ( 16.19138771800991350, 121.3864332154274877, 0.1624333549846388725 ) ) ;
#30882 = DIRECTION ( 'NONE',  ( -5.188838149069472160E-16, 1.699382548006136559E-16, 1.000000000000000000 ) ) ;
#30883 = AXIS2_PLACEMENT_3D ( 'NONE', #14062, #7693, #40695 ) ;
#30884 = CARTESIAN_POINT ( 'NONE',  ( 2.015967980637507928, -15.45937876265861277, 5.999498870620294966 ) ) ;
#30885 = LINE ( 'NONE', #41113, #27482 ) ;
#30886 = CARTESIAN_POINT ( 'NONE',  ( -6.682056005205734733E-14, 110.9644662015457328, 1.123945309419055369E-18 ) ) ;
#30887 = CARTESIAN_POINT ( 'NONE',  ( -4.843431534479017309, 117.8278034786011972, 0.6983875874824077012 ) ) ;
#30888 = VERTEX_POINT ( 'NONE', #26923 ) ;
#30889 = VERTEX_POINT ( 'NONE', #7138 ) ;
#30890 = DIRECTION ( 'NONE',  ( -0.8745520943968231320, 0.4849315768086568390, -5.691349986800559712E-16 ) ) ;
#30891 = CARTESIAN_POINT ( 'NONE',  ( 2.584482069992259490, 117.5998511199927776, -0.6690006159187619206 ) ) ;
#30892 = CARTESIAN_POINT ( 'NONE',  ( -2.231675704589730191, 117.6064948828932444, -1.117935386608752024 ) ) ;
#30894 = CARTESIAN_POINT ( 'NONE',  ( 4.804053917469309987, 117.6427837140938806, 1.111766096040093910 ) ) ;
#30893 = CIRCLE ( 'NONE', #36364, 0.3809999999999984510 ) ;
#30895 = CARTESIAN_POINT ( 'NONE',  ( -4.757248700628498916, 117.4032733054477973, -1.206458840162573543 ) ) ;
#30896 = CARTESIAN_POINT ( 'NONE',  ( -0.8427018527672123227, 121.5536190086353372, 0.3367535922268983795 ) ) ;
#30897 = CARTESIAN_POINT ( 'NONE',  ( -4.478778176974228309, 3.316883148187759645, 1.141857468124592101 ) ) ;
#30898 = CARTESIAN_POINT ( 'NONE',  ( -48.28978369826177186, 19.63653578263565436, 5.206999999995388428 ) ) ;
#30899 = CARTESIAN_POINT ( 'NONE',  ( -3.204561054529846853, 108.0377196974498872, -4.255356325961729524 ) ) ;
#30900 = CARTESIAN_POINT ( 'NONE',  ( 2.390819523577490280, -14.89105559343156848, 5.112470274569719919 ) ) ;
#30901 = B_SPLINE_CURVE_WITH_KNOTS ( 'NONE', 3,
 ( #21866, #34892, #5723, #14643, #25291, #38295, #9115, #22077, #35104, #17842, #30841, #25707, #19098, #171, #26133, #23121 ),
 .UNSPECIFIED., .F., .F.,
 ( 4, 2, 2, 2, 2, 2, 2, 4 ),
 ( 0.000000000000000000, 0.005276917911546602849, 0.006596147389433264403, 0.007915376867319925958, 0.01055383582309329070, 0.01319229477886665544, 0.01583075373464001845, 0.02110767164618673059 ),
 .UNSPECIFIED. ) ;
#30902 = CARTESIAN_POINT ( 'NONE',  ( 3.905206024139304066, 115.3331674797404247, -1.578293011005953650 ) ) ;
#30903 = CARTESIAN_POINT ( 'NONE',  ( -0.5637839999484974829, 35.87001837459851572, 2.917945788214682423 ) ) ;
#30904 = CARTESIAN_POINT ( 'NONE',  ( -1.153367143837488618, 115.7029425286913238, 1.700742857507489214 ) ) ;
#30905 = CARTESIAN_POINT ( 'NONE',  ( -3.453265078539333288, 21.00871511114837276, -3.102408547967784092 ) ) ;
#30906 = ORIENTED_EDGE ( 'NONE', *, *, #27686, .T. ) ;
#30907 = CARTESIAN_POINT ( 'NONE',  ( -5.314278422745060126, 105.1224610256965235, 0.4583187270701635785 ) ) ;
#30908 = AXIS2_PLACEMENT_3D ( 'NONE', #20107, #15992, #10031 ) ;
#30909 = CARTESIAN_POINT ( 'NONE',  ( 4.539898764682361865, -15.38453816280940778, 0.3562021009913567959 ) ) ;
#30910 = CARTESIAN_POINT ( 'NONE',  ( -0.01152893261320283441, 118.7114655739656257, 0.5769549317675700673 ) ) ;
#30911 = CARTESIAN_POINT ( 'NONE',  ( 0.8015440831811396771, 19.08345756868062892, -0.5584349385947994238 ) ) ;
#30912 = ORIENTED_EDGE ( 'NONE', *, *, #39433, .T. ) ;
#30913 = ORIENTED_EDGE ( 'NONE', *, *, #7649, .T. ) ;
#30914 = CARTESIAN_POINT ( 'NONE',  ( -3.743815577281074614, 31.31851751214970037, -0.6207396561878217867 ) ) ;
#30915 = CARTESIAN_POINT ( 'NONE',  ( 0.5453179846284311738, 107.9696733310005214, 4.488644025489749723 ) ) ;
#30916 =( NAMED_UNIT ( * ) SI_UNIT ( $, .STERADIAN. ) SOLID_ANGLE_UNIT ( ) );
#30917 = CARTESIAN_POINT ( 'NONE',  ( -16.77814054344329620, 146.6545634508490821, 1.109899152166417657 ) ) ;
#30918 = FACE_OUTER_BOUND ( 'NONE', #37393, .T. ) ;
#30919 = ADVANCED_FACE ( 'NONE', ( #39725 ), #10524, .F. ) ;
#30920 = CARTESIAN_POINT ( 'NONE',  ( 4.567598822338898579, 118.0323598375720877, -0.6818831079871943146 ) ) ;
#30921 = CARTESIAN_POINT ( 'NONE',  ( 13.17493328878353509, 125.9194590699508893, -1.341157253524417170 ) ) ;
#30922 = CARTESIAN_POINT ( 'NONE',  ( -11.20355582914615233, 156.1341193432522800, -2.130866455309295748 ) ) ;
#30923 = ADVANCED_FACE ( 'NONE', ( #36106 ), #30124, .T. ) ;
#30924 = EDGE_LOOP ( 'NONE', ( #14811, #37981, #28087, #18700 ) ) ;
#30925 = CARTESIAN_POINT ( 'NONE',  ( 4.416202647269503068, 118.1792123024622896, -0.3908220537550897711 ) ) ;
#30926 = CARTESIAN_POINT ( 'NONE',  ( 7.938918103923345626, 154.5997988942315260, -0.3378123388718580200 ) ) ;
#30927 = EDGE_LOOP ( 'NONE', ( #21037, #25455, #26730, #23, #33703, #27365, #16482, #38028, #7104, #38628, #12845 ) ) ;
#30928 = CARTESIAN_POINT ( 'NONE',  ( 1.978641239374031136, -15.23252017110923795, 5.293569756250467329 ) ) ;
#30929 = DIRECTION ( 'NONE',  ( 0.000000000000000000, 1.000000000000000000, 0.000000000000000000 ) ) ;
#30930 = CARTESIAN_POINT ( 'NONE',  ( -58.52535285190437975, -0.5719483744759017441, 0.2498204902891903723 ) ) ;
#30931 = CARTESIAN_POINT ( 'NONE',  ( 2.990331240142678482, -7.206181497205274233, 3.547999066060627094 ) ) ;
#30932 = CARTESIAN_POINT ( 'NONE',  ( 10.68802918394754897, 123.5542795626547417, 1.432819001183019969 ) ) ;
#30933 = CARTESIAN_POINT ( 'NONE',  ( -0.8015897017430366756, 32.12766266987975428, 3.088637291698237863 ) ) ;
#30934 = CARTESIAN_POINT ( 'NONE',  ( -6.874578817172170453, 121.8312213470058225, 0.01890686361714006766 ) ) ;
#30935 = CARTESIAN_POINT ( 'NONE',  ( -4.515506726787251068, -6.291224493951820484, 1.111903093310195212 ) ) ;
#30936 = CARTESIAN_POINT ( 'NONE',  ( -0.001367086239828292421, 156.3041635968983485, 0.06841458569046213190 ) ) ;
#30937 = CARTESIAN_POINT ( 'NONE',  ( -1.690137127919513649, -8.491432666745847513, 8.270632449787910900 ) ) ;
#30938 = CARTESIAN_POINT ( 'NONE',  ( -57.34787435976332404, 1.552391619547691004, -1.028525222821079960E-14 ) ) ;
#30939 = CARTESIAN_POINT ( 'NONE',  ( 8.789005074032305131, 117.7562713746568193, -0.1097197802411318257 ) ) ;
#30940 = CARTESIAN_POINT ( 'NONE',  ( 0.01046636459289907069, 120.7331730230139755, -0.5237796829255388920 ) ) ;
#30941 = CARTESIAN_POINT ( 'NONE',  ( -6.059261036834482361, 64.39150124418098642, -5.016499999999999737 ) ) ;
#30942 = CARTESIAN_POINT ( 'NONE',  ( 2.008732664060283390, -15.70244684250787870, 5.701976698490780926 ) ) ;
#30943 = FACE_OUTER_BOUND ( 'NONE', #41220, .T. ) ;
#30944 = CARTESIAN_POINT ( 'NONE',  ( 5.270772580891830650, -0.5842219557417941411, -6.616342194954959233 ) ) ;
#30945 = CARTESIAN_POINT ( 'NONE',  ( 5.332911103893867022, 115.7029491485453150, 0.1077752590139453570 ) ) ;
#30946 = DIRECTION ( 'NONE',  ( -5.206863593109713661E-17, 1.000000000000000000, -1.077750396879097183E-30 ) ) ;
#30947 = CARTESIAN_POINT ( 'NONE',  ( 2.460727335429193197, -15.06314154744310585, 4.845259171755021299 ) ) ;
#30948 = CARTESIAN_POINT ( 'NONE',  ( 0.09934209768992387224, 106.7790779034713324, -4.971484795507160825 ) ) ;
#30949 = CARTESIAN_POINT ( 'NONE',  ( -5.835061174465498546, 117.1115750087645608, 0.2489150398414471388 ) ) ;
#30950 = ORIENTED_EDGE ( 'NONE', *, *, #33097, .F. ) ;
#30951 = FACE_OUTER_BOUND ( 'NONE', #13344, .T. ) ;
#30952 = VERTEX_POINT ( 'NONE', #4155 ) ;
#30953 = CARTESIAN_POINT ( 'NONE',  ( -46.93088534759994701, 20.29541677029510893, -5.030633991645946601 ) ) ;
#30954 = CARTESIAN_POINT ( 'NONE',  ( -7.783246152616193569, 154.6561476914895081, -0.1555277812256514736 ) ) ;
#30955 = CARTESIAN_POINT ( 'NONE',  ( 3.779930934242227369, -15.54964480308611208, 5.049599803682278676 ) ) ;
#30956 = CARTESIAN_POINT ( 'NONE',  ( -0.02969037535081191920, 158.7301711276701894, 1.485827791648137497 ) ) ;
#30957 = CARTESIAN_POINT ( 'NONE',  ( 10.29385411648718396, 157.8242135995235458, -0.8711791838966669310 ) ) ;
#30958 = CARTESIAN_POINT ( 'NONE',  ( 3.043391175932955495, 18.63480288530714191, -3.501419995799015528 ) ) ;
#30959 = CARTESIAN_POINT ( 'NONE',  ( -15.60595500976395122, 121.0226940419799462, -0.7351363234501833155 ) ) ;
#30960 = CARTESIAN_POINT ( 'NONE',  ( -50.97644874786027458, 14.69290941399900596, -4.697037614708189146 ) ) ;
#30961 = ORIENTED_EDGE ( 'NONE', *, *, #13127, .F. ) ;
#30962 = CARTESIAN_POINT ( 'NONE',  ( -29.81357423954495189, 70.62209452652477637, -1.524000000000007349 ) ) ;
#30963 = CARTESIAN_POINT ( 'NONE',  ( -30.09725872720941453, 70.36776381375388212, 1.523999999999992250 ) ) ;
#30964 = CARTESIAN_POINT ( 'NONE',  ( -7.383627470571842544, 120.8389031223305352, 0.9130476668403029183 ) ) ;
#30965 = CARTESIAN_POINT ( 'NONE',  ( -56.32662672728373821, 4.077578507741069558, -2.263812825962038033 ) ) ;
#30966 = CARTESIAN_POINT ( 'NONE',  ( 12.45504352496358003, 122.8403290575659526, -1.325700600460794742 ) ) ;
#30967 = CARTESIAN_POINT ( 'NONE',  ( -3.992970410919193025, 117.9114980025989752, -0.8736511219775315862 ) ) ;
#30968 = CARTESIAN_POINT ( 'NONE',  ( -43.83556092231052048, 21.45200552150719631, -2.811646013901254015 ) ) ;
#30969 = EDGE_CURVE ( 'NONE', #2591, #11424, #28929, .T. ) ;
#30970 = CARTESIAN_POINT ( 'NONE',  ( 1.739825554502939076, 156.3676537730497387, -0.7044751146431473821 ) ) ;
#30971 = EDGE_LOOP ( 'NONE', ( #15735, #4446 ) ) ;
#30972 = CARTESIAN_POINT ( 'NONE',  ( -18.24092514812192434, 147.9371514012413229, -2.391122828403475342 ) ) ;
#30973 = CARTESIAN_POINT ( 'NONE',  ( 2.199016089875075686, -15.62526216655714428, 5.252760144517266916 ) ) ;
#30974 = CARTESIAN_POINT ( 'NONE',  ( -4.345421273754075386, 118.1827543097632969, -0.6195030316670109283 ) ) ;
#30975 = CARTESIAN_POINT ( 'NONE',  ( -57.09878488423309051, 3.216020309495956742, -2.217633722229552351 ) ) ;
#30976 = CARTESIAN_POINT ( 'NONE',  ( -4.953655876003494107, 117.5439441053769087, 0.8524319712158592299 ) ) ;
#30977 = CARTESIAN_POINT ( 'NONE',  ( 11.39530606461018358, 123.1738952066917534, 1.661446624139454764 ) ) ;
#30978 = DIRECTION ( 'NONE',  ( -4.017660918040594346E-17, 1.000000000000000000, 2.376309959284834438E-19 ) ) ;
#30979 = CARTESIAN_POINT ( 'NONE',  ( 8.274862188802355689, -1.658786094895864149, -1.630640499628306372 ) ) ;
#30980 = CARTESIAN_POINT ( 'NONE',  ( 15.39048793250114500, 143.5427300040290106, 0.9094471879209009568 ) ) ;
#30981 = CARTESIAN_POINT ( 'NONE',  ( -57.66338803320029882, 2.692357263605615891, -1.869785753600856637 ) ) ;
#30983 = ORIENTED_EDGE ( 'NONE', *, *, #17004, .F. ) ;
#30982 = CARTESIAN_POINT ( 'NONE',  ( -33.42971872652992005, 49.93539301574497102, -1.524000000000005572 ) ) ;
#30984 = DIRECTION ( 'NONE',  ( 1.011795553208986377E-16, 1.000000000000000000, -0.000000000000000000 ) ) ;
#30985 = DIRECTION ( 'NONE',  ( 0.8745520943968235761, -0.4849315768086558398, 4.268512490100410909E-16 ) ) ;
#30986 = CARTESIAN_POINT ( 'NONE',  ( -57.55293229875817218, 1.419684655164468623, 1.132508401016375288 ) ) ;
#30987 = CARTESIAN_POINT ( 'NONE',  ( -50.36444701916330047, 17.30043933429478642, 4.508886934713581596 ) ) ;
#30988 = CARTESIAN_POINT ( 'NONE',  ( -17.17894352244484679, 122.7237354506536491, -0.1767255469942457524 ) ) ;
#30989 = AXIS2_PLACEMENT_3D ( 'NONE', #1228, #20570, #33178 ) ;
#30990 = ORIENTED_EDGE ( 'NONE', *, *, #1565, .F. ) ;
#30991 = CARTESIAN_POINT ( 'NONE',  ( -48.77319768356018415, 22.00425556813275563, -2.071420771163298813 ) ) ;
#30992 = CARTESIAN_POINT ( 'NONE',  ( -5.768081145802491427, 121.1576386676896249, -0.5241667226324177031 ) ) ;
#30993 = CARTESIAN_POINT ( 'NONE',  ( -7.931359276468322506, 121.9896588117074003, 0.6306316981394846088 ) ) ;
#30994 = CARTESIAN_POINT ( 'NONE',  ( 2.857216417531940333, 115.6909491485452577, -1.572722873744161642 ) ) ;
#30995 = CARTESIAN_POINT ( 'NONE',  ( -7.590630008422064812, 122.4062900713904440, -0.3515417406328248395 ) ) ;
#30996 = CARTESIAN_POINT ( 'NONE',  ( 4.144384115003134639, -13.99490941865914806, 4.432938699676250316 ) ) ;
#30997 = CARTESIAN_POINT ( 'NONE',  ( -1.273577801943225785, 159.1407128229522527, 1.197834500974594318 ) ) ;
#30998 = DIRECTION ( 'NONE',  ( -0.9876665170007974393, 0.1565721916417901483, -8.537024980200831679E-16 ) ) ;
#30999 = CARTESIAN_POINT ( 'NONE',  ( 0.9036256862535075873, 116.4850453793277865, 0.1155468115323372985 ) ) ;
#31000 = CARTESIAN_POINT ( 'NONE',  ( -0.0007136890092010687164, 156.3034662015457741, 0.03571591641522637445 ) ) ;
#31001 = CARTESIAN_POINT ( 'NONE',  ( 0.4398701176286285985, 29.43434963188315834, -0.8729469796826672123 ) ) ;
#31002 = CARTESIAN_POINT ( 'NONE',  ( -22.83278390340161934, 150.4073064562084880, -0.5330863269314417563 ) ) ;
#31003 = CARTESIAN_POINT ( 'NONE',  ( 5.008145224984434485, 117.3993836135855418, -0.7758584094373792706 ) ) ;
#31004 = EDGE_CURVE ( 'NONE', #21597, #35463, #17859, .T. ) ;
#31005 = VERTEX_POINT ( 'NONE', #36521 ) ;
#31006 = CARTESIAN_POINT ( 'NONE',  ( -8.094215566179986610, 117.4700539287145631, -0.1617416914405450934 ) ) ;
#31007 = ORIENTED_EDGE ( 'NONE', *, *, #12028, .F. ) ;
#31008 = CARTESIAN_POINT ( 'NONE',  ( 5.962972180698049129, 118.6887585580880398, 1.206927124751090208 ) ) ;
#31009 = DIRECTION ( 'NONE',  ( 0.01876124593811915112, 0.9998239923360757730, 0.000000000000000000 ) ) ;
#31010 = CARTESIAN_POINT ( 'NONE',  ( -0.008945125900511092729, 117.5133074443058945, 0.4476506782301716836 ) ) ;
#31011 = CARTESIAN_POINT ( 'NONE',  ( -58.33068375617585133, -0.2093732065605730108, -0.2478323015014812503 ) ) ;
#31012 = CARTESIAN_POINT ( 'NONE',  ( 6.741874166124438794, 157.8130281244853279, -1.606654124060122424 ) ) ;
#31013 = CARTESIAN_POINT ( 'NONE',  ( -0.7749869142727341398, -12.81603963768374044, -4.556214072895795830 ) ) ;
#31014 = CARTESIAN_POINT ( 'NONE',  ( -21.15273274666908421, 151.2337125027825095, -1.710087910014103985 ) ) ;
#31015 = CARTESIAN_POINT ( 'NONE',  ( 4.747437835475817103, 117.7228179995735502, -0.9150688999438771898 ) ) ;
#31016 = EDGE_CURVE ( 'NONE', #13569, #14379, #4299, .T. ) ;
#31017 = VERTEX_POINT ( 'NONE', #33326 ) ;
#31018 = CARTESIAN_POINT ( 'NONE',  ( -9.164740666424060933, 153.8946005065304803, 0.1038620377607964856 ) ) ;
#31019 = CARTESIAN_POINT ( 'NONE',  ( 4.434149479847604880, -15.45467793902401077, 4.427262213160148896 ) ) ;
#31020 =( BOUNDED_SURFACE ( )  B_SPLINE_SURFACE ( 3, 2, ( 
 ( #20394, #8258, #40450 ),
 ( #14219, #14014, #4668 ),
 ( #20603, #27021, #30416 ),
 ( #7854, #23806, #20814 ),
 ( #33635, #34050, #36826 ),
 ( #10613, #7645, #37235 ),
 ( #14427, #11443, #11241 ),
 ( #27637, #24226, #34260 ),
 ( #4462, #7436, #17419 ),
 ( #4251, #27228, #8054 ),
 ( #17214, #40241, #11036 ),
 ( #24431, #21027, #27434 ),
 ( #1470, #33421, #18041 ),
 ( #30833, #37436, #26812 ),
 ( #840, #39820, #4880 ),
 ( #33840, #1680, #23595 ),
 ( #36617, #9314, #11658 ),
 ( #14844, #31892, #37654 ),
 ( #24864, #2520, #31464 ),
 ( #9108, #21860, #28272 ) ),
 .UNSPECIFIED., .F., .F., .T. ) 
 B_SPLINE_SURFACE_WITH_KNOTS ( ( 4, 2, 2, 2, 2, 2, 2, 2, 2, 4 ),
 ( 3, 3 ),
 ( 1.678480488279121552E-17, 0.0008043537003518050343, 0.001608707400703593372, 0.002413061101055381710, 0.003217414801407169830, 0.004021768501758958385, 0.004826122202110746939, 0.006434829602814323181, 0.009652244404221476531, 0.01286965920562862901 ),
 ( 0.000000000000000000, 1.000000000000000000 ),
 .UNSPECIFIED. ) 
 GEOMETRIC_REPRESENTATION_ITEM ( )  RATIONAL_B_SPLINE_SURFACE ( (
 ( 1.000000000000000000, 0.9815197824473206323, 1.000000000000000000),
 ( 1.000000000000000000, 0.9811767838555041088, 1.000000000000000000),
 ( 1.000000000000000000, 0.9804039767733835342, 1.000000000000000000),
 ( 1.000000000000000000, 0.9775760511973242695, 1.000000000000000000),
 ( 1.000000000000000000, 0.9755247961224483566, 1.000000000000000000),
 ( 1.000000000000000000, 0.9705275854478995212, 1.000000000000000000),
 ( 1.000000000000000000, 0.9675790768618311999, 1.000000000000000000),
 ( 1.000000000000000000, 0.9611010073753046834, 1.000000000000000000),
 ( 1.000000000000000000, 0.9576315359795163351, 1.000000000000000000),
 ( 1.000000000000000000, 0.9503812888595358777, 1.000000000000000000),
 ( 1.000000000000000000, 0.9466096088198014957, 1.000000000000000000),
 ( 1.000000000000000000, 0.9387890754370313839, 1.000000000000000000),
 ( 1.000000000000000000, 0.9347210935246765828, 1.000000000000000000),
 ( 1.000000000000000000, 0.9222591698861631881, 1.000000000000000000),
 ( 1.000000000000000000, 0.9133676415844801388, 1.000000000000000000),
 ( 1.000000000000000000, 0.8858621071945419478, 1.000000000000000000),
 ( 1.000000000000000000, 0.8667308185384640096, 1.000000000000000000),
 ( 1.000000000000000000, 0.8330124393854519971, 1.000000000000000000),
 ( 1.000000000000000000, 0.8190729568363664947, 1.000000000000000000),
 ( 1.000000000000000000, 0.8123912451051847894, 1.000000000000000000) ) ) 
 REPRESENTATION_ITEM ( '' )  SURFACE ( )  );
#31021 = CARTESIAN_POINT ( 'NONE',  ( -6.405903822259908509, 29.15797647828624406, 0.04789268291063029231 ) ) ;
#31022 = AXIS2_PLACEMENT_3D ( 'NONE', #11502, #2150, #21702 ) ;
#31023 = CARTESIAN_POINT ( 'NONE',  ( -2.549993051094809449, 117.9496054164201695, -1.337954177656600407 ) ) ;
#31024 = ADVANCED_FACE ( 'NONE', ( #7550 ), #11753, .T. ) ;
#31026 = ORIENTED_EDGE ( 'NONE', *, *, #38287, .F. ) ;
#31025 = AXIS2_PLACEMENT_3D ( 'NONE', #38443, #12858, #35043 ) ;
#31027 = CARTESIAN_POINT ( 'NONE',  ( 17.42401203395154141, 135.4862447717955547, 2.417378365323842981 ) ) ;
#31028 = CARTESIAN_POINT ( 'NONE',  ( 10.92199999999999704, 55.24500000000000455, -3.904382278571533962E-15 ) ) ;
#31029 = DIRECTION ( 'NONE',  ( -0.000000000000000000, -0.000000000000000000, -1.000000000000000000 ) ) ;
#31030 = CARTESIAN_POINT ( 'NONE',  ( -0.7241986523584001967, 107.9696733310005214, 4.463276061801071393 ) ) ;
#31031 = CARTESIAN_POINT ( 'NONE',  ( -4.294125178196657622, -12.16697637372164564, -7.253078015393731981 ) ) ;
#31032 = CARTESIAN_POINT ( 'NONE',  ( 10.97991518849985759, 126.1652090859982707, 0.9941924553172261092 ) ) ;
#31033 = CARTESIAN_POINT ( 'NONE',  ( -4.792076001792309192, 115.6909491485453003, -1.475558552157980818 ) ) ;
#31034 = CARTESIAN_POINT ( 'NONE',  ( 22.71566531765381569, 150.0520759213295889, -0.3958359165339124797 ) ) ;
#31035 = ADVANCED_FACE ( 'NONE', ( #32906 ), #10314, .F. ) ;
#31036 = CARTESIAN_POINT ( 'NONE',  ( 5.511275327877898533, 57.15000000000044622, -5.111309965977538283 ) ) ;
#31037 = CARTESIAN_POINT ( 'NONE',  ( -58.36850749721234877, -0.2888827900911983271, 0.04284473868145901448 ) ) ;
#31038 = CARTESIAN_POINT ( 'NONE',  ( 5.177913976931214357, 57.15000000000004832, 5.372099999999999653 ) ) ;
#31039 = CARTESIAN_POINT ( 'NONE',  ( -49.76517000418316172, 16.66822512019472313, 4.974244438740138108 ) ) ;
#31040 = ADVANCED_FACE ( 'NONE', ( #32477, #23073 ), #6708, .T. ) ;
#31041 = DIRECTION ( 'NONE',  ( 4.017660918040594346E-17, -1.000000000000000000, -2.376309959284834438E-19 ) ) ;
#31042 = CARTESIAN_POINT ( 'NONE',  ( -4.241115207526993558, 118.2240460336109464, 0.3200252020677880616 ) ) ;
#31043 = CARTESIAN_POINT ( 'NONE',  ( 3.682264917456192332, 88.48546620154573361, 0.07358041635423968885 ) ) ;
#31044 = ORIENTED_EDGE ( 'NONE', *, *, #33247, .T. ) ;
#31045 = CARTESIAN_POINT ( 'NONE',  ( -50.11792632901008915, 17.09067799859288783, 5.048577231237564966 ) ) ;
#31046 = CARTESIAN_POINT ( 'NONE',  ( -6.136200860584644090, 119.6162947413529025, -1.249506624868057969 ) ) ;
#31047 = CARTESIAN_POINT ( 'NONE',  ( -4.973569738608247803, 117.3993868453981548, -0.9750659555622913643 ) ) ;
#31048 = CARTESIAN_POINT ( 'NONE',  ( 4.250260335411498502, 118.2244068006796169, 0.4633496807658996075 ) ) ;
#31049 = CARTESIAN_POINT ( 'NONE',  ( -7.664053125822943180, 122.2986020547093915, -0.5896768268545020675 ) ) ;
#31050 = DIRECTION ( 'NONE',  ( 0.01997839162482749342, 1.040247600000944484E-18, -0.9998004120163608288 ) ) ;
#31051 = CARTESIAN_POINT ( 'NONE',  ( 17.31377588638417819, 122.7721875394316555, 0.3459704467065362055 ) ) ;
#31052 = ADVANCED_FACE ( 'NONE', ( #3737 ), #16695, .T. ) ;
#31053 = EDGE_LOOP ( 'NONE', ( #34545, #17710, #4440, #41358, #619 ) ) ;
#31054 = CARTESIAN_POINT ( 'NONE',  ( 1.141857472271699425, 24.90688314728939190, 4.478778191171412182 ) ) ;
#31055 = CARTESIAN_POINT ( 'NONE',  ( -16.71293428529044078, 146.3384789841921361, -1.780605135160314045 ) ) ;
#31056 = DIRECTION ( 'NONE',  ( 0.000000000000000000, -1.000000000000000000, 0.000000000000000000 ) ) ;
#31057 = DIRECTION ( 'NONE',  ( -5.206863593109713661E-17, 1.000000000000000000, -1.077750396879097183E-30 ) ) ;
#31058 = CIRCLE ( 'NONE', #36516, 0.3809999999999984510 ) ;
#31059 = CARTESIAN_POINT ( 'NONE',  ( -5.309060684617390516E-14, 83.56599999999998829, 0.000000000000000000 ) ) ;
#31060 = CARTESIAN_POINT ( 'NONE',  ( 6.069820211534818100, 121.4363512089535249, 0.2627894127678002678 ) ) ;
#31061 = CARTESIAN_POINT ( 'NONE',  ( -0.2501726036287156840, 25.39126883368370002, -4.616104092076634302 ) ) ;
#31062 = CARTESIAN_POINT ( 'NONE',  ( 22.48407052889629654, 149.9757045183965261, 1.524144198737067857 ) ) ;
#31063 = CARTESIAN_POINT ( 'NONE',  ( -29.82321757229076908, 71.17901112636586447, -1.270000000000007123 ) ) ;
#31065 = CARTESIAN_POINT ( 'NONE',  ( 4.947803190686594021, 118.0342071775839941, -0.7636311594363673905 ) ) ;
#31064 = CARTESIAN_POINT ( 'NONE',  ( 2.768784035434307178, -15.00486597294339930, 4.394545281259884639 ) ) ;
#31066 = CARTESIAN_POINT ( 'NONE',  ( -8.076210525097467396, 156.3870133935118076, 1.723082682300313806 ) ) ;
#31067 = CARTESIAN_POINT ( 'NONE',  ( -2.714482067202859561, 26.26591195808746448, -3.750338772627290762 ) ) ;
#31068 = CARTESIAN_POINT ( 'NONE',  ( 0.008148259816488066104, 159.5682499516715040, -0.4077722408685185429 ) ) ;
#31069 = CARTESIAN_POINT ( 'NONE',  ( 0.9467939684353117169, 21.72092434492431323, 0.2316696090552467224 ) ) ;
#31070 = VERTEX_POINT ( 'NONE', #26286 ) ;
#31071 = CARTESIAN_POINT ( 'NONE',  ( -52.94148447887670272, 9.133269539094115430, 0.6394659809470414347 ) ) ;
#31072 = CARTESIAN_POINT ( 'NONE',  ( -7.714568708787910012, 122.2455405838764335, 0.3552802434219702321 ) ) ;
#31073 = CARTESIAN_POINT ( 'NONE',  ( 5.309946395046844181, -12.59883844183437596, 1.960244440597288529 ) ) ;
#31074 = CARTESIAN_POINT ( 'NONE',  ( 0.02400040557466523797, 156.7459281804771365, -1.201078436782489600 ) ) ;
#31075 = EDGE_LOOP ( 'NONE', ( #36941, #1313, #22400, #29757 ) ) ;
#31076 = CIRCLE ( 'NONE', #10671, 0.6350000000000001199 ) ;
#31077 = CARTESIAN_POINT ( 'NONE',  ( 1.198181792750290464, 115.7029448766258781, 1.741964538748038027 ) ) ;
#31078 = ORIENTED_EDGE ( 'NONE', *, *, #11250, .F. ) ;
#31079 = CARTESIAN_POINT ( 'NONE',  ( 2.120958618816386920, -15.04726689571640819, 5.287964242625700528 ) ) ;
#31080 = CARTESIAN_POINT ( 'NONE',  ( -4.682896055009653224, 117.8402614876679309, -1.032663334385100384 ) ) ;
#31081 = CARTESIAN_POINT ( 'NONE',  ( 9.076946558997631698, 124.0722828908287454, 0.1472919029216551157 ) ) ;
#31082 = ORIENTED_EDGE ( 'NONE', *, *, #28468, .T. ) ;
#31083 = CARTESIAN_POINT ( 'NONE',  ( 8.818906024077392658, 119.8693228481767932, 1.468947216590822391 ) ) ;
#31084 = MECHANICAL_DESIGN_GEOMETRIC_PRESENTATION_REPRESENTATION (  '', ( #41382 ), #6621 ) ;
#31085 = CARTESIAN_POINT ( 'NONE',  ( -6.603988835907287056E-14, 91.53346620154573543, -3.493462572467304738E-18 ) ) ;
#31086 = CARTESIAN_POINT ( 'NONE',  ( -4.476425760464393555, 71.61790547347303004, -1.523999999999994248 ) ) ;
#31087 = ADVANCED_FACE ( 'NONE', ( #748 ), #35897, .F. ) ;
#31088 = VECTOR ( 'NONE', #31193, 1000.000000000000000 ) ;
#31089 = CARTESIAN_POINT ( 'NONE',  ( 15.61624682818904297, 120.8175431576145940, 0.1535658744814574483 ) ) ;
#31090 = EDGE_CURVE ( 'NONE', #2471, #11710, #11777, .T. ) ;
#31091 = DIRECTION ( 'NONE',  ( -5.188838149069472160E-16, 1.699382548006136559E-16, 1.000000000000000000 ) ) ;
#31092 = CARTESIAN_POINT ( 'NONE',  ( 1.782359092197000061, -15.48430479490869871, 5.418275911098993980 ) ) ;
#31093 = CARTESIAN_POINT ( 'NONE',  ( -45.67973391888839529, 25.66060799623228661, 1.523999999999991806 ) ) ;
#31094 = CARTESIAN_POINT ( 'NONE',  ( -3.682264917456323339, 75.78546620154573077, -0.07358041635423923088 ) ) ;
#31095 = CARTESIAN_POINT ( 'NONE',  ( -4.777430207200964674, 117.8484153795353393, 0.7997178450909804281 ) ) ;
#31096 = ORIENTED_EDGE ( 'NONE', *, *, #21909, .F. ) ;
#31097 = ORIENTED_EDGE ( 'NONE', *, *, #102, .T. ) ;
#31098 = CARTESIAN_POINT ( 'NONE',  ( -16.02764313970816090, 80.34763903973272647, 1.523999999999997579 ) ) ;
#31099 = EDGE_CURVE ( 'NONE', #17114, #21064, #36942, .T. ) ;
#31100 = CARTESIAN_POINT ( 'NONE',  ( 8.570152792252320850, 118.9011554048343129, -0.9064097239879936874 ) ) ;
#31101 = CARTESIAN_POINT ( 'NONE',  ( -5.278237183132178600, 122.2451909684448310, -0.2611397421478203751 ) ) ;
#31102 = CARTESIAN_POINT ( 'NONE',  ( 4.707096360283405723, 117.7228093591007365, 1.103996979757269514 ) ) ;
#31103 = CARTESIAN_POINT ( 'NONE',  ( -11.55299880265461887, 55.57741982016710125, -4.472382752598250910 ) ) ;
#31104 = CARTESIAN_POINT ( 'NONE',  ( -1.034729067459851271, 124.2655319029901335, 0.03890078971358925525 ) ) ;
#31105 = CIRCLE ( 'NONE', #36565, 0.6350000000000014522 ) ;
#31106 = CARTESIAN_POINT ( 'NONE',  ( 1.686640475165922748, -9.627085671684914914, -4.319569293544198274 ) ) ;
#31107 = EDGE_CURVE ( 'NONE', #31688, #33162, #4371, .T. ) ;
#31108 = CARTESIAN_POINT ( 'NONE',  ( -56.90590057130552282, 4.418898835881354792, 2.427662546266514454 ) ) ;
#31109 = CARTESIAN_POINT ( 'NONE',  ( -19.68500000000000227, 71.11999999999999034, 5.016499999999999737 ) ) ;
#31110 = CARTESIAN_POINT ( 'NONE',  ( 3.015147157152042290, -12.41699557045261670, 0.4662733852003331791 ) ) ;
#31111 = CARTESIAN_POINT ( 'NONE',  ( 3.689824518792477637, 110.1236525333376619, -3.433021159709686909 ) ) ;
#31112 = CARTESIAN_POINT ( 'NONE',  ( -3.748619050207897985, 28.91994025391836942, 2.520532616727765518 ) ) ;
#31113 = CARTESIAN_POINT ( 'NONE',  ( -1.240271560838381637, 115.7029491485453576, 1.694587172447594936 ) ) ;
#31114 = CARTESIAN_POINT ( 'NONE',  ( -2.707926769430928804, 11.08828375386998033, -3.745406074561137277 ) ) ;
#31115 = ORIENTED_EDGE ( 'NONE', *, *, #4066, .F. ) ;
#31116 = CARTESIAN_POINT ( 'NONE',  ( -4.078417157467525200, 104.6144662015457811, -2.601001456789872712 ) ) ;
#31117 = CARTESIAN_POINT ( 'NONE',  ( 4.228667402019948618, -15.40433107038223426, 0.8683934293704824725 ) ) ;
#31118 = CARTESIAN_POINT ( 'NONE',  ( -11.07050914993725677, 156.0189320485970086, 1.715486126203028538 ) ) ;
#31119 = CARTESIAN_POINT ( 'NONE',  ( 0.7511875256325919459, -11.68598654017788974, 0.6195722450943603743 ) ) ;
#31120 = CARTESIAN_POINT ( 'NONE',  ( 0.7678286665867425365, 17.13787758575863762, 0.6011479000593502597 ) ) ;
#31121 = ORIENTED_EDGE ( 'NONE', *, *, #30382, .T. ) ;
#31122 = ORIENTED_EDGE ( 'NONE', *, *, #33425, .F. ) ;
#31123 = PLANE ( 'NONE',  #27621 ) ;
#31124 = CIRCLE ( 'NONE', #12663, 0.2540000000000004476 ) ;
#31125 = CARTESIAN_POINT ( 'NONE',  ( -0.1065646865916383135, 105.8844662015456777, 5.332932678536313809 ) ) ;
#31126 = CARTESIAN_POINT ( 'NONE',  ( -9.244484035386584253, 123.0263237342149978, 0.6646791600263458610 ) ) ;
#31127 = CARTESIAN_POINT ( 'NONE',  ( -25.81615557310160369, 74.46796499802707103, 1.523999999999993582 ) ) ;
#31128 = CARTESIAN_POINT ( 'NONE',  ( 1.897380780832740532, -15.05783359004129984, 5.662421594695133287 ) ) ;
#31129 = CARTESIAN_POINT ( 'NONE',  ( 8.333011053690729142, 121.0263440914440736, -1.031464938890432004 ) ) ;
#31130 = CARTESIAN_POINT ( 'NONE',  ( -19.83855703208276466, 148.9191654756151024, -2.494779984669014183 ) ) ;
#31131 = CARTESIAN_POINT ( 'NONE',  ( -3.671158984043940170E-14, 57.78499999999999659, 0.000000000000000000 ) ) ;
#31132 = CARTESIAN_POINT ( 'NONE',  ( 4.123150137924818992, 118.2429491485453354, -0.1807919990337682747 ) ) ;
#31133 = CARTESIAN_POINT ( 'NONE',  ( 7.065481736843126193, 122.0164807696326790, -0.1187983231582534355 ) ) ;
#31134 = ORIENTED_EDGE ( 'NONE', *, *, #10952, .F. ) ;
#31135 = CARTESIAN_POINT ( 'NONE',  ( 1.822811606207361823, -15.29362660170947841, 5.402418844745947801 ) ) ;
#31136 = CARTESIAN_POINT ( 'NONE',  ( -3.521685918548247418, 29.33394459973516888, 3.031038535435704340 ) ) ;
#31137 = AXIS2_PLACEMENT_3D ( 'NONE', #5421, #28191, #31811 ) ;
#31138 = CARTESIAN_POINT ( 'NONE',  ( -58.39415239746359276, -0.3126312442514861401, 0.4522786855634189918 ) ) ;
#31139 = CARTESIAN_POINT ( 'NONE',  ( 4.587442282481145384, -5.694351208059624803, -0.5507456681084095251 ) ) ;
#31140 = CARTESIAN_POINT ( 'NONE',  ( 0.7656893570837772778, 156.6562795458349910, 1.120391489380295535 ) ) ;
#31141 = CARTESIAN_POINT ( 'NONE',  ( 0.8489375256178871565, 34.04538252295368039, 1.759639877157939347 ) ) ;
#31142 = CARTESIAN_POINT ( 'NONE',  ( -7.618479139564732883, 124.9344662015457317, -0.1522353441811853947 ) ) ;
#31143 = CARTESIAN_POINT ( 'NONE',  ( -2.948169924849943335, 1.592661447142720732, -3.562413953034572867 ) ) ;
#31144 = CARTESIAN_POINT ( 'NONE',  ( 11.82813386268891165, 130.3161362890850512, 0.2363542639706544268 ) ) ;
#31145 = CARTESIAN_POINT ( 'NONE',  ( 3.560122487986403517, 2.076091768892780909, 7.630420683349803390 ) ) ;
#31146 = CARTESIAN_POINT ( 'NONE',  ( -57.99953387342350908, 0.4830015814202143209, -0.7353922615980251765 ) ) ;
#31147 = CARTESIAN_POINT ( 'NONE',  ( -5.523483301223560460, 116.8734833957022090, -0.5481978220757582898 ) ) ;
#31148 = DIRECTION ( 'NONE',  ( -0.9998004120163608288, 0.000000000000000000, -0.01997839162482749342 ) ) ;
#31149 = CARTESIAN_POINT ( 'NONE',  ( -43.82859865241511699, 24.63416949198730421, -1.524000000000006905 ) ) ;
#31150 = CARTESIAN_POINT ( 'NONE',  ( -5.591489108514605455, 77.73497692594764885, 1.270000000000002238 ) ) ;
#31151 = CARTESIAN_POINT ( 'NONE',  ( 2.739727753987758252, 28.35525327666260864, -3.728201022356329553 ) ) ;
#31152 = ADVANCED_FACE ( 'NONE', ( #20935 ), #37555, .T. ) ;
#31153 = CARTESIAN_POINT ( 'NONE',  ( 4.299309211086679738, 118.1588881536522564, 0.6869296180760711135 ) ) ;
#31154 = DIRECTION ( 'NONE',  ( 0.9998004120163609398, 0.000000000000000000, 0.01997839162482749689 ) ) ;
#31155 = DIRECTION ( 'NONE',  ( -0.8745520943968250194, 0.4849315768086532863, -5.361993529360574930E-16 ) ) ;
#31156 = CARTESIAN_POINT ( 'NONE',  ( 0.8039382690412617549, 120.8419495465347069, -0.4447074479469316222 ) ) ;
#31157 = CARTESIAN_POINT ( 'NONE',  ( -22.28323889858847195, 137.0232865695268458, 0.2611169771296155684 ) ) ;
#31158 = EDGE_LOOP ( 'NONE', ( #38822, #34002, #30783, #39670 ) ) ;
#31159 = CARTESIAN_POINT ( 'NONE',  ( -58.16194989728257525, 1.772972946764567181, -0.08436090182518581060 ) ) ;
#31160 = ORIENTED_EDGE ( 'NONE', *, *, #5289, .T. ) ;
#31161 = CARTESIAN_POINT ( 'NONE',  ( -46.39387867998599546, 20.78226312412258991, -4.747706454273081356 ) ) ;
#31162 = CARTESIAN_POINT ( 'NONE',  ( -0.6474952184382374298, 120.9973616653156512, 0.02013384967883425844 ) ) ;
#31163 = CARTESIAN_POINT ( 'NONE',  ( 4.283822907657564016, -15.48171044555848930, 4.591852530049981063 ) ) ;
#31164 = CARTESIAN_POINT ( 'NONE',  ( -13.43626322254348260, 155.6061939908119882, 1.534180175809178648 ) ) ;
#31165 = CARTESIAN_POINT ( 'NONE',  ( 1.044861395163911411, 117.1967307433898640, -0.4172573962433456796 ) ) ;
#31166 = CARTESIAN_POINT ( 'NONE',  ( 4.458631606973747274, 16.91056413504885825, 1.251853190366734259 ) ) ;
#31167 = CARTESIAN_POINT ( 'NONE',  ( -23.02690842483890066, 149.8694456586574972, -0.9127416204503945307 ) ) ;
#31168 = CARTESIAN_POINT ( 'NONE',  ( -50.20358007252900734, 15.96865141398877697, -4.880505329357888833 ) ) ;
#31169 = EDGE_LOOP ( 'NONE', ( #13369, #29191, #3423, #22874 ) ) ;
#31170 = CARTESIAN_POINT ( 'NONE',  ( 8.789531458490529303, 117.7096508578360101, 0.3423636166664316693 ) ) ;
#31171 = FACE_OUTER_BOUND ( 'NONE', #40723, .T. ) ;
#31172 = CARTESIAN_POINT ( 'NONE',  ( -0.02768739821015298377, 156.9833357668885014, 1.385590625008459087 ) ) ;
#31173 = CARTESIAN_POINT ( 'NONE',  ( -53.66578727863507225, 9.481950398213415454, -3.598112444201927662 ) ) ;
#31174 = CARTESIAN_POINT ( 'NONE',  ( 17.50667431346010972, 135.4862447717955547, -1.719380121689204177 ) ) ;
#31175 = CARTESIAN_POINT ( 'NONE',  ( -13.87194369518297599, 121.7708260186165177, -1.632391212143505799 ) ) ;
#31176 = CARTESIAN_POINT ( 'NONE',  ( -50.11792632901008915, 17.09067799859288783, -5.048577231237582730 ) ) ;
#31177 = CARTESIAN_POINT ( 'NONE',  ( 13.84625834149330359, 134.3516747369166069, -0.8047173373260269047 ) ) ;
#31178 = EDGE_LOOP ( 'NONE', ( #11242, #14555, #10341, #27528 ) ) ;
#31179 = CARTESIAN_POINT ( 'NONE',  ( -17.50950237657583131, 148.8653046532945723, -2.321071487785774767 ) ) ;
#31180 = CARTESIAN_POINT ( 'NONE',  ( 3.954393197012034733, -15.56809308616131915, 2.853032214330836869 ) ) ;
#31181 = CARTESIAN_POINT ( 'NONE',  ( -4.448382910831185200, 118.1283983457245625, -0.7237973005349965794 ) ) ;
#31182 = CARTESIAN_POINT ( 'NONE',  ( -58.33777482027510786, 1.113448835244251756, -1.208045587469442017 ) ) ;
#31183 = CARTESIAN_POINT ( 'NONE',  ( -4.828569062062975092, 117.4060461567800786, 1.008118597039231235 ) ) ;
#31184 = CARTESIAN_POINT ( 'NONE',  ( 7.383155613640851378, 155.9567503867590972, 1.861932028473976208 ) ) ;
#31185 = CARTESIAN_POINT ( 'NONE',  ( -3.628388194583719468E-14, 57.78499999999999659, 1.904999999999999805 ) ) ;
#31186 = CARTESIAN_POINT ( 'NONE',  ( -6.853500063829680577, -7.707324007402828414, -4.930749982112237362 ) ) ;
#31187 = CARTESIAN_POINT ( 'NONE',  ( 12.24221062544593153, 130.6044139104978115, 0.7866602228194184976 ) ) ;
#31188 = LINE ( 'NONE', #41218, #11294 ) ;
#31189 = TOROIDAL_SURFACE ( 'NONE', #19636, 3.683000000000000718, 0.5080000000000000071 ) ;
#31191 = ORIENTED_EDGE ( 'NONE', *, *, #12507, .T. ) ;
#31190 = CARTESIAN_POINT ( 'NONE',  ( -44.27221412529542022, 20.06621383160478445, -0.8981538560692819972 ) ) ;
#31192 = CARTESIAN_POINT ( 'NONE',  ( 0.3822965766165241086, 105.7854827256092420, -5.327377110122780479 ) ) ;
#31193 = DIRECTION ( 'NONE',  ( 0.000000000000000000, 1.000000000000000000, 0.000000000000000000 ) ) ;
#31194 = CARTESIAN_POINT ( 'NONE',  ( -58.18636467486479091, 0.07352994790495170907, 0.3924542439260513826 ) ) ;
#31195 = CARTESIAN_POINT ( 'NONE',  ( -50.72152632752359125, 17.59631655692102470, 3.767527310968340704 ) ) ;
#31196 = CARTESIAN_POINT ( 'NONE',  ( -6.908764576387383727, 117.1865127098105575, -0.01035743554829984120 ) ) ;
#31197 = EDGE_LOOP ( 'NONE', ( #36682, #16606, #14353, #32687 ) ) ;
#31198 = CARTESIAN_POINT ( 'NONE',  ( -50.10414895690885828, 20.83497401302349061, -1.621381026025509708 ) ) ;
#31199 = CARTESIAN_POINT ( 'NONE',  ( 5.943351980717774374, 121.3891827933073557, -0.07897414172417135947 ) ) ;
#31200 = CARTESIAN_POINT ( 'NONE',  ( -8.511289907599598692, 119.1972314554215302, 1.000383355283217757 ) ) ;
#31201 = EDGE_LOOP ( 'NONE', ( #3919, #6523, #30375, #16033 ) ) ;
#31202 = CARTESIAN_POINT ( 'NONE',  ( 3.205182831369184804, 118.7629491485453741, -1.047990948762189456 ) ) ;
#31203 = CARTESIAN_POINT ( 'NONE',  ( -4.265939155585104281, 155.8374496918941077, -0.3214930909109445234 ) ) ;
#31204 = CARTESIAN_POINT ( 'NONE',  ( 5.472227756958008449, -13.43587746834383445, 2.852490916751204697 ) ) ;
#31205 = CARTESIAN_POINT ( 'NONE',  ( -21.57210427006343423, 149.5883454796168621, 1.274511887596345039 ) ) ;
#31206 = CARTESIAN_POINT ( 'NONE',  ( 7.213960532363567602, 83.56599999999998829, 1.904999999999995364 ) ) ;
#31207 = CARTESIAN_POINT ( 'NONE',  ( 23.20201897184725226, 149.6253602407241488, 0.6175280007103176594 ) ) ;
#31208 = CARTESIAN_POINT ( 'NONE',  ( 4.218275339060157059, 155.8585684991085714, 0.08429118021179421438 ) ) ;
#31209 = CARTESIAN_POINT ( 'NONE',  ( -4.988560382155355022, 117.5941865341327741, 0.6973410046930860196 ) ) ;
#31210 = CARTESIAN_POINT ( 'NONE',  ( 0.6255416438669687551, 26.40915095058528905, 0.7518939258676016202 ) ) ;
#31211 = CARTESIAN_POINT ( 'NONE',  ( -23.44243449907619237, 146.8400249081559537, -0.5456528120549730687 ) ) ;
#31212 = CARTESIAN_POINT ( 'NONE',  ( -46.44929266343369534, 20.74717589152057329, -4.783910049210099658 ) ) ;
#31213 = FACE_OUTER_BOUND ( 'NONE', #9957, .T. ) ;
#31214 = ORIENTED_EDGE ( 'NONE', *, *, #36060, .F. ) ;
#31215 = CARTESIAN_POINT ( 'NONE',  ( 3.622559830352364507, 117.9414738143271109, 0.9055989021787060889 ) ) ;
#31216 = DIRECTION ( 'NONE',  ( -0.8745520943968245753, 0.4849315768086539524, -5.691349986800526185E-16 ) ) ;
#31217 = CARTESIAN_POINT ( 'NONE',  ( 19.51124600060703784, 152.2820370773569323, 1.942483913431542364 ) ) ;
#31218 = CARTESIAN_POINT ( 'NONE',  ( -48.15691857873192561, 19.01861963077412199, -5.213839621096282961 ) ) ;
#31219 = CARTESIAN_POINT ( 'NONE',  ( 0.4495176323322074285, 118.2558431149878402, -0.5768950177939177193 ) ) ;
#31220 = CARTESIAN_POINT ( 'NONE',  ( 8.093748642744952093, 23.43776531741863423, -2.407353130276413733 ) ) ;
#31221 = CARTESIAN_POINT ( 'NONE',  ( -22.07943683853339323, 148.3267584643486146, -2.032026126618132089 ) ) ;
#31222 = CARTESIAN_POINT ( 'NONE',  ( 4.861667474615974704, 117.7348714202375248, -0.8247141752807952697 ) ) ;
#31223 = CARTESIAN_POINT ( 'NONE',  ( 3.903247448917655849, 109.8183322527596602, 3.677532532511333052 ) ) ;
#31224 = ORIENTED_EDGE ( 'NONE', *, *, #36551, .T. ) ;
#31225 = CARTESIAN_POINT ( 'NONE',  ( -0.002459394113084579191, 156.3065584682211124, 0.1230781383047673677 ) ) ;
#31226 = CARTESIAN_POINT ( 'NONE',  ( -12.62197313556529110, 122.7135068550949200, -1.834144044656287109 ) ) ;
#31228 = CARTESIAN_POINT ( 'NONE',  ( 2.058067359092986326, -15.63668844659656187, 5.842422791592841946 ) ) ;
#31227 = AXIS2_PLACEMENT_3D ( 'NONE', #25024, #8847, #2474 ) ;
#31229 = CIRCLE ( 'NONE', #25118, 7.461249999999999716 ) ;
#31230 = CARTESIAN_POINT ( 'NONE',  ( 13.77279150232676130, 16.85108474679722690, -5.016499999999997961 ) ) ;
#31231 = CARTESIAN_POINT ( 'NONE',  ( -3.153262279070554897, 117.9496044432466419, -1.302034589134676068 ) ) ;
#31232 = ORIENTED_EDGE ( 'NONE', *, *, #6581, .T. ) ;
#31233 = CARTESIAN_POINT ( 'NONE',  ( 2.358209769532786382, 119.0637060312156024, 0.7902384042126602282 ) ) ;
#31234 = CARTESIAN_POINT ( 'NONE',  ( -5.332935381406168851, 115.7029491485442634, -0.1065653510733624160 ) ) ;
#31235 = CARTESIAN_POINT ( 'NONE',  ( -4.834697789094183129, 118.7629491485453599, 0.4653049473571303496 ) ) ;
#31236 = CARTESIAN_POINT ( 'NONE',  ( -1.603046668355913917, 118.6366899268033279, 0.8036507178775276206 ) ) ;
#31237 = CARTESIAN_POINT ( 'NONE',  ( 7.363685156731384573, -6.572911479292511849, 4.144591825403105112 ) ) ;
#31238 = CARTESIAN_POINT ( 'NONE',  ( 15.82363114525486836, 143.7482200480382346, 1.443160993194752217 ) ) ;
#31239 = FACE_OUTER_BOUND ( 'NONE', #4367, .T. ) ;
#31240 = CARTESIAN_POINT ( 'NONE',  ( 14.93494801707985609, 120.8072429308574414, -0.3831319127562621274 ) ) ;
#31241 = CARTESIAN_POINT ( 'NONE',  ( 5.638141748386683361, 56.51499999999961688, -5.060111600422207090 ) ) ;
#31242 = CARTESIAN_POINT ( 'NONE',  ( -58.36779176277465808, -0.2873857612693362373, 0.05403644662055718390 ) ) ;
#31243 = DIRECTION ( 'NONE',  ( -5.188838149069471174E-16, 1.699382548006136313E-16, 1.000000000000000000 ) ) ;
#31244 = ADVANCED_FACE ( 'NONE', ( #18158 ), #36502, .T. ) ;
#31245 = EDGE_CURVE ( 'NONE', #26949, #19837, #21255, .T. ) ;
#31246 = DIRECTION ( 'NONE',  ( -5.188838149069471174E-16, 1.699382548006136313E-16, 1.000000000000000000 ) ) ;
#31248 = CARTESIAN_POINT ( 'NONE',  ( -4.116494434418081383, 118.2429491485453354, 0.1883380258390151551 ) ) ;
#31247 = AXIS2_PLACEMENT_3D ( 'NONE', #33354, #1195, #10756 ) ;
#31249 = LINE ( 'NONE', #8478, #4345 ) ;
#31250 = ORIENTED_EDGE ( 'NONE', *, *, #261, .T. ) ;
#31251 = CARTESIAN_POINT ( 'NONE',  ( -51.54051843738712080, 14.84038450301108192, 4.692172599169413871 ) ) ;
#31252 = CIRCLE ( 'NONE', #25814, 16.60960244842765832 ) ;
#31253 = CARTESIAN_POINT ( 'NONE',  ( -6.150511332855731261, 119.6465158254115835, -1.246810306309521943 ) ) ;
#31254 = CARTESIAN_POINT ( 'NONE',  ( -5.336395407662996249, 116.0444662015457169, 0.06658830643601890142 ) ) ;
#31255 = CARTESIAN_POINT ( 'NONE',  ( 4.364698422493899166, 118.1847547154890208, 0.6011634615692652561 ) ) ;
#31256 = CARTESIAN_POINT ( 'NONE',  ( 0.004350076772674690319, 120.7058980590201429, -0.2176956299261763039 ) ) ;
#31257 = DIRECTION ( 'NONE',  ( 9.627370216492862708E-17, 1.000000000000000000, -0.000000000000000000 ) ) ;
#31258 = CARTESIAN_POINT ( 'NONE',  ( 9.822473411059192472, 117.9943479623217399, 0.1962763949404991992 ) ) ;
#31259 = EDGE_LOOP ( 'NONE', ( #9360, #2387, #11521, #33615, #40866, #134, #19421 ) ) ;
#31260 = CARTESIAN_POINT ( 'NONE',  ( -0.01876340930523686876, 19.73428105357427853, -4.634220987317214657 ) ) ;
#31261 = DIRECTION ( 'NONE',  ( 5.188838149069472160E-16, -1.699382548006136559E-16, -1.000000000000000000 ) ) ;
#31262 = CARTESIAN_POINT ( 'NONE',  ( -25.56614996202194590, 73.65611136973726047, 1.269999999999993578 ) ) ;
#31263 = CARTESIAN_POINT ( 'NONE',  ( -41.52577271625691679, 22.97115911878592343, 1.523999999999989807 ) ) ;
#31264 = FACE_OUTER_BOUND ( 'NONE', #6259, .T. ) ;
#31265 = CARTESIAN_POINT ( 'NONE',  ( 6.989608668544338599, 121.8932936631570669, 0.4001562091357755979 ) ) ;
#31266 = CARTESIAN_POINT ( 'NONE',  ( -3.618988008572157522, 19.14412854911201123, 2.900346660497036044 ) ) ;
#31267 = CARTESIAN_POINT ( 'NONE',  ( 22.60558431049191697, 149.7032342875954498, 1.528355188309250545 ) ) ;
#31268 = CARTESIAN_POINT ( 'NONE',  ( 4.780938538460484111, 104.6144662015456959, -0.7305874870394178933 ) ) ;
#31270 = CARTESIAN_POINT ( 'NONE',  ( 15.01775385910449145, 123.1914926142276130, -1.125269324988861896 ) ) ;
#31269 = CARTESIAN_POINT ( 'NONE',  ( 1.824654213811243819, -15.25386490109567639, 5.420715704377902178 ) ) ;
#31271 = CARTESIAN_POINT ( 'NONE',  ( -18.38987645279124550, 147.6341482083243761, 1.661003423535650558 ) ) ;
#31272 = CARTESIAN_POINT ( 'NONE',  ( -1.512449008193210931, 25.81601926892489018, -4.382106060783010903 ) ) ;
#31273 = CARTESIAN_POINT ( 'NONE',  ( -16.56062761363025970, 155.2525159475892167, -1.104293791145709802 ) ) ;
#31274 = CARTESIAN_POINT ( 'NONE',  ( 0.9735350199255810022, 12.44701472381428609, 0.02964292050307446719 ) ) ;
#31275 = EDGE_LOOP ( 'NONE', ( #23971, #22740 ) ) ;
#31276 = CARTESIAN_POINT ( 'NONE',  ( -57.41561397472474937, 1.705883423724310788, 1.231064337386900354 ) ) ;
#31277 = CARTESIAN_POINT ( 'NONE',  ( -4.393282770141167859, 155.8497297829079571, 0.4427821657071677741 ) ) ;
#31278 = CARTESIAN_POINT ( 'NONE',  ( 5.341062828015524566, -12.45213391371734168, 1.712110018432928982 ) ) ;
#31279 = CARTESIAN_POINT ( 'NONE',  ( 10.62684080304149603, 123.4307455932968765, -0.9978443992970126297 ) ) ;
#31280 = ORIENTED_EDGE ( 'NONE', *, *, #7178, .T. ) ;
#31281 = CARTESIAN_POINT ( 'NONE',  ( 0.7313781531325286300, 115.7029491485453292, 1.756327035003194981 ) ) ;
#31282 = B_SPLINE_CURVE_WITH_KNOTS ( 'NONE', 3,
 ( #31460, #31677, #3510, #16680, #6904, #12080, #18670, #2517, #28482, #23267 ),
 .UNSPECIFIED., .F., .F.,
 ( 4, 2, 2, 2, 4 ),
 ( 0.007397145391538724121, 0.008407694387831695856, 0.009418243384124665857, 0.01042879238041763759, 0.01143934137671060933 ),
 .UNSPECIFIED. ) ;
#31283 = CARTESIAN_POINT ( 'NONE',  ( -4.641629919619552957, 117.8847811183079841, -1.004318260171652266 ) ) ;
#31284 = ADVANCED_FACE ( 'NONE', ( #2638, #15175 ), #22394, .F. ) ;
#31285 = CARTESIAN_POINT ( 'NONE',  ( 8.074187567048884517, 122.8559727437779827, 0.08249527776860611505 ) ) ;
#31286 = AXIS2_PLACEMENT_3D ( 'NONE', #18496, #15520, #34505 ) ;
#31287 = ORIENTED_EDGE ( 'NONE', *, *, #5270, .F. ) ;
#31288 = CARTESIAN_POINT ( 'NONE',  ( 19.82367009662574375, 149.5711785761137662, 2.459487706365388604 ) ) ;
#31289 = CARTESIAN_POINT ( 'NONE',  ( 1.561582345843624431, 156.2588034088681184, 0.03120413162939523685 ) ) ;
#31290 = CARTESIAN_POINT ( 'NONE',  ( -23.75997692595333177, 82.67351089148900201, 1.269999999999992912 ) ) ;
#31291 = DIRECTION ( 'NONE',  ( -0.8745520943968235761, 0.4849315768086558398, -5.691349986800547879E-16 ) ) ;
#31292 = CARTESIAN_POINT ( 'NONE',  ( 23.25537431167556690, 149.3282167461061931, 0.1335628131362695814 ) ) ;
#31293 = CARTESIAN_POINT ( 'NONE',  ( 0.03707542933077223601, 115.3931862868688398, -1.855406091731502505 ) ) ;
#31294 = CARTESIAN_POINT ( 'NONE',  ( 1.989440554114935145, -15.14293609156945664, 5.899323384112847179 ) ) ;
#31295 = CARTESIAN_POINT ( 'NONE',  ( 10.28897677580357950, 56.51500000000000057, 4.381499999999999950 ) ) ;
#31296 = CARTESIAN_POINT ( 'NONE',  ( -11.53797084252497207, 82.58007221317646440, -1.524000000000000021 ) ) ;
#31297 = CARTESIAN_POINT ( 'NONE',  ( -4.657380072211783073, 117.9834161660140381, 0.7123224875277872625 ) ) ;
#31298 = B_SPLINE_SURFACE_WITH_KNOTS ( 'NONE', 3, 3, ( 
 ( #31456, #2300, #18666, #40848, #28048 ),
 ( #2513, #41057, #11867, #15477, #24856 ),
 ( #39956, #33346, #20744, #27568, #37366 ),
 ( #8185, #1605, #4176, #20319, #1393 ),
 ( #14563, #14349, #17754, #33560, #30754 ),
 ( #17139, #36961, #4803, #13946, #23515 ),
 ( #36749, #30140, #40577, #1186, #24152 ),
 ( #30968, #981, #20531, #26944, #4594 ),
 ( #34183, #10749, #33975, #39748, #23730 ),
 ( #17350, #7570, #10956, #21153, #37161 ),
 ( #11168, #27360, #36543, #14148, #14770 ),
 ( #4394, #40163, #30338, #27151, #40372 ),
 ( #23943, #11374, #24361, #7783, #33769 ),
 ( #17553, #7361, #5009, #17970, #1809 ),
 ( #30554, #7982, #10546, #20951, #19017 ),
 ( #15406, #2017, #41416, #24998, #21782 ),
 ( #21998, #12222, #31390, #31176, #8607 ),
 ( #25428, #15612, #28196, #41202, #34597 ),
 ( #35230, #38429, #27982, #27772, #5850 ),
 ( #24784, #12006, #22201, #14981, #9243 ),
 ( #11581, #5426, #28617, #37782, #40783 ),
 ( #31607, #6057, #31816, #2445, #18805 ),
 ( #2654, #24566, #21359, #37998, #35030 ),
 ( #37570, #21569, #18382, #34385, #5219 ),
 ( #38217, #18173, #2233, #41628, #2861 ),
 ( #32023, #15193, #12435, #8397, #8822 ),
 ( #34808, #5641, #40990, #28410, #18599 ),
 ( #25214, #11793, #9033, #12639, #6675 ),
 ( #19437, #16235, #41843, #25626, #13267 ),
 ( #3701, #7102, #39049, #509, #32443 ),
 ( #29239, #13482, #26251, #294, #29455 ),
 ( #39261, #10278, #36070, #10067, #29028 ),
 ( #3070, #35434, #32655, #6258, #16028 ),
 ( #23039, #42047, #12844, #38636, #38839 ),
 ( #6886, #39473, #32869, #16661, #25829 ),
 ( #28829, #9855, #20063, #9648, #3491 ),
 ( #19855, #13049, #22825, #29668, #22615 ),
 ( #26470, #35862, #19641, #35649, #16449 ),
 ( #6463, #23248, #9441, #26040, #32238 ) ),
 .UNSPECIFIED., .F., .F., .F.,
 ( 4, 1, 1, 1, 1, 1, 1, 1, 1, 1, 1, 2, 1, 1, 1, 1, 1, 1, 1, 1, 1, 1, 1, 1, 1, 1, 1, 1, 1, 1, 1, 1, 1, 1, 1, 4 ),
 ( 4, 1, 4 ),
 ( 0.000000000000000000, 0.01653533301974152367, 0.03307066603948304734, 0.04960599905922460223, 0.06614133207896609468, 0.08267666509870763569, 0.09921199811844919059, 0.1322826641579321894, 0.1653533301974152714, 0.1984239962368983812, 0.2314946622763813522, 0.2645653283158643787, 0.3105299952961229071, 0.3335123287862520880, 0.3564946622763812689, 0.4024593292566397418, 0.4484239962368982702, 0.4943886632171566875, 0.5403533301974150493, 0.5863179971776735222, 0.6322826641579321061, 0.6782473311381906900, 0.7242119981184491628, 0.7701766650987074136, 0.8161413320789658865, 0.8621059990592241373, 0.8735971658042887000, 0.8850883325493537068, 0.8965794992944182695, 0.9080706660394826102, 0.9195618327845473949, 0.9310529995296121797, 0.9425441662746769644, 0.9540353330197415271, 0.9770176665098706525, 1.000000000000000000 ),
 ( 0.000000000000000000, 0.5000000000000000000, 1.000000000000000000 ),
 .UNSPECIFIED. ) ;
#31299 = ORIENTED_EDGE ( 'NONE', *, *, #14169, .T. ) ;
#31300 = VERTEX_POINT ( 'NONE', #28180 ) ;
#31301 = CARTESIAN_POINT ( 'NONE',  ( 5.174194766718689387, 115.7029491485453150, -1.071326111713503559 ) ) ;
#31302 = CARTESIAN_POINT ( 'NONE',  ( 3.046135264910829754, 118.1726090481387814, -0.7595472998034786816 ) ) ;
#31303 = CARTESIAN_POINT ( 'NONE',  ( -4.758673294993353231, 116.4582014290525507, -1.187054331573000665 ) ) ;
#31305 = CARTESIAN_POINT ( 'NONE',  ( 4.796259625824248474, 117.7368196676605265, 1.049688617138287317 ) ) ;
#31304 = AXIS2_PLACEMENT_3D ( 'NONE', #37478, #27481, #11487 ) ;
#31306 = CARTESIAN_POINT ( 'NONE',  ( -11.48503488083589730, 55.92196062030022574, -5.016499999999890491 ) ) ;
#31307 = CARTESIAN_POINT ( 'NONE',  ( -0.3929232564621699120, 123.1683257372383054, 0.1777898040562597426 ) ) ;
#31308 = CYLINDRICAL_SURFACE ( 'NONE', #4994, 2.540000000000002256 ) ;
#31309 = CARTESIAN_POINT ( 'NONE',  ( -17.09698261757901960, 84.43312239790384410, 1.269999999999995355 ) ) ;
#31310 = CARTESIAN_POINT ( 'NONE',  ( 3.682264917456191888, 101.6934662015457320, 0.07358041635423968885 ) ) ;
#31311 = CARTESIAN_POINT ( 'NONE',  ( 3.325379330704291814, -12.45968715000887705, 0.9553361148970926919 ) ) ;
#31312 = CARTESIAN_POINT ( 'NONE',  ( 6.118667329349966266, 121.4157903421748301, -0.08376844782033862624 ) ) ;
#31313 = CARTESIAN_POINT ( 'NONE',  ( -17.50701641564917921, 146.6691408387931688, -2.165841098895500583 ) ) ;
#31314 = EDGE_CURVE ( 'NONE', #27648, #35654, #21919, .T. ) ;
#31315 = DIRECTION ( 'NONE',  ( -0.9998501190848636533, -0.01731298258487590572, 2.898946086000287674E-15 ) ) ;
#31316 = DIRECTION ( 'NONE',  ( 5.188838149069472160E-16, -1.699382548006136559E-16, -1.000000000000000000 ) ) ;
#31317 = CARTESIAN_POINT ( 'NONE',  ( -48.28978369826177186, 19.63653578263564015, -5.206999999995405304 ) ) ;
#31318 = CARTESIAN_POINT ( 'NONE',  ( 2.801506786573456420, 9.139157206818806500, -3.684590140147142368 ) ) ;
#31320 = ORIENTED_EDGE ( 'NONE', *, *, #11735, .F. ) ;
#31319 = CARTESIAN_POINT ( 'NONE',  ( 14.58714721168222006, 120.3300541288867862, 0.7025926276034526463 ) ) ;
#31321 = CARTESIAN_POINT ( 'NONE',  ( 2.186726956427079926, 104.6144662015457243, -4.302861239856920150 ) ) ;
#31322 = CARTESIAN_POINT ( 'NONE',  ( 4.535010020878385895, -15.35856548043400238, 0.06517018677027014428 ) ) ;
#31323 = CARTESIAN_POINT ( 'NONE',  ( -0.01147819631912393688, 118.8623374019222894, 0.5744158801423953076 ) ) ;
#31324 = CARTESIAN_POINT ( 'NONE',  ( -0.4283232389533950801, 25.18001705023179326, -0.8778289364919926729 ) ) ;
#31325 = CIRCLE ( 'NONE', #14988, 3.683000000000001162 ) ;
#31326 = CARTESIAN_POINT ( 'NONE',  ( 0.4606059098249736805, 26.09511874640634943, 0.8667040019166204479 ) ) ;
#31327 = ORIENTED_EDGE ( 'NONE', *, *, #5930, .T. ) ;
#31328 = ORIENTED_EDGE ( 'NONE', *, *, #34455, .F. ) ;
#31329 = FACE_BOUND ( 'NONE', #32265, .T. ) ;
#31330 = CARTESIAN_POINT ( 'NONE',  ( 1.673685645604575445, 111.6436615656963909, 3.078281589618439895 ) ) ;
#31331 = CARTESIAN_POINT ( 'NONE',  ( -9.903729432088850260, 123.6875948057429895, 0.6970279851166614193 ) ) ;
#31332 = EDGE_CURVE ( 'NONE', #5382, #37727, #15111, .T. ) ;
#31333 = DIRECTION ( 'NONE',  ( -0.7071067811865479058, -0.7071067811865472397, 8.659560562354936556E-17 ) ) ;
#31334 = CARTESIAN_POINT ( 'NONE',  ( 3.604966970014626959, -13.82400766246429136, 3.906450875976586801 ) ) ;
#31335 = CARTESIAN_POINT ( 'NONE',  ( 14.02613073054668824, 152.5802402909829425, -1.631301951249304993 ) ) ;
#31336 = CARTESIAN_POINT ( 'NONE',  ( -5.840405771877655638, 118.8996324090661147, -1.179527747254400349 ) ) ;
#31337 = DIRECTION ( 'NONE',  ( -1.000000000000000000, 0.000000000000000000, 0.000000000000000000 ) ) ;
#31338 = AXIS2_PLACEMENT_3D ( 'NONE', #2857, #29025, #41840 ) ;
#31339 = CARTESIAN_POINT ( 'NONE',  ( -15.21351360038804579, 143.4186079242267340, -0.3040022078858841126 ) ) ;
#31340 = CARTESIAN_POINT ( 'NONE',  ( 4.074910602682932925, 118.2429491485453354, -0.1454311599470142491 ) ) ;
#31341 = CARTESIAN_POINT ( 'NONE',  ( 15.88665273169769598, 145.7686330500600036, -0.2792794258574998745 ) ) ;
#31342 = ORIENTED_EDGE ( 'NONE', *, *, #27207, .T. ) ;
#31343 = CARTESIAN_POINT ( 'NONE',  ( 2.915559332840946816, -14.19431184016030301, 0.3483797586856177686 ) ) ;
#31344 = CARTESIAN_POINT ( 'NONE',  ( -5.994056581265662363E-14, 72.48346620154573827, 9.856484473772818746E-17 ) ) ;
#31345 = EDGE_CURVE ( 'NONE', #25690, #500, #22616, .T. ) ;
#31346 = VECTOR ( 'NONE', #13005, 1000.000000000000000 ) ;
#31347 = DIRECTION ( 'NONE',  ( -0.9876665170007974393, 0.1565721916417901483, -8.537024980200831679E-16 ) ) ;
#31348 = EDGE_CURVE ( 'NONE', #2461, #40395, #41185, .T. ) ;
#31349 = CARTESIAN_POINT ( 'NONE',  ( -49.26674734213751350, 17.44270459986665145, 5.073646373251102126 ) ) ;
#31350 = CARTESIAN_POINT ( 'NONE',  ( -3.942997264624582776, -11.51663297089948479, -2.426127359622226809 ) ) ;
#31351 = CARTESIAN_POINT ( 'NONE',  ( 0.5640265924886082027, 120.2131932824006526, 0.4111470527632634098 ) ) ;
#31352 = CARTESIAN_POINT ( 'NONE',  ( -3.640095369667306180, 28.17176065243310390, 0.7113786998093643010 ) ) ;
#31353 = CARTESIAN_POINT ( 'NONE',  ( -0.1065646865916160396, 105.8844662015456777, 5.332932678536313809 ) ) ;
#31354 = CARTESIAN_POINT ( 'NONE',  ( 4.224370802630715183, -2.505441902618962935, 1.893578447770203566 ) ) ;
#31355 = CARTESIAN_POINT ( 'NONE',  ( 10.39928917620358817, 153.1223395828141918, 0.2078025466733119664 ) ) ;
#31356 = ADVANCED_FACE ( 'NONE', ( #15598 ), #20551, .T. ) ;
#31357 = CARTESIAN_POINT ( 'NONE',  ( -6.277010209292351206, 0.1250379130781943404, 5.629075605414042727 ) ) ;
#31358 = CARTESIAN_POINT ( 'NONE',  ( -57.70855261479918141, 1.142328357490882240, -1.228565355106010504 ) ) ;
#31359 = CARTESIAN_POINT ( 'NONE',  ( 8.786181581555666753, 117.7732179722915618, -0.1423289417060864537 ) ) ;
#31360 = CARTESIAN_POINT ( 'NONE',  ( -0.9836305199215028550, 123.5966405200008325, -0.1412250206608574310 ) ) ;
#31361 = CARTESIAN_POINT ( 'NONE',  ( -6.096037513970403054, 78.08166987308820239, -1.523999999999996247 ) ) ;
#31362 = DIRECTION ( 'NONE',  ( -0.9998004120163609398, 0.000000000000000000, -0.01997839162482749689 ) ) ;
#31363 = CARTESIAN_POINT ( 'NONE',  ( -8.412600736458745843, -6.831223903669816799, -0.4304377746521336201 ) ) ;
#31364 = CARTESIAN_POINT ( 'NONE',  ( 3.960059183279624140, 117.9394489435469211, 1.233284679773928971 ) ) ;
#31365 = PLANE ( 'NONE',  #38914 ) ;
#31366 = DIRECTION ( 'NONE',  ( 0.9998004120163608288, 0.000000000000000000, 0.01997839162482749342 ) ) ;
#31367 = CARTESIAN_POINT ( 'NONE',  ( 0.7689147969092013923, 119.5055576915191580, -0.7020325503247994980 ) ) ;
#31368 = CARTESIAN_POINT ( 'NONE',  ( -23.19190728264284829, 146.6831645211815101, 0.2733909575703943884 ) ) ;
#31369 = ORIENTED_EDGE ( 'NONE', *, *, #15522, .F. ) ;
#31370 = CARTESIAN_POINT ( 'NONE',  ( -58.82374062945601167, -0.06097470622967726683, -0.2234658159562166180 ) ) ;
#31371 = ORIENTED_EDGE ( 'NONE', *, *, #18005, .F. ) ;
#31372 = CARTESIAN_POINT ( 'NONE',  ( -16.71197878298170991, 83.87086364642222236, -1.270000000000002682 ) ) ;
#31374 = CARTESIAN_POINT ( 'NONE',  ( -15.77133435453296606, 146.5691041611200660, -0.3151487940933135334 ) ) ;
#31373 = AXIS2_PLACEMENT_3D ( 'NONE', #21844, #31029, #31451 ) ;
#31375 = CARTESIAN_POINT ( 'NONE',  ( 5.567940837815767097, -14.86657585147074734, 2.969021103613282531 ) ) ;
#31376 = CARTESIAN_POINT ( 'NONE',  ( -16.52101850268839200, 153.5550899668227203, 1.581448849539220269 ) ) ;
#31377 = CARTESIAN_POINT ( 'NONE',  ( 15.08259856265889809, 121.6710330000183546, -0.7362983101480767845 ) ) ;
#31378 = CARTESIAN_POINT ( 'NONE',  ( -4.492784857928645792, 12.16275517495587977, -1.104450737933446725 ) ) ;
#31379 = CARTESIAN_POINT ( 'NONE',  ( -23.20196384716143001, 149.3105122542552863, -0.9177021184322480263 ) ) ;
#31380 = EDGE_CURVE ( 'NONE', #15239, #9633, #22185, .T. ) ;
#31381 = CARTESIAN_POINT ( 'NONE',  ( -50.27159791831159197, 15.85842796992063164, -4.865305682342245142 ) ) ;
#31382 = ADVANCED_FACE ( 'NONE', ( #35215 ), #36946, .T. ) ;
#31383 = ORIENTED_EDGE ( 'NONE', *, *, #31589, .F. ) ;
#31384 = CARTESIAN_POINT ( 'NONE',  ( -8.798408483647307321, 117.6899343870790631, -0.1004539260620418706 ) ) ;
#31385 = DIRECTION ( 'NONE',  ( 0.1728608224830406603, 0.000000000000000000, -0.9849462604886047856 ) ) ;
#31386 = CARTESIAN_POINT ( 'NONE',  ( -0.5497817020643304131, 119.7690751942239729, 0.4902208388216632851 ) ) ;
#31387 = CARTESIAN_POINT ( 'NONE',  ( -49.16865371179721933, 17.52875052363311070, -5.029076361559855712 ) ) ;
#31388 = CARTESIAN_POINT ( 'NONE',  ( 15.01676740740983007, 152.9649416503947634, -1.747251348416147820 ) ) ;
#31389 = CARTESIAN_POINT ( 'NONE',  ( -10.54454712121203741, 119.9085704333771787, -1.450830856784145917 ) ) ;
#31390 = CARTESIAN_POINT ( 'NONE',  ( -49.93490050754573417, 16.96705409125581099, -5.170188367178254474 ) ) ;
#31391 = CARTESIAN_POINT ( 'NONE',  ( 5.210205730215608178, 121.0352659167314755, -0.3424523703800271823 ) ) ;
#31392 = VERTEX_POINT ( 'NONE', #2845 ) ;
#31393 = CARTESIAN_POINT ( 'NONE',  ( -17.91131452944958014, 148.1388135707062474, -2.335088068787735782 ) ) ;
#31394 = CARTESIAN_POINT ( 'NONE',  ( 1.897852064921616622, -15.54654116324019597, 5.408738352340563438 ) ) ;
#31395 = AXIS2_PLACEMENT_3D ( 'NONE', #31471, #30842, #15064 ) ;
#31396 = CARTESIAN_POINT ( 'NONE',  ( 4.825036788390894671, 51.14746620154573264, 0.09641571798141809757 ) ) ;
#31397 = AXIS2_PLACEMENT_3D ( 'NONE', #11556, #24540, #8371 ) ;
#31398 = EDGE_CURVE ( 'NONE', #34293, #2670, #5664, .T. ) ;
#31399 = CARTESIAN_POINT ( 'NONE',  ( -57.67794393518098417, 1.927849678527493449, -1.763631237166056520 ) ) ;
#31400 = ADVANCED_FACE ( 'NONE', ( #22809 ), #13466, .T. ) ;
#31401 = CARTESIAN_POINT ( 'NONE',  ( -4.815275531776046947, 117.4047736241515736, 1.012442419610674271 ) ) ;
#31402 = CARTESIAN_POINT ( 'NONE',  ( 17.60198365394328590, 148.3509993576462307, 2.281626375285575659 ) ) ;
#31403 = CARTESIAN_POINT ( 'NONE',  ( -5.586884702347497900, 136.3644662015457527, -0.1116392523995361485 ) ) ;
#31404 = CIRCLE ( 'NONE', #13036, 0.2540000000000000036 ) ;
#31405 = CARTESIAN_POINT ( 'NONE',  ( -3.848622047617309860, 1.169161361801722032, -7.524129562738414378 ) ) ;
#31406 = CARTESIAN_POINT ( 'NONE',  ( 9.155891339183860111, 123.9989874199980022, 0.4132670667758964744 ) ) ;
#31407 = CARTESIAN_POINT ( 'NONE',  ( 1.949857553418792744, 118.1238931878471448, -0.8604232605442251325 ) ) ;
#31408 = CARTESIAN_POINT ( 'NONE',  ( -23.24761240069422286, 77.83567810938664877, -1.270000000000005125 ) ) ;
#31409 = CARTESIAN_POINT ( 'NONE',  ( -1.138279655186107187, 117.9394518318250107, 1.346695663613399097 ) ) ;
#31410 = CARTESIAN_POINT ( 'NONE',  ( -57.43854689232674815, 1.757847328446624058, 1.624773336220232789 ) ) ;
#31411 = PLANE ( 'NONE',  #40627 ) ;
#31412 = CARTESIAN_POINT ( 'NONE',  ( -6.615214180512292604E-14, 94.32746620154571815, -2.829521569843129660E-18 ) ) ;
#31413 = CARTESIAN_POINT ( 'NONE',  ( -48.88162864671050301, 20.15829640254822408, 3.957548906738488803 ) ) ;
#31414 = CARTESIAN_POINT ( 'NONE',  ( -21.55438672983833825, 132.6250929350426020, -0.2276674992303580614 ) ) ;
#31415 = ORIENTED_EDGE ( 'NONE', *, *, #27436, .F. ) ;
#31416 = CARTESIAN_POINT ( 'NONE',  ( -48.20156657701303970, 19.76063879377972654, -5.201425424509408479 ) ) ;
#31417 = CARTESIAN_POINT ( 'NONE',  ( -6.029124040440666299, 121.4385140814827651, -0.1554332074001965880 ) ) ;
#31418 = DIRECTION ( 'NONE',  ( 5.188838149069472160E-16, -1.699382548006136559E-16, -1.000000000000000000 ) ) ;
#31419 = EDGE_LOOP ( 'NONE', ( #10145, #34590, #30293, #3492 ) ) ;
#31420 = CARTESIAN_POINT ( 'NONE',  ( 2.215630398121276823, 118.7629491485453883, -1.137602048208893768 ) ) ;
#31421 = CARTESIAN_POINT ( 'NONE',  ( -6.012785076883673696, 155.3544091381320982, -0.3765917842305991914 ) ) ;
#31422 = CARTESIAN_POINT ( 'NONE',  ( 4.441035242322985965, -14.03446645907663282, 4.353459135924754086 ) ) ;
#31423 = CARTESIAN_POINT ( 'NONE',  ( -20.51279501983856690, 150.9797539340098069, 1.282250019969888077 ) ) ;
#31424 = CARTESIAN_POINT ( 'NONE',  ( 5.285751105924014759, 78.93631598568867958, -5.267410652559297191 ) ) ;
#31425 = VECTOR ( 'NONE', #18359, 1000.000000000000000 ) ;
#31426 = CARTESIAN_POINT ( 'NONE',  ( 21.59686147024584102, 132.6646020023713959, 0.5653344646799389750 ) ) ;
#31427 = CARTESIAN_POINT ( 'NONE',  ( 15.72253002844083447, 146.8976288395060124, 0.3811693606321951422 ) ) ;
#31428 = FACE_OUTER_BOUND ( 'NONE', #29388, .T. ) ;
#31429 = CARTESIAN_POINT ( 'NONE',  ( -0.4102451260098727293, 24.68626973166569982, 0.8857237506759965129 ) ) ;
#31430 = CARTESIAN_POINT ( 'NONE',  ( -13.67522198567664482, 119.6429072192227494, -0.3220992662749118107 ) ) ;
#31431 = CARTESIAN_POINT ( 'NONE',  ( -42.38674010915296009, 22.29968555344163761, -1.779698089469653466 ) ) ;
#31432 = DIRECTION ( 'NONE',  ( 0.9998004120163608288, 0.000000000000000000, 0.01997839162482736852 ) ) ;
#31433 = ORIENTED_EDGE ( 'NONE', *, *, #34997, .T. ) ;
#31434 = CARTESIAN_POINT ( 'NONE',  ( -4.022005995279760882, 118.2573117515256911, 0.8180388012835972944 ) ) ;
#31435 = DIRECTION ( 'NONE',  ( 4.017660918040594346E-17, -1.000000000000000000, -2.376309959284834438E-19 ) ) ;
#31436 = CARTESIAN_POINT ( 'NONE',  ( 16.77501307560209654, 125.2521365416322254, 1.703383479906432685 ) ) ;
#31437 = CARTESIAN_POINT ( 'NONE',  ( 2.242939865367092001, 118.2767885243204944, -0.6835633642702234614 ) ) ;
#31438 = CARTESIAN_POINT ( 'NONE',  ( -7.074087999897446188, 26.91573472731666783, -4.615267515785972385 ) ) ;
#31439 = CARTESIAN_POINT ( 'NONE',  ( -22.29769713523688779, 148.9358926463403918, -1.890714429241201699 ) ) ;
#31440 = CARTESIAN_POINT ( 'NONE',  ( 4.866058426851059160, 117.6757764595213018, -0.8743054753177306182 ) ) ;
#31441 = CARTESIAN_POINT ( 'NONE',  ( 5.028795574735070772, 114.3519703858145959, 1.961426316196308361 ) ) ;
#31442 = CARTESIAN_POINT ( 'NONE',  ( -14.69813734295233232, 148.8396455022467535, -0.06702550439777849034 ) ) ;
#31443 = CARTESIAN_POINT ( 'NONE',  ( -16.83022555070514770, 151.2926467857828072, -2.419188160499602613 ) ) ;
#31444 = AXIS2_PLACEMENT_3D ( 'NONE', #10923, #23913, #36929 ) ;
#31445 = CARTESIAN_POINT ( 'NONE',  ( 4.355571528211143573, -15.30747929803376373, 4.711715777764150737 ) ) ;
#31446 = CARTESIAN_POINT ( 'NONE',  ( -6.571239715384261478E-14, 88.48546620154573361, -1.207165459146770882E-19 ) ) ;
#31447 = CARTESIAN_POINT ( 'NONE',  ( -1.551677701541317234, 118.1651005044952285, -0.8611336031554802650 ) ) ;
#31448 = ORIENTED_EDGE ( 'NONE', *, *, #10721, .F. ) ;
#31449 = CARTESIAN_POINT ( 'NONE',  ( 5.029336563146884487, 119.5555251685854330, 1.067692183578045073 ) ) ;
#31450 = CARTESIAN_POINT ( 'NONE',  ( -17.14500000000466784, 71.11999999999886768, 1.523999999999998689 ) ) ;
#31451 = DIRECTION ( 'NONE',  ( -1.000000000000000000, 0.000000000000000000, 0.000000000000000000 ) ) ;
#31452 = AXIS2_PLACEMENT_3D ( 'NONE', #31372, #21765, #16013 ) ;
#31453 = CARTESIAN_POINT ( 'NONE',  ( -2.219425127536600151, 123.7320667226965867, 0.04105829392232424740 ) ) ;
#31454 = CARTESIAN_POINT ( 'NONE',  ( -7.958381229837070414, -11.09356959825496247, -2.748999415197344476 ) ) ;
#31455 = CARTESIAN_POINT ( 'NONE',  ( 6.199776539618373938, 155.3658059236344684, 0.8002054381730366872 ) ) ;
#31456 = CARTESIAN_POINT ( 'NONE',  ( -41.05189575270516400, 23.09451173561986081, -1.524000000000003130 ) ) ;
#31457 = CARTESIAN_POINT ( 'NONE',  ( 1.382728874883415449, 159.5452856091935132, -0.4834108180186508230 ) ) ;
#31458 = CARTESIAN_POINT ( 'NONE',  ( 5.322311914403613287, 56.51499999999978030, -5.239113282919442227 ) ) ;
#31459 = CARTESIAN_POINT ( 'NONE',  ( -58.05678064718770770, 0.3813734126662043922, 0.7812039021332745081 ) ) ;
#31460 = CARTESIAN_POINT ( 'NONE',  ( 7.213960532367366341, 78.77618639008778700, 1.904999999999999583 ) ) ;
#31461 = CARTESIAN_POINT ( 'NONE',  ( -6.571239715384261478E-14, 88.48546620154573361, -1.207165459146770882E-19 ) ) ;
#31462 = CARTESIAN_POINT ( 'NONE',  ( -4.119378102468195912, 118.2429491485453354, 0.1851105702619638971 ) ) ;
#31463 = CIRCLE ( 'NONE', #32823, 0.6349999999999969003 ) ;
#31464 = CARTESIAN_POINT ( 'NONE',  ( 5.219047500496350800, 114.8007926982748614, -1.212193980527778603 ) ) ;
#31465 = EDGE_LOOP ( 'NONE', ( #17836, #8778, #5163, #41708, #1242 ) ) ;
#31466 = CARTESIAN_POINT ( 'NONE',  ( -52.30895062419047292, 13.66434875625866674, 4.401212925246481333 ) ) ;
#31467 = CARTESIAN_POINT ( 'NONE',  ( 8.274444664989344389, 120.3629719553960769, -1.109322312946052103 ) ) ;
#31468 = CARTESIAN_POINT ( 'NONE',  ( 4.304052292061569140, 104.6144662015457385, -3.992357259174772466 ) ) ;
#31469 = CARTESIAN_POINT ( 'NONE',  ( -2.729962743039006323, 120.7841308545065431, -0.3244322735474264308 ) ) ;
#31470 = CARTESIAN_POINT ( 'NONE',  ( -5.586884702347496123, 87.97746620154572383, -0.1116392523995361624 ) ) ;
#31471 = CARTESIAN_POINT ( 'NONE',  ( 17.14499999999999957, 71.11999999999999034, -1.904999999999999583 ) ) ;
#31472 = ORIENTED_EDGE ( 'NONE', *, *, #21654, .F. ) ;
#31473 = CARTESIAN_POINT ( 'NONE',  ( 4.203610184846851894, 17.99761390031315500, -1.968029828111186319 ) ) ;
#31474 = CARTESIAN_POINT ( 'NONE',  ( -29.04966993605376047, 66.62533279659477614, 1.523999999999992916 ) ) ;
#31475 = DIRECTION ( 'NONE',  ( 5.188838149069472160E-16, -1.699382548006136559E-16, -1.000000000000000000 ) ) ;
#31476 = CARTESIAN_POINT ( 'NONE',  ( 7.127785904777375059, 78.78377652171666057, -2.231330898844071875 ) ) ;
#31477 = DIRECTION ( 'NONE',  ( -4.017660918040594346E-17, 1.000000000000000000, 2.376309959284834438E-19 ) ) ;
#31478 = CARTESIAN_POINT ( 'NONE',  ( -6.991984101104667282, 121.9387022086022654, -0.02476450050892398808 ) ) ;
#31479 = CARTESIAN_POINT ( 'NONE',  ( 2.233585966345281282, 24.54162662436292308, -4.064490141941544898 ) ) ;
#31480 = CARTESIAN_POINT ( 'NONE',  ( 3.857972943339615046, 117.0975898859979054, 0.5726864223607190940 ) ) ;
#31481 = CARTESIAN_POINT ( 'NONE',  ( -1.939077340875614341, 104.6144662015454543, -4.428395887593343794 ) ) ;
#31483 = CARTESIAN_POINT ( 'NONE',  ( 21.30706188252186450, 149.4807732621110006, -1.383641861344254931 ) ) ;
#31482 = CARTESIAN_POINT ( 'NONE',  ( 2.349528287245666647, -15.15257587461875310, 4.947206973663434759 ) ) ;
#31484 = CARTESIAN_POINT ( 'NONE',  ( -6.628409759327085204, 120.2999964176511014, 0.9194780514890086298 ) ) ;
#31485 = CARTESIAN_POINT ( 'NONE',  ( 0.7724745873405186591, -15.29971413243098688, -0.5873327843062005060 ) ) ;
#31486 = CARTESIAN_POINT ( 'NONE',  ( 0.005915287708642085092, 116.9295063353193882, -0.2960251855814708399 ) ) ;
#31487 = CIRCLE ( 'NONE', #2955, 0.7619999999999983453 ) ;
#31488 = CARTESIAN_POINT ( 'NONE',  ( -0.6899137464274212039, -3.097154947502566813, -0.6881565663087282347 ) ) ;
#31489 = ORIENTED_EDGE ( 'NONE', *, *, #39691, .T. ) ;
#31490 = CARTESIAN_POINT ( 'NONE',  ( -55.81215269371604393, 4.390389611868092068, 0.4227292597524335283 ) ) ;
#31491 = CARTESIAN_POINT ( 'NONE',  ( -14.45325548908966695, 139.0941462050048187, 0.3122831254358890418 ) ) ;
#31492 = CARTESIAN_POINT ( 'NONE',  ( 5.397943591185104140, -12.01093657298729589, 0.9516947191793155847 ) ) ;
#31493 = CARTESIAN_POINT ( 'NONE',  ( 8.784047514290564962, 154.8283212766472445, -1.235621501372049513 ) ) ;
#31494 = ORIENTED_EDGE ( 'NONE', *, *, #20898, .F. ) ;
#31495 = CARTESIAN_POINT ( 'NONE',  ( 1.801784832236646094, 115.7029148924688116, 1.722822550453829482 ) ) ;
#31496 = CARTESIAN_POINT ( 'NONE',  ( -4.726758526000762295, 117.7280786527958156, -1.096802179199823035 ) ) ;
#31497 = CARTESIAN_POINT ( 'NONE',  ( 5.966562942537897207, 155.3820107761045790, 0.07923228615413213660 ) ) ;
#31498 = ORIENTED_EDGE ( 'NONE', *, *, #24127, .F. ) ;
#31499 = CARTESIAN_POINT ( 'NONE',  ( 11.23789960528888443, 121.3367100885591015, 1.694033198309416122 ) ) ;
#31500 = CARTESIAN_POINT ( 'NONE',  ( 3.174366308151881366, 84.67546620154573134, 0.06343139340882768262 ) ) ;
#31501 = DIRECTION ( 'NONE',  ( -1.000000000000000000, 0.000000000000000000, 0.000000000000000000 ) ) ;
#31502 = B_SPLINE_CURVE_WITH_KNOTS ( 'NONE', 3,
 ( #29161, #7, #34413, #8635 ),
 .UNSPECIFIED., .F., .F.,
 ( 4, 4 ),
 ( 0.000000000000000000, 1.000000000000000000 ),
 .UNSPECIFIED. ) ;
#31503 = DIRECTION ( 'NONE',  ( -0.8745520943968251304, 0.4849315768086532863, -5.424246918827961050E-16 ) ) ;
#31504 = CARTESIAN_POINT ( 'NONE',  ( 3.772649051594905156, 116.7207137014398626, -0.1335598970234344318 ) ) ;
#31505 = FACE_OUTER_BOUND ( 'NONE', #19274, .T. ) ;
#31506 = CIRCLE ( 'NONE', #36975, 5.080000000000006288 ) ;
#31507 = CARTESIAN_POINT ( 'NONE',  ( -11.37822013471369864, 56.06794068206548332, 5.016500000000540638 ) ) ;
#31508 = CARTESIAN_POINT ( 'NONE',  ( 1.969151417587075681, -15.07365727821173529, 5.800531510698589521 ) ) ;
#31509 = DIRECTION ( 'NONE',  ( -0.8745520943968225769, 0.4849315768086578382, -5.691349986800571545E-16 ) ) ;
#31510 = DIRECTION ( 'NONE',  ( -6.353134868986659519E-16, 1.000000000000000000, 0.000000000000000000 ) ) ;
#31511 = TOROIDAL_SURFACE ( 'NONE', #24034, 0.7620000000000000107, 0.2540000000000000036 ) ;
#31512 = CARTESIAN_POINT ( 'NONE',  ( -4.807805788012706749, 117.8776837157520561, 0.6743155973055370289 ) ) ;
#31513 = ORIENTED_EDGE ( 'NONE', *, *, #24554, .F. ) ;
#31514 = ORIENTED_EDGE ( 'NONE', *, *, #10507, .F. ) ;
#31515 = DIRECTION ( 'NONE',  ( -0.7548010569845121642, -0.6559537821943426383, 0.000000000000000000 ) ) ;
#31516 = CARTESIAN_POINT ( 'NONE',  ( -5.564994385194649062, 118.1214215447172080, -1.127427256207502948 ) ) ;
#31517 = B_SPLINE_CURVE_WITH_KNOTS ( 'NONE', 3,
 ( #16893, #16681, #39493, #20080, #13709, #36505, #23268, #32464, #6693, #36091 ),
 .UNSPECIFIED., .F., .F.,
 ( 4, 2, 2, 2, 4 ),
 ( -5.999999999944513512E-08, 0.0006000059959409705622, 0.001200071991881940551, 0.002400203983763880312, 0.004800467967527762003 ),
 .UNSPECIFIED. ) ;
#31518 = CARTESIAN_POINT ( 'NONE',  ( -4.275575466068185726, 118.7880935209305591, -0.6699701396488103589 ) ) ;
#31519 = CARTESIAN_POINT ( 'NONE',  ( 4.772772660974615277, 117.5405024988783396, 1.172286739505868702 ) ) ;
#31520 = CARTESIAN_POINT ( 'NONE',  ( -12.21488373878702127, 55.49440886859285627, -5.016499999999999737 ) ) ;
#31521 = CARTESIAN_POINT ( 'NONE',  ( -0.2185697341917780256, 107.6766875080336376, 4.612355970162428598 ) ) ;
#31522 = AXIS2_PLACEMENT_3D ( 'NONE', #29981, #20797, #27002 ) ;
#31523 = CARTESIAN_POINT ( 'NONE',  ( 2.522041008973656240, -3.380034811851383214, 3.874746376371965617 ) ) ;
#31524 = CARTESIAN_POINT ( 'NONE',  ( -5.639506490940112471, 64.42185452804264401, -1.269999999999993578 ) ) ;
#31525 = CARTESIAN_POINT ( 'NONE',  ( 15.36699999999999733, 12.96302561210691628, 1.881914736249736896E-15 ) ) ;
#31526 = CARTESIAN_POINT ( 'NONE',  ( 2.973740295910565212, -14.46567735677360744, 4.831635400698222504 ) ) ;
#31527 = CARTESIAN_POINT ( 'NONE',  ( 7.618479139564603209, 124.7215218652630710, 0.1522353441811858110 ) ) ;
#31528 = CARTESIAN_POINT ( 'NONE',  ( -8.045112435069388113, 121.5393406094847819, -1.176871282714906153 ) ) ;
#31529 = DIRECTION ( 'NONE',  ( -0.000000000000000000, -0.000000000000000000, -1.000000000000000000 ) ) ;
#31530 = DIRECTION ( 'NONE',  ( -0.1565721916417989190, -0.9876665170007961070, 6.504343050004413423E-15 ) ) ;
#31531 = CARTESIAN_POINT ( 'NONE',  ( -0.8204882251181495612, 115.7029491485453292, 1.724334212604217820 ) ) ;
#31532 = CARTESIAN_POINT ( 'NONE',  ( -2.923568588381722844, 13.88697512809157786, 3.594856661414283394 ) ) ;
#31534 = EDGE_LOOP ( 'NONE', ( #31918, #31494, #22117, #23043 ) ) ;
#31533 = CARTESIAN_POINT ( 'NONE',  ( 3.798364743159144741, 116.8316721669309572, 0.3950458664356922833 ) ) ;
#31535 = CARTESIAN_POINT ( 'NONE',  ( 4.653077788127276904, 104.6144662015412905, -2.613629344544315281 ) ) ;
#31536 = CARTESIAN_POINT ( 'NONE',  ( 3.946041497568072653, -15.66665589675640646, 3.498282510246776500 ) ) ;
#31537 = CARTESIAN_POINT ( 'NONE',  ( -12.16919611748930308, 122.5392882283422864, 1.309229788656695037 ) ) ;
#31538 = CARTESIAN_POINT ( 'NONE',  ( -0.9274737138984842089, 27.34353985424608524, 0.2860612317039745167 ) ) ;
#31539 = CARTESIAN_POINT ( 'NONE',  ( -0.8918910426314872186, 22.31184809748591391, -0.3959014520797728975 ) ) ;
#31540 = ORIENTED_EDGE ( 'NONE', *, *, #11028, .F. ) ;
#31541 = ORIENTED_EDGE ( 'NONE', *, *, #25110, .F. ) ;
#31542 = DIRECTION ( 'NONE',  ( 5.188838149069472160E-16, -1.699382548006136559E-16, -1.000000000000000000 ) ) ;
#31543 = CARTESIAN_POINT ( 'NONE',  ( 4.398525312957987765, 119.2572634999566930, 0.5937511404893220934 ) ) ;
#31544 = CARTESIAN_POINT ( 'NONE',  ( -16.07945855365744592, 143.8376908863262997, 0.9680047772055858646 ) ) ;
#31545 = CARTESIAN_POINT ( 'NONE',  ( 8.689997779576109740E-16, 9.026346327358515609, 0.000000000000000000 ) ) ;
#31546 = CARTESIAN_POINT ( 'NONE',  ( 2.454477138217164178, -14.79624793513299785, 5.258896552041426808 ) ) ;
#31547 = CARTESIAN_POINT ( 'NONE',  ( 7.451643811072074186, 155.9567503867590972, -1.565497431107723880 ) ) ;
#31548 = VECTOR ( 'NONE', #32481, 1000.000000000000000 ) ;
#31549 = CARTESIAN_POINT ( 'NONE',  ( -20.37866581877395689, 147.6366098820875266, -2.483541293540720396 ) ) ;
#31550 = DIRECTION ( 'NONE',  ( 9.627370216492862708E-17, 1.000000000000000000, -0.000000000000000000 ) ) ;
#31551 = EDGE_CURVE ( 'NONE', #12215, #21468, #925, .T. ) ;
#31552 = CARTESIAN_POINT ( 'NONE',  ( -14.16569067496518564, 138.8670163227233161, -0.2830642121559646673 ) ) ;
#31553 = CARTESIAN_POINT ( 'NONE',  ( -6.530520361951679398, 29.76765211936704247, -0.1582873856006195845 ) ) ;
#31554 = CARTESIAN_POINT ( 'NONE',  ( 15.41453346427784155, 143.5427300040290106, -0.2938895485367987725 ) ) ;
#31555 = AXIS2_PLACEMENT_3D ( 'NONE', #25648, #39494, #28848 ) ;
#31556 = ORIENTED_EDGE ( 'NONE', *, *, #6503, .T. ) ;
#31557 = DIRECTION ( 'NONE',  ( 5.188838149069472160E-16, -1.699382548006136559E-16, -1.000000000000000000 ) ) ;
#31558 = DIRECTION ( 'NONE',  ( -5.188838149069472160E-16, 1.699382548006136559E-16, 1.000000000000000000 ) ) ;
#31559 = DIRECTION ( 'NONE',  ( -0.000000000000000000, -0.000000000000000000, -1.000000000000000000 ) ) ;
#31560 = CIRCLE ( 'NONE', #16588, 0.2540000000000002811 ) ;
#31561 = CARTESIAN_POINT ( 'NONE',  ( -57.20860189792659156, 2.757428422320171268, 2.041684569450760822 ) ) ;
#31562 = EDGE_CURVE ( 'NONE', #10068, #38754, #19840, .T. ) ;
#31563 = CARTESIAN_POINT ( 'NONE',  ( 2.357476308904321360, 24.96372521773390929, -8.086248583043326832 ) ) ;
#31564 = CARTESIAN_POINT ( 'NONE',  ( 16.15947664645532100, 148.3349945484709451, 1.756847814979443756 ) ) ;
#31565 = CARTESIAN_POINT ( 'NONE',  ( -2.958531772299361151, 39.20946620154573736, -1.329372033065077119 ) ) ;
#31566 = CARTESIAN_POINT ( 'NONE',  ( 8.075779052176489614, 158.6620026115301698, 0.1430648235678990965 ) ) ;
#31567 = CARTESIAN_POINT ( 'NONE',  ( -7.669306984062492560, 124.7206709383052043, -0.1533317827557519053 ) ) ;
#31568 = AXIS2_PLACEMENT_3D ( 'NONE', #3295, #22845, #3724 ) ;
#31569 = AXIS2_PLACEMENT_3D ( 'NONE', #22512, #9141, #2959 ) ;
#31570 = CARTESIAN_POINT ( 'NONE',  ( -0.8823465807374654135, 5.041073445128725794, 4.537322665494407659 ) ) ;
#31571 = CARTESIAN_POINT ( 'NONE',  ( 5.945776936743700780, 121.5465042053001667, 0.1188107733588234238 ) ) ;
#31572 = PRODUCT_DEFINITION ( 'UNKNOWN', '', #8708, #22694 ) ;
#31573 = CARTESIAN_POINT ( 'NONE',  ( -0.3690887223898375868, -3.321408231106627973, -8.411989387140767604 ) ) ;
#31574 = CARTESIAN_POINT ( 'NONE',  ( -57.72731561024291125, 0.8685078910842247701, -0.07340608407947644964 ) ) ;
#31575 = CARTESIAN_POINT ( 'NONE',  ( 5.518167891550173287, 117.1006821660659227, -0.5215187594908856639 ) ) ;
#31576 = CARTESIAN_POINT ( 'NONE',  ( -0.8775954529457390407, 122.2453746293775652, -0.2818696459738748716 ) ) ;
#31577 = AXIS2_PLACEMENT_3D ( 'NONE', #22872, #25472, #6932 ) ;
#31578 = LINE ( 'NONE', #37543, #40972 ) ;
#31579 = CARTESIAN_POINT ( 'NONE',  ( -3.164706401634815869, 50.63946620154572997, -1.543954388298182101 ) ) ;
#31580 = CARTESIAN_POINT ( 'NONE',  ( -4.507778648822867495, 31.37953541088120346, -1.025544427737863362 ) ) ;
#31581 = CARTESIAN_POINT ( 'NONE',  ( 0.9908229604283667058, 117.3993836601774490, 1.479714518555806491 ) ) ;
#31582 = CARTESIAN_POINT ( 'NONE',  ( -15.74027684387364978, 85.27021604205610572, -1.270000000000002460 ) ) ;
#31583 = CARTESIAN_POINT ( 'NONE',  ( 6.059261036834406866, 57.14999999999999858, 5.016499999999999737 ) ) ;
#31584 = EDGE_CURVE ( 'NONE', #4990, #1598, #23883, .T. ) ;
#31585 = CARTESIAN_POINT ( 'NONE',  ( 0.8427018527670834258, 121.5536190086353372, -0.3367535922268982129 ) ) ;
#31586 = CARTESIAN_POINT ( 'NONE',  ( -1.399407963385900899, 159.5796833544862352, 0.3162364300534757922 ) ) ;
#31587 = EDGE_LOOP ( 'NONE', ( #38682, #37703, #27879, #4531 ) ) ;
#31588 = CARTESIAN_POINT ( 'NONE',  ( -58.49256177947683000, 0.7572623586737103896, -0.8868308481464118875 ) ) ;
#31589 = EDGE_CURVE ( 'NONE', #2780, #18488, #15844, .T. ) ;
#31590 = VERTEX_POINT ( 'NONE', #35847 ) ;
#31591 = CARTESIAN_POINT ( 'NONE',  ( -41.35912177800447154, 22.76994845978005344, -1.271081184882984383 ) ) ;
#31592 = CARTESIAN_POINT ( 'NONE',  ( -11.75644783568344209, 130.2587663741292658, -0.1212624266273917006 ) ) ;
#31593 = CARTESIAN_POINT ( 'NONE',  ( 2.058067359092986326, -15.63668844659656187, 5.842422791592841946 ) ) ;
#31594 = CARTESIAN_POINT ( 'NONE',  ( -5.883429839103577308, 118.5625182843610617, 0.8957466683066146462 ) ) ;
#31595 = EDGE_CURVE ( 'NONE', #39783, #19939, #6867, .T. ) ;
#31596 = CARTESIAN_POINT ( 'NONE',  ( 22.10195095183540204, 148.8299554149626260, -1.146864445019731171 ) ) ;
#31597 = CARTESIAN_POINT ( 'NONE',  ( 1.141857472271699425, 24.90688314728939190, 4.478778191171412182 ) ) ;
#31598 = CARTESIAN_POINT ( 'NONE',  ( -15.47334368943532290, 120.8153160915142337, -0.6283931236857891456 ) ) ;
#31599 = CARTESIAN_POINT ( 'NONE',  ( -58.51381316099766394, -0.04972149827416968287, -0.6596742545330949170 ) ) ;
#31600 = EDGE_LOOP ( 'NONE', ( #12465, #22042, #25127, #10961, #18958, #34034, #39309, #21678, #39455, #26837 ) ) ;
#31601 = CARTESIAN_POINT ( 'NONE',  ( 0.3702369378893882734, 122.2435587914033022, 0.3018087652966767731 ) ) ;
#31602 = DIRECTION ( 'NONE',  ( 5.188838149069472160E-16, -1.699382548006136559E-16, -1.000000000000000000 ) ) ;
#31603 = CARTESIAN_POINT ( 'NONE',  ( -1.430496892223491079, 119.9358631726476574, 0.4886406555826711684 ) ) ;
#31604 = CARTESIAN_POINT ( 'NONE',  ( -55.48157428470955921, 5.837899645253390446, -2.755819015989877663 ) ) ;
#31605 = CARTESIAN_POINT ( 'NONE',  ( 17.18700207657765944, 151.3967157021085654, -1.745027292404997432 ) ) ;
#31606 = CARTESIAN_POINT ( 'NONE',  ( -9.094277710717381780, 119.2843051134756536, -1.347562189204172034 ) ) ;
#31607 = CARTESIAN_POINT ( 'NONE',  ( -53.09398923718962493, 10.65108322687173548, -3.938325876039776574 ) ) ;
#31608 = CARTESIAN_POINT ( 'NONE',  ( 7.125763582822450815, 121.8059686962219672, -0.4001172506815711127 ) ) ;
#31609 = VERTEX_POINT ( 'NONE', #23024 ) ;
#31610 = CARTESIAN_POINT ( 'NONE',  ( -18.07470265256061381, 147.5382818419693649, -2.342107984669389520 ) ) ;
#31611 = CARTESIAN_POINT ( 'NONE',  ( 4.393930847168488363, -15.54918382657802312, 2.099248807845041309 ) ) ;
#31612 = CARTESIAN_POINT ( 'NONE',  ( -4.065972646788793554, 118.2429491485453070, -0.3080848862740693250 ) ) ;
#31613 = CARTESIAN_POINT ( 'NONE',  ( -58.43690671596436914, -0.4125963578781866037, -1.035377653829272970E-14 ) ) ;
#31614 = CARTESIAN_POINT ( 'NONE',  ( -4.897933694818515704, 117.4787572636957265, 0.9608329789684921796 ) ) ;
#31615 = CARTESIAN_POINT ( 'NONE',  ( 11.27861017918422526, 123.5700555580090594, 1.596916299002706818 ) ) ;
#31616 = CARTESIAN_POINT ( 'NONE',  ( -30.09725872720941453, 70.36776381375388212, -1.270000000000007123 ) ) ;
#31617 = CARTESIAN_POINT ( 'NONE',  ( -2.691543149356179665, 0.9405793051805824145, -7.980626778548312927 ) ) ;
#31618 = CARTESIAN_POINT ( 'NONE',  ( 10.44459398727714472, 153.0728660266736370, 0.5066767128784235297 ) ) ;
#31619 = LINE ( 'NONE', #12020, #22159 ) ;
#31620 = ADVANCED_FACE ( 'NONE', ( #20254 ), #6448, .T. ) ;
#31623 = EDGE_CURVE ( 'NONE', #20434, #3752, #9016, .T. ) ;
#31622 = VERTEX_POINT ( 'NONE', #32854 ) ;
#31621 = DIRECTION ( 'NONE',  ( 0.000000000000000000, -0.000000000000000000, -1.000000000000000000 ) ) ;
#31624 = CARTESIAN_POINT ( 'NONE',  ( -0.8481206146765604137, 117.9394518213541403, 1.367598340852225425 ) ) ;
#31625 = CARTESIAN_POINT ( 'NONE',  ( -57.36719850051837000, 1.975114663830185302, 1.756955940785651871 ) ) ;
#31626 = CARTESIAN_POINT ( 'NONE',  ( -7.976708347975113078, 121.5957277616080745, -1.139915918955932694 ) ) ;
#31627 = CARTESIAN_POINT ( 'NONE',  ( -58.37241122568488549, -0.2962816677227753104, -1.039428729632917149E-14 ) ) ;
#31628 = CARTESIAN_POINT ( 'NONE',  ( -52.06588384954375925, 19.72955628912294301, 0.3571238398875058451 ) ) ;
#31629 = CARTESIAN_POINT ( 'NONE',  ( -22.65077213736933004, 150.6401102206664291, -0.2239908233986876995 ) ) ;
#31630 = ORIENTED_EDGE ( 'NONE', *, *, #7183, .F. ) ;
#31631 = CARTESIAN_POINT ( 'NONE',  ( -49.01671973967525275, 18.67808020721671625, -5.174630477995055600 ) ) ;
#31632 = CARTESIAN_POINT ( 'NONE',  ( 7.810646221566016401, 122.5288342873456031, -0.1253198868880078809 ) ) ;
#31633 = CARTESIAN_POINT ( 'NONE',  ( -5.639506490940112471, 64.42185452804264401, -1.523999999999993582 ) ) ;
#31634 = VERTEX_POINT ( 'NONE', #39459 ) ;
#31635 = CARTESIAN_POINT ( 'NONE',  ( 0.8204245609312718068, 115.7029491485453718, -1.724338730900728534 ) ) ;
#31636 = CARTESIAN_POINT ( 'NONE',  ( -15.73024628025059712, 145.6958675726371553, -0.4429222902984590871 ) ) ;
#31637 = CARTESIAN_POINT ( 'NONE',  ( 4.992311776856191763, -13.37494578157311054, 3.269494339340476952 ) ) ;
#31638 = CARTESIAN_POINT ( 'NONE',  ( -15.35657197080329084, 154.8698957928756954, 1.403577372161787906 ) ) ;
#31639 = CARTESIAN_POINT ( 'NONE',  ( 5.555120986090499535, 78.91530963298721701, -5.093895734005235099 ) ) ;
#31640 = CARTESIAN_POINT ( 'NONE',  ( 23.29193865421784793, 149.0397177335360652, 0.7969840597304524987 ) ) ;
#31641 = EDGE_CURVE ( 'NONE', #37473, #40423, #13883, .T. ) ;
#31642 = CARTESIAN_POINT ( 'NONE',  ( 15.26080815366967869, 148.0236959631692173, 0.4380210713017328450 ) ) ;
#31643 = DIRECTION ( 'NONE',  ( -0.9336303900108928744, -0.3582377630123714241, 0.000000000000000000 ) ) ;
#31644 = CARTESIAN_POINT ( 'NONE',  ( -0.1409938471676187022, 25.13008524939761656, 0.9676832235670267401 ) ) ;
#31645 = CARTESIAN_POINT ( 'NONE',  ( -2.754305024641401367, 116.5489981622532127, -0.1298538421819643296 ) ) ;
#31646 = DIRECTION ( 'NONE',  ( -0.8745520943968246863, 0.4849315768086537859, -5.361993529360573944E-16 ) ) ;
#31647 = DIRECTION ( 'NONE',  ( 1.011795553208986377E-16, 1.000000000000000000, -0.000000000000000000 ) ) ;
#31648 = ORIENTED_EDGE ( 'NONE', *, *, #28983, .F. ) ;
#31649 =( GEOMETRIC_REPRESENTATION_CONTEXT ( 3 ) GLOBAL_UNCERTAINTY_ASSIGNED_CONTEXT ( ( #29104 ) ) GLOBAL_UNIT_ASSIGNED_CONTEXT ( ( #24013, #14423, #1465 ) ) REPRESENTATION_CONTEXT ( 'NONE', 'WORKASPACE' ) );
#31650 = CARTESIAN_POINT ( 'NONE',  ( 5.999509053885005549, 118.7663675842279787, 1.217167017065042822 ) ) ;
#31651 = CARTESIAN_POINT ( 'NONE',  ( 2.362155674307470310, -13.89060443905824194, -3.983575812745123290 ) ) ;
#31652 = CARTESIAN_POINT ( 'NONE',  ( 12.43770564682699842, 156.7420262770442037, 1.659670365993107355 ) ) ;
#31653 = CARTESIAN_POINT ( 'NONE',  ( 19.16692462419648280, 150.4642993720107143, -1.670612363451736027 ) ) ;
#31654 = CARTESIAN_POINT ( 'NONE',  ( 8.378134419073882455, 22.78949214230337006, 1.148743996083190888 ) ) ;
#31655 = EDGE_CURVE ( 'NONE', #28135, #1100, #7607, .T. ) ;
#31656 = CARTESIAN_POINT ( 'NONE',  ( 0.01887972822138463125, 159.3676309965788960, -0.9448188026860500077 ) ) ;
#31657 = CARTESIAN_POINT ( 'NONE',  ( 4.858182150843307845, 117.6759154865132899, -0.8826695618964555123 ) ) ;
#31658 = CARTESIAN_POINT ( 'NONE',  ( 7.669269000495035904, 124.9344662015457317, 0.1532502464757268257 ) ) ;
#31659 = CARTESIAN_POINT ( 'NONE',  ( -5.933842156842998428, 121.5392726388429168, -0.04747900449317086352 ) ) ;
#31660 = CARTESIAN_POINT ( 'NONE',  ( -19.21961548592749836, 147.3692480224366079, -2.508364867928685626 ) ) ;
#31661 = CARTESIAN_POINT ( 'NONE',  ( 2.825551972395176303, -15.60239892947398666, 5.624417742107700846 ) ) ;
#31662 = DIRECTION ( 'NONE',  ( -9.627370216492862708E-17, -1.000000000000000000, 0.000000000000000000 ) ) ;
#31663 = CARTESIAN_POINT ( 'NONE',  ( -4.379091697861483112, 117.3993836135479967, -1.268018312266817160 ) ) ;
#31664 = EDGE_LOOP ( 'NONE', ( #7230, #18972, #35372, #16268 ) ) ;
#31665 = B_SPLINE_SURFACE_WITH_KNOTS ( 'NONE', 3, 3, ( 
 ( #8900, #18679, #40865, #34471, #27444, #5304, #21442, #14435, #18253, #40460, #31258, #8268, #34269, #5097, #28064, #41074, #11883, #8691, #18049, #31051, #1890, #172, #9941, #2736, #13142, #38713, #41498, #6136, #19725, #31899, #12926, #9735, #12718, #28903, #38925, #16325, #22492, #16108, #41918, #19100, #9116, #15902, #9320, #32315, #26134, #2939, #35733 ),
 ( #6544, #25708, #22912, #12304, #32108, #9524, #29329, #35519, #22703, #19519, #6340, #5929, #32527, #29112, #19311, #18891, #25504, #41706, #39135, #3358, #3145, #42130, #22282, #35945, #6757, #2529, #15692, #15491, #28489, #12513, #38504, #25917, #25292, #28698, #38296, #22078, #35105, #35308, #3578, #385, #26557, #20353, #6975, #20151, #26772, #33174, #30172 ),
 ( #29551, #26341, #29959, #39991, #23122, #23977, #39347, #800, #10151, #36159, #23763, #1013, #19946, #36376, #36786, #7816, #7604, #36995, #13567, #20564, #16541, #13775, #32746, #33593, #30374, #4426, #32966, #4002, #39782, #13351, #36576, #10997, #17384, #7392, #10783, #39564, #1223, #3791, #16751, #10576, #14183, #29756, #595, #10368, #23555, #23339, #7193 ),
 ( #16960, #33377, #27186, #4210, #40200, #17173, #13977, #26981, #33802, #18001, #12041, #8216, #1841, #30589, #8434, #27598, #25031, #14593, #8016, #1428, #14387, #18206, #31426, #38034, #2050, #41024, #17585, #11833, #27394, #31207, #40405, #8641, #21603, #1639, #40608, #11199, #11407, #4630, #11616, #34631, #24394, #24185, #4838, #27807, #15015, #15231, #24820 ),
 ( #28231, #37195, #30999, #24602, #20987, #37399, #34008, #28015, #17792, #30789, #21190, #14805, #2268, #41237, #20778, #37815, #5458, #34217, #40815, #5046, #18418, #37608, #21392, #34419, #5252, #22443, #6090, #2897, #29067, #15647, #38462, #38876, #15859, #12676, #5884, #25665, #16277, #38253, #12881, #2481, #19053, #25249, #31851, #28865, #32274, #26083, #18846 ),
 ( #9688, #9070, #15442, #32058, #28446, #41451, #42087, #19267, #12256, #12472, #25870, #8854, #22655, #13091, #2690, #35688, #21818, #41877, #126, #9280, #38672, #18636, #9479, #28652, #34845, #41664, #22035, #31640, #35063, #6296, #19475, #5678, #3104, #6497, #25466, #32482, #22238, #16065, #35266, #3311, #29281, #35472, #19896, #32697, #29705, #9892, #29915 ),
 ( #3532, #23078, #3953, #7345, #33545, #17124, #33331, #33124, #4377, #6712, #7143, #754, #19681, #546, #16492, #4161, #39299, #26291, #29498, #20100, #7556, #17335, #20516, #13933, #26928, #6926, #16915, #22865, #39941, #10733, #338, #26723, #13304, #10529, #36326, #13729, #30125, #3742, #26509, #23715, #39731, #23499, #36112, #36526, #30326, #10107, #964 ),
 ( #1170, #36733, #32912, #39090, #14134, #16700, #13521, #23289, #35902, #39514, #10320, #20305, #10942, #31319, #40149, #36947, #21503, #15337, #1379, #15122, #21715, #28125, #25145, #21930, #2377, #5988, #18317, #8544, #27347, #40360, #5570, #34536, #24716, #37930, #11941, #34959, #41560, #18528, #41351, #24932, #2163, #33755, #41135, #5362, #28342, #25356, #8753 ),
 ( #17539, #31747, #34739, #35161, #23931, #31533, #12153, #12368, #38149, #5782, #18737, #8962, #30541, #2590, #15550, #28552, #14337, #38360, #37720, #9175, #22132, #18951, #31957, #2796, #27136, #7768, #20731, #11155, #4581, #36000, #12774, #25764, #15, #10208, #32166, #13411, #35363, #41771, #19367, #28758, #25559, #9582, #3415, #3001, #3202, #9790, #16164 ),
 ( #32582, #36213, #6397, #38771, #15961, #28959, #35791, #22551, #35581, #13202, #16597, #29169, #41975, #19574, #19783, #32373, #12981, #25974, #441, #22758, #38982, #32802, #23178, #6603, #16382, #29387, #227, #38563, #26186, #9376, #39190, #26400, #7034, #9998, #22970, #12572, #6813, #3633, #39405, #29606, #20001, #33019, #15753, #22340, #6193, #19162, #1066 ),
 ( #23612, #13831, #17231, #1488, #11259, #4060, #14445, #40047, #653, #7455, #21045, #33232, #14238, #11054, #30645, #30227, #24039, #37054, #20412, #7246, #40260, #17437, #33441, #20205, #26829, #858, #27455, #33858, #4268, #14034, #10633, #7872, #24245, #40468, #17019, #3848, #20834, #39836, #36633, #27038, #37253, #30018, #8071, #23395, #29814, #10840, #16812 ),
 ( #23825, #36845, #7664, #20622, #1280, #4687, #33652, #13621, #4477, #30434, #27244, #17643, #26612, #39619, #10425, #36427, #34902, #5313, #34278, #37878, #38095, #11675, #5107, #21451, #18687, #41084, #18059, #8910, #41509, #18264, #31267, #31062, #34688, #1698, #1900, #27657, #5517, #31697, #28500, #34481, #11892, #4897, #24881, #2109, #2539, #8701, #25302 ),
 ( #12314, #8278, #21664, #15073, #18475, #31480, #24662, #14863, #28073, #15500, #38305, #27866, #9126, #2325, #30853, #37671, #34070, #21248, #15285, #41297, #28290, #12101, #25090, #5734, #21876, #17852, #14653, #8494, #40668, #11460, #40874, #24450, #37454, #22501, #13150, #5941, #12522, #26143, #35531, #29559, #18900, #38724, #6351, #32325, #19321, #16334, #35953 ),
 ( #3154, #25717, #28707, #16118, #28912, #9744, #19733, #29121, #39145, #31910, #25513, #9949, #42140, #394, #2747, #9532, #12935, #6766, #25925, #29339, #22922, #38934, #38513, #181, #35741, #22713, #9330, #2948, #19111, #32754, #3588, #6553, #19528, #41927, #16549, #13361, #26350, #22293, #22087, #39356, #32118, #15912, #32535, #35114, #35318, #15702, #41716 ),
 ( #6145, #12728, #3367, #40002, #26565, #39791, #4221, #10585, #7614, #4435, #26991, #30600, #808, #33184, #10378, #23347, #30181, #16969, #7201, #20576, #11008, #23563, #36385, #13987, #14192, #29968, #20159, #36585, #37006, #17182, #4012, #27197, #17596, #7403, #20365, #13784, #10793, #19955, #26780, #3798, #23775, #7825, #4639, #33387, #1022, #23130, #36796 ),
 ( #33602, #1438, #17393, #23987, #14398, #39572, #30384, #1235, #40210, #20787, #33811, #27406, #10160, #36167, #6985, #32973, #16760, #29767, #603, #13577, #15454, #27610, #8653, #5469, #11626, #24404, #41035, #8027, #11418, #34023, #11844, #38045, #34856, #40827, #18216, #11212, #31217, #24613, #25042, #2061, #31652, #5263, #12052, #5688, #14605, #15025, #37621 ),
 ( #31010, #24196, #28025, #8865, #1852, #4848, #37410, #24831, #21614, #18645, #18428, #34641, #34430, #2492, #20998, #8444, #37826, #17804, #14816, #30801, #31436, #40619, #8229, #1650, #21402, #21827, #40416, #37206, #15242, #28243, #21202, #2278, #34228, #41247, #5057, #18013, #27818, #2701, #42098, #25677, #22455, #6510, #35277, #15870, #16289, #35484, #32286 ),
 ( #35914, #15658, #32494, #22045, #38684, #28662, #9290, #6306, #9700, #3543, #38472, #6724, #13103, #29293, #41674, #35074, #9490, #136, #26095, #39101, #12482, #28876, #19278, #9080, #3115, #19692, #3322, #16075, #19485, #22251, #9904, #25258, #5895, #29079, #35699, #18856, #32709, #31861, #12893, #25476, #6102, #22876, #38888, #19065, #32071, #28456, #41462 ),
 ( #2907, #12269, #38263, #25881, #41889, #12687, #22666, #4172, #20526, #10745, #19909, #16504, #30136, #29716, #558, #33135, #33556, #32924, #23726, #36124, #350, #23301, #29511, #10119, #10331, #36537, #3755, #3965, #13740, #16926, #17134, #975, #23510, #17346, #36338, #39527, #13533, #26521, #39742, #7154, #20113, #13942, #36745, #29926, #764, #7356, #26940 ),
 ( #26734, #7566, #10541, #20315, #39951, #13317, #33342, #4388, #26303, #39312, #16713, #23090, #6938, #13014, #10034, #6849, #12807, #32411, #25397, #3241, #25798, #39224, #16200, #3664, #19403, #26219, #19818, #28797, #29204, #9616, #48, #39017, #32205, #22374, #38804, #23006, #32835, #12606, #36034, #6430, #9210, #15995, #29636, #41811, #22791, #19607, #22584 ),
 ( #16630, #26008, #9825, #35616, #28995, #18987, #35827, #19198, #6643, #12405, #32620, #3452, #38399, #2829, #16415, #29421, #22167, #35199, #42012, #262, #6025, #13236, #31991, #15789, #25594, #38601, #9408, #35400, #6227, #3038, #23427, #39653, #40293, #30467, #891, #20659, #39439, #36246, #39866, #7698, #33049, #33891, #7067, #10663, #20031, #3880, #33685 ),
 ( #4508, #17674, #17470, #4721, #36455, #1312, #13447, #23644, #474, #30053, #36666, #10242, #30258, #7275, #26435, #20237, #29845, #23213, #16845, #40078, #11086, #683, #23861, #14268, #13655, #27279, #26645, #10873, #10457, #24073, #37085, #33263, #4092, #17051, #13865, #26859, #33474, #7902, #7487, #20447, #4304, #17267, #36880, #20867, #1098, #14066, #27070 ),
 ( #4710, #27678, #8301, #30457, #4919, #24266, #27266, #34090, #27478, #21271, #18285, #21065, #11698, #4498, #11076, #24685, #17873, #28094, #17459, #37272, #30875, #5331, #1719, #27886, #37692, #8092, #24059, #14884, #34299, #14674, #37074, #1512, #17664, #31288, #8514, #40690, #11482, #40487, #40894, #41105, #2130, #20854, #20645, #21473, #30664, #14468, #24472 ),
 ( #15093, #40284, #1301, #37474, #33675, #14258, #11281, #5130, #7893, #18081, #31083, #1922, #34504, #11912, #24900, #37899, #33882, #6363, #9145, #41943, #34707, #41317, #12744, #22103, #16130, #5537, #25322, #35131, #35547, #5958, #15928, #25731, #12334, #12122, #2965, #22308, #38327, #25112, #31716, #5753, #19333, #38738, #18917, #31927, #15519, #28926, #29133 ),
 ( #8722, #9546, #18706, #2558, #2764, #3168, #38116, #32339, #28310, #18495, #15719, #21683, #31499, #28521, #38530, #8929, #28724, #41735, #12540, #6160, #22516, #25529, #42152, #41529, #9345, #21897, #34926, #35332, #19127, #32133, #12947, #25937, #2347, #15305, #620, #821, #16564, #9965, #26365, #23577, #3814, #22937, #13797, #4234, #23144, #10175, #35965 ),
 ( #6779, #32546, #39586, #36600, #33404, #39373, #16777, #9760, #29781, #36181, #7420, #13589, #30194, #26578, #10598, #17195, #13167, #10391, #7001, #23363, #36397, #29573, #19748, #19970, #20378, #1035, #39159, #14000, #32987, #35755, #409, #38947, #26157, #7214, #4025, #20173, #33199, #32768, #16983, #29983, #6570, #26795, #13377, #3381, #16348, #39805, #22725 ),
 ( #19540, #3600, #29353, #193, #14412, #21012, #27419, #24417, #21215, #1664, #5280, #17610, #7836, #27211, #40226, #4863, #33824, #24001, #37422, #27834, #40432, #11020, #30818, #31027, #4653, #37021, #11224, #11644, #34035, #20800, #1867, #34447, #24209, #37220, #30611, #27623, #36811, #1453, #20587, #40633, #24628, #21420, #8039, #17818, #40016, #14620, #11429 ),
 ( #18231, #8243, #40841, #31233, #1249, #34242, #5074, #18025, #14829, #37638, #8462, #2075, #27004, #10808, #23790, #7629, #33616, #4447, #17405, #30399, #14205, #25489, #22266, #25272, #41477, #41262, #22061, #2717, #24848, #12284, #18660, #21630, #28471, #21841, #15673, #12702, #15468, #6117, #41050, #5483, #19083, #38276, #22471, #11861, #31666, #9095, #41902 ),
 ( #32086, #2507, #18443, #9305, #28677, #35087, #31449, #38061, #12069, #25691, #2921, #5910, #18871, #34869, #35290, #35501, #38696, #15254, #15041, #15884, #25056, #8878, #31876, #9505, #2293, #5702, #41687, #37845, #28257, #8668, #12495, #6320, #19293, #38486, #28889, #28041, #32298, #34656, #29941, #6956, #36555, #10132, #16942, #39762, #19500, #19925, #366 ),
 ( #22893, #13121, #16519, #780, #10557, #3340, #13756, #39326, #42112, #6739, #20332, #32510, #13548, #10349, #13332, #29527, #29311, #23105, #32942, #12907, #26321, #19710, #9716, #36139, #9923, #3771, #26752, #3560, #36356, #29094, #35716, #7171, #16731, #23528, #25898, #32728, #29735, #7373, #574, #23319, #20130, #26539, #6524, #39545, #33155, #3983, #16308 ),
 ( #3128, #16089, #38904, #22682, #35929, #153, #26113, #39117, #33572, #33358, #11383, #30351, #1200, #17564, #27780, #7582, #30977, #10761, #17152, #36973, #4190, #994, #27163, #20964, #20542, #20756, #27374, #33781, #30765, #27577, #7996, #11592, #23955, #14160, #4406, #17363, #11178, #40176, #10971, #1615, #34195, #4609, #7795, #37172, #37376, #30565, #1405 ),
 ( #14361, #8193, #40792, #40383, #24163, #30152, #33985, #4813, #17980, #17766, #40585, #24370, #14572, #36763, #21162, #5019, #1817, #14781, #24575, #37581, #8408, #13958, #26957, #39971, #23742, #28625, #28839, #19027, #21579, #21368, #41639, #18391, #31402, #5654, #15833, #37790, #32033, #41000, #5228, #25009, #34395, #31184, #15202, #9042, #8617, #8831, #15415 ),
 ( #15621, #38228, #41852, #12014, #2244, #34606, #5435, #41425, #28205, #41213, #18817, #22210, #34819, #38009, #25222, #25438, #21791, #18609, #31615, #6066, #28419, #2454, #38439, #12651, #12232, #22008, #35039, #5859, #2026, #31825, #14991, #2662, #2871, #25638, #12446, #9254, #18183, #35240, #38646, #27992, #11804, #24795, #16461, #23260, #3926, #25841, #13278 ),
 ( #36083, #29251, #19448, #22836, #7114, #16886, #9660, #20073, #3502, #6270, #13062, #26694, #38849, #19867, #16673, #19652, #35874, #35662, #29468, #39272, #19241, #6685, #26052, #16039, #32668, #16247, #10078, #33095, #9866, #521, #35445, #42060, #13494, #308, #29887, #32455, #26262, #32882, #9452, #3286, #725, #36295, #39484, #22627, #3080, #23049, #10290 ),
 ( #6473, #6897, #3714, #32250, #29678, #13700, #26480, #22419, #29041, #95, #12854, #39063, #33304, #36919, #4764, #30096, #30932, #4134, #7737, #17093, #937, #30715, #7944, #13907, #1142, #1567, #14731, #14523, #1771, #20487, #27533, #10501, #20703, #39701, #27107, #33729, #7317, #27320, #4348, #23471, #33514, #26899, #20277, #39911, #37122, #8145, #36497 ),
 ( #10705, #17716, #23684, #20913, #36705, #40540, #11335, #17310, #30299, #7526, #14108, #40119, #30509, #24323, #10913, #23902, #4552, #17512, #33936, #34142, #37329, #21116, #1350, #4969, #14307, #40333, #11127, #17927, #24114, #8570, #21960, #27943, #14941, #37530, #8786, #38391, #35191, #9202, #2617, #15577, #37746, #21744, #11541, #28582, #41590, #31140, #15365 ),
 ( #18767, #31351, #1979, #34990, #41378, #2194, #40951, #21531, #24744, #25388, #12398, #28156, #41162, #34563, #5811, #11756, #27733, #31776, #5390, #18345, #11968, #22161, #15152, #6017, #5183, #24525, #24960, #40744, #8355, #37961, #28371, #34770, #5603, #18558, #31564, #25177, #18981, #2405, #31985, #12184, #38178, #8992, #2823, #21323, #34351, #18135, #13803 ),
 ( #15986, #20180, #20383, #35607, #28987, #3820, #1040, #23369, #42003, #33409, #23795, #625, #29786, #12800, #16988, #25587, #25791, #9402, #29989, #14005, #10814, #16783, #36402, #28790, #7219, #13595, #27011, #33204, #7635, #4030, #30200, #36816, #32197, #828, #26583, #26801, #39810, #6423, #38796, #39594, #40020, #20594, #9608, #33623, #10397, #12600, #19396 ),
 ( #10603, #23583, #36606, #7425, #22576, #4241, #17202, #38594, #15782, #32992, #22366, #41802, #35391, #6220, #19190, #3031, #37644, #30406, #37028, #8470, #4868, #11866, #1255, #21017, #17826, #31238, #30824, #11649, #21425, #8044, #7842, #40847, #18030, #34040, #20805, #27425, #1459, #2081, #34453, #1670, #14625, #11230, #24634, #24855, #15045, #27629, #40640 ),
 ( #24215, #34250, #28047, #11434, #5286, #14210, #33831, #18236, #24422, #37852, #27217, #37427, #8248, #41056, #21220, #8674, #21635, #5080, #4659, #4452, #31032, #1873, #17615, #40438, #14418, #17410, #40231, #14835, #27839, #37225, #11026, #24007, #30616, #34875, #34661, #12707, #31671, #2512, #18877, #29100, #8883, #32303, #12075, #18449, #38282, #5489, #2299 ),
 ( #21847, #22066, #28683, #35092, #32092, #28893, #9310, #12912, #25277, #15476, #5708, #18665, #12502, #41482, #28478, #2927, #35507, #5915, #12290, #38491, #38703, #9100, #31886, #2722, #19297, #41692, #15679, #9510, #42119, #25494, #22272, #35296, #6124, #15259, #19089, #28262, #15889, #3133, #25904, #41907, #25697, #31455, #22479, #6326, #16094, #38910, #9722 ),
 ( #41270, #25062, #38066, #10353, #7176, #371, #32734, #36146, #20337, #30157, #22897, #33362, #16736, #19505, #26326, #39975, #9928, #33159, #29945, #32949, #6961, #6746, #29740, #23325, #32516, #39767, #10561, #3565, #3778, #6529, #23534, #36561, #26119, #36360, #39122, #20136, #19932, #581, #785, #29535, #10139, #7377, #13553, #26543, #19714, #39550, #998 ),
 ( #16313, #3987, #35934, #16526, #16947, #13760, #22687, #13337, #13962, #4195, #17157, #39332, #29317, #26757, #26962, #35721, #3347, #23110, #159, #13129, #33576, #14576, #31187, #14784, #27581, #30980, #4613, #1820, #7586, #4410, #8000, #17983, #1204, #2032, #17367, #20969, #30356, #14164, #27786, #21168, #27171, #14367, #40796, #27995, #11596, #14995, #33785 ),
 ( #33991, #10768, #40387, #4819, #20547, #40589, #17568, #23748, #30571, #40182, #10976, #23960, #8197, #21372, #36767, #34200, #24579, #36978, #37585, #7799, #5025, #20761, #8413, #34398, #1411, #27377, #11182, #24167, #37177, #1620, #5231, #17773, #30771, #11389, #24374, #18186, #37382, #19031, #35244, #35042, #6273, #8620, #9046, #5657, #9455, #31829, #21796 ),
 ( #28209, #21582, #22012, #22422, #19244, #35450, #2457, #5439, #12235, #18613, #28629, #38649, #41428, #32037, #24800, #31406, #2874, #25226, #32254, #37794, #15420, #38231, #25642, #5862, #6069, #15836, #28423, #2247, #28843, #12449, #18822, #15206, #34824, #38012, #3083, #41856, #2666, #15625, #31618, #12653, #16043, #41003, #41217, #11809, #34610, #8834, #41642 ),
 ( #18397, #25443, #12019, #25012, #38442, #9257, #22214, #39275, #9664, #32885, #7321, #33099, #3718, #7119, #22839, #20076, #25844, #22630, #26265, #36298, #19451, #20280, #35666, #10081, #6476, #32460, #3929, #39488, #3289, #32671, #16889, #4137, #29890, #33307, #9869, #728, #42063, #23053, #29045, #16464, #36087, #38853, #16677, #35878, #12857, #6689, #16250 ),
 ( #26483, #39704, #29254, #10295, #13705, #99, #26698, #13065, #23263, #26056, #10505, #23475, #19656, #3506, #39067, #29471, #313, #19870, #36500, #13281, #6901, #29681, #524, #13497, #11545, #37333, #11341, #11131, #24529, #26902, #27326, #23908, #27738, #7948, #40124, #24327, #37536, #17516, #37127, #30100, #20917, #30515, #1775, #33940, #8360, #24118, #30936 ),
 ( #4768, #14313, #17720, #1571, #36923, #27112, #1354, #14736, #21328, #17313, #40748, #30721, #13910, #20708, #34355, #4352, #27537, #8149, #40337, #14528, #1145, #40544, #21120, #39915, #34148, #33733, #23689, #4974, #7741, #17933, #17097, #940, #10709, #36708, #7530, #20491, #33517, #30303, #14113, #4556, #10918, #31990, #18564, #12404, #38398, #8790, #8574 ),
 ( #21748, #21537, #28162, #2199, #2828, #35197, #5608, #31571, #11972, #25396, #12605, #15788, #5394, #5187, #9208, #15157, #41166, #2410, #41810, #34567, #28796, #24750, #31144, #34775, #18140, #14945, #24965, #34996, #18350, #15371, #41384, #28377, #2623, #41595, #21966, #25592, #37965, #12189, #31355, #25182, #38183, #9000, #5816, #15582, #6023, #18772, #31783 ) ),
 .UNSPECIFIED., .F., .F., .F.,
 ( 4, 1, 1, 1, 1, 1, 1, 1, 1, 1, 1, 1, 1, 1, 1, 1, 1, 1, 1, 1, 1, 1, 1, 1, 1, 1, 1, 1, 1, 1, 1, 1, 1, 1, 1, 1, 1, 1, 1, 1, 1, 1, 1, 1, 1, 1, 4 ),
 ( 4, 1, 1, 1, 1, 1, 1, 1, 1, 1, 1, 1, 2, 1, 1, 1, 2, 1, 1, 1, 1, 1, 2, 1, 1, 1, 1, 1, 1, 1, 2, 1, 1, 1, 1, 1, 1, 1, 1, 1, 4 ),
 ( 0.000000000000000000, 0.007812500000000000000, 0.01562500000000000000, 0.02343750000000000000, 0.03125000000000000000, 0.04687500000000000000, 0.06250000000000000000, 0.07812500000000000000, 0.09375000000000000000, 0.1093750000000000000, 0.1250000000000000000, 0.1406250000000000000, 0.1562500000000000000, 0.1875000000000000000, 0.2187500000000000000, 0.2500000000000000000, 0.2812500000000000000, 0.3125000000000000000, 0.3281250000000000000, 0.3437500000000000000, 0.3750000000000000000, 0.4062500000000000000, 0.4375000000000000000, 0.4687500000000000000, 0.5000000000000000000, 0.5312500000000000000, 0.5625000000000000000, 0.5937500000000000000, 0.6250000000000000000, 0.6562500000000000000, 0.6718750000000000000, 0.6875000000000000000, 0.7187500000000000000, 0.7500000000000000000, 0.7812500000000000000, 0.8125000000000000000, 0.8437500000000000000, 0.8750000000000000000, 0.8906250000000000000, 0.9062500000000000000, 0.9218750000000000000, 0.9375000000000000000, 0.9531250000000000000, 0.9687500000000000000, 0.9765625000000000000, 0.9843750000000000000, 1.000000000000000000 ),
 ( 0.000000000000000000, 0.01539374999999999945, 0.03078749999999999890, 0.04618125000000002089, 0.06157499999999999779, 0.07696875000000003020, 0.09236250000000004179, 0.1077562499999999979, 0.1231499999999999956, 0.1431375000000000008, 0.1631250000000000200, 0.1831125000000000114, 0.2031000000000000028, 0.2063375000000000070, 0.2095750000000000113, 0.2128125000000000155, 0.2160500000000000198, 0.2667375000000000163, 0.3174250000000000682, 0.3681125000000000647, 0.4188000000000000611, 0.5201750000000000540, 0.6215500000000000469, 0.6266374999999999584, 0.6317250000000000920, 0.6368124999999997815, 0.6418999999999999151, 0.6469874999999999376, 0.6520749999999999602, 0.6571624999999999828, 0.6622500000000000053, 0.7044687500000000879, 0.7466875000000001705, 0.7889062500000000311, 0.8010555555555555207, 0.8311249999999998916, 0.8733437499999998632, 0.9155625000000000568, 0.9403166666666666895, 0.9577812500000000284, 1.000000000000000000 ),
 .UNSPECIFIED. ) ;
#31666 = CARTESIAN_POINT ( 'NONE',  ( 2.275810046414661336, 157.5529522918930638, 1.704261365023472363 ) ) ;
#31667 = SURFACE_SIDE_STYLE ('',( #5703 ) ) ;
#31668 = DIRECTION ( 'NONE',  ( 9.627370216492862708E-17, 1.000000000000000000, -0.000000000000000000 ) ) ;
#31669 = CARTESIAN_POINT ( 'NONE',  ( -2.271240278323964468, 124.1308405194309188, 0.008591128553798703035 ) ) ;
#31670 = CARTESIAN_POINT ( 'NONE',  ( 3.135079784281773918, -3.970030566872769562, -7.817010796087090263 ) ) ;
#31671 = CARTESIAN_POINT ( 'NONE',  ( 13.94748453383783193, 150.2679186505038160, 1.219128122479325560 ) ) ;
#31672 = CARTESIAN_POINT ( 'NONE',  ( -4.732562794078051915, 118.5930653697794384, -1.019569371435221417 ) ) ;
#31673 = CIRCLE ( 'NONE', #6506, 0.5079999999999993410 ) ;
#31674 = CARTESIAN_POINT ( 'NONE',  ( 18.06489503062820390, 125.1493905788104684, -0.4137567899827961915 ) ) ;
#31675 = CARTESIAN_POINT ( 'NONE',  ( 5.449044798931634404, 57.15000000000252811, -5.145813327217715560 ) ) ;
#31676 = CARTESIAN_POINT ( 'NONE',  ( -58.15532689777176500, 0.1682042465437465772, 0.6324092216884573681 ) ) ;
#31677 = CARTESIAN_POINT ( 'NONE',  ( 7.126949251439474331, 78.78385021288468693, 2.234499184491886670 ) ) ;
#31678 = CARTESIAN_POINT ( 'NONE',  ( -4.074955089416341991, 118.2429491485453497, 0.1454234154749720065 ) ) ;
#31679 = CARTESIAN_POINT ( 'NONE',  ( -13.70496720262328161, 119.6480011847128253, -0.2738578607176473945 ) ) ;
#31680 = ORIENTED_EDGE ( 'NONE', *, *, #36346, .T. ) ;
#31681 = CARTESIAN_POINT ( 'NONE',  ( -57.24023649071029496, 3.661034843983918208, 2.195083147259549339 ) ) ;
#31682 = CARTESIAN_POINT ( 'NONE',  ( -4.428416584346161144, 119.5534643524533465, -0.9253073463357188722 ) ) ;
#31683 = CARTESIAN_POINT ( 'NONE',  ( -5.329450492226126990, 104.6144662015457243, -0.2809636609891541514 ) ) ;
#31684 = CARTESIAN_POINT ( 'NONE',  ( -3.075464349291260557, 156.1450793681712241, -0.7387695966741766318 ) ) ;
#31685 = CARTESIAN_POINT ( 'NONE',  ( 3.174366308151882254, 63.84746620154572838, 0.06343139340882768262 ) ) ;
#31686 = CARTESIAN_POINT ( 'NONE',  ( 0.1312748386005784529, 117.9496053154094994, -1.403673244313596857 ) ) ;
#31687 = EDGE_CURVE ( 'NONE', #35981, #22227, #18555, .T. ) ;
#31688 = VERTEX_POINT ( 'NONE', #19624 ) ;
#31689 = CARTESIAN_POINT ( 'NONE',  ( -4.563195415240126174, 21.88328375387019165, -0.7336086519975816289 ) ) ;
#31690 = CARTESIAN_POINT ( 'NONE',  ( -29.47815206463771887, 60.51098513943350810, 1.523999999999992916 ) ) ;
#31691 = CARTESIAN_POINT ( 'NONE',  ( -6.194847070882102180, 64.72978607931611350, -1.269999999999994023 ) ) ;
#31692 = CARTESIAN_POINT ( 'NONE',  ( -41.35912177800472023, 22.76994845977980120, 1.271081184897154825 ) ) ;
#31693 = CARTESIAN_POINT ( 'NONE',  ( -4.543829802832370035, 27.87764462337559834, 0.5128545597630081998 ) ) ;
#31694 = CARTESIAN_POINT ( 'NONE',  ( 6.992351373757773381, 121.9428086355924847, 0.2543945838518893998 ) ) ;
#31695 = ADVANCED_FACE ( 'NONE', ( #32639 ), #10891, .T. ) ;
#31696 = CARTESIAN_POINT ( 'NONE',  ( -3.199182136055901626, 19.34408232073488065, 3.339653329369344004 ) ) ;
#31697 = CARTESIAN_POINT ( 'NONE',  ( 18.14731753714279705, 154.1160801429439857, 1.378418044792611541 ) ) ;
#31698 = CARTESIAN_POINT ( 'NONE',  ( 1.155656144204274094, 104.6144662015457243, -4.695275792171453411 ) ) ;
#31700 = CARTESIAN_POINT ( 'NONE',  ( 17.06313393459302574, 153.7580772870718988, -1.402989014430432446 ) ) ;
#31699 = CARTESIAN_POINT ( 'NONE',  ( 2.565602711990033313, 107.6377026157736765, 4.562358351827791481 ) ) ;
#31701 = CARTESIAN_POINT ( 'NONE',  ( -10.90225753734639547, 122.6724665872831679, 1.173089625842028472 ) ) ;
#31702 = CARTESIAN_POINT ( 'NONE',  ( 0.7725557299734273631, -15.30006921971679112, -0.5871674697799584841 ) ) ;
#31703 = CARTESIAN_POINT ( 'NONE',  ( -21.97734904378691567, 136.8935083344700558, -1.380722529463845438 ) ) ;
#31704 = CARTESIAN_POINT ( 'NONE',  ( 0.6674325042100914818, 1.652014723813869823, 0.7093539244141242595 ) ) ;
#31705 = VERTEX_POINT ( 'NONE', #39885 ) ;
#31706 = CARTESIAN_POINT ( 'NONE',  ( -54.16862281694330505, 7.200593192618495841, 0.5614961770967360488 ) ) ;
#31707 = AXIS2_PLACEMENT_3D ( 'NONE', #18833, #12243, #2254 ) ;
#31708 = CARTESIAN_POINT ( 'NONE',  ( -15.99593626731850371, 146.6619865182943272, 0.4079709740032108067 ) ) ;
#31709 = CARTESIAN_POINT ( 'NONE',  ( 2.999908722124702720, -15.10219813539979938, 5.696538855611934515 ) ) ;
#31710 = CARTESIAN_POINT ( 'NONE',  ( 16.95093959817310036, 147.3835828867039766, -1.246432153888628713 ) ) ;
#31711 = ORIENTED_EDGE ( 'NONE', *, *, #19630, .F. ) ;
#31712 = CARTESIAN_POINT ( 'NONE',  ( 0.9705268335128862667, 115.7029418470908979, 1.748962964377746898 ) ) ;
#31713 = CARTESIAN_POINT ( 'NONE',  ( -4.666417123046072035, 117.8349074441706534, -1.040161417730997462 ) ) ;
#31714 = CARTESIAN_POINT ( 'NONE',  ( 4.599243292695290641, 121.2024757821991159, 0.09190382657876458583 ) ) ;
#31715 = ORIENTED_EDGE ( 'NONE', *, *, #20329, .T. ) ;
#31716 = CARTESIAN_POINT ( 'NONE',  ( 14.08011273344093972, 154.3735777161816429, 2.279704494881448884 ) ) ;
#31717 = LINE ( 'NONE', #21474, #36752 ) ;
#31718 = CARTESIAN_POINT ( 'NONE',  ( -6.422645615570758970, 77.88548590848095898, 1.270000000000002682 ) ) ;
#31719 = CARTESIAN_POINT ( 'NONE',  ( 4.837884815698807017, 117.5445328966380174, -0.9682318550270561097 ) ) ;
#31720 = CARTESIAN_POINT ( 'NONE',  ( 23.26894437362528834, 149.0206351951634076, 0.01026395906018904604 ) ) ;
#31721 = CARTESIAN_POINT ( 'NONE',  ( -4.825844303143389524, 56.51499999999997215, -4.829557277217701561 ) ) ;
#31722 = CARTESIAN_POINT ( 'NONE',  ( -11.08653569745463052, 56.26057688450561045, 4.438844214435411217 ) ) ;
#31723 = CARTESIAN_POINT ( 'NONE',  ( -47.15184857521119710, 25.06101562935922900, 0.8929867115423234525 ) ) ;
#31724 = CARTESIAN_POINT ( 'NONE',  ( 2.101534993908720228, -15.10541647001627297, 5.790699435179030630 ) ) ;
#31725 = CARTESIAN_POINT ( 'NONE',  ( -45.45367893016184979, 22.54667639846615046, 3.012003376585078662 ) ) ;
#31726 = CARTESIAN_POINT ( 'NONE',  ( -15.15189561879767410, 77.97492127061565270, 1.904999999999999583 ) ) ;
#31727 = CIRCLE ( 'NONE', #13368, 0.5079999999999997851 ) ;
#31728 = CARTESIAN_POINT ( 'NONE',  ( -4.619290091002365095, 118.0409613858636817, 0.6362367808012175940 ) ) ;
#31729 = CIRCLE ( 'NONE', #22854, 0.3810000000000007825 ) ;
#31730 = ORIENTED_EDGE ( 'NONE', *, *, #5071, .T. ) ;
#31731 = CARTESIAN_POINT ( 'NONE',  ( -18.00660244842765323, 5.291346980525729287E-15, 0.000000000000000000 ) ) ;
#31732 = CARTESIAN_POINT ( 'NONE',  ( -8.348687675306351252, 119.7531329056243123, -1.433503554597048257 ) ) ;
#31733 = CARTESIAN_POINT ( 'NONE',  ( -2.249496549248517496, 107.4436264546101967, -4.650814322000806911 ) ) ;
#31734 = CARTESIAN_POINT ( 'NONE',  ( 4.811414313804822207, 117.8278363537766182, 0.8915698343676533577 ) ) ;
#31735 = CARTESIAN_POINT ( 'NONE',  ( 2.102813808753936087, -15.18136450426021256, 5.202461169095355942 ) ) ;
#31736 = CARTESIAN_POINT ( 'NONE',  ( -0.3827772581122253492, 119.9741034315941732, 0.6590906510345962976 ) ) ;
#31737 = CARTESIAN_POINT ( 'NONE',  ( -2.646443841375008432, -8.127818987380491578, -3.789199236247322133 ) ) ;
#31738 = DIRECTION ( 'NONE',  ( -0.01997839162482761832, -1.040247600000950455E-18, 0.9998004120163610509 ) ) ;
#31739 = CARTESIAN_POINT ( 'NONE',  ( -6.059261036834476144, 57.14999999999999858, -5.016499999999999737 ) ) ;
#31740 = CARTESIAN_POINT ( 'NONE',  ( 1.676539183893630991, 107.1743931308027129, -4.723177562573835253 ) ) ;
#31741 = CARTESIAN_POINT ( 'NONE',  ( -9.008986559116538118, 121.9018297702777858, -1.332107995734232109 ) ) ;
#31742 = ADVANCED_FACE ( 'NONE', ( #23663 ), #7694, .T. ) ;
#31743 = CARTESIAN_POINT ( 'NONE',  ( -4.880629475884273205, 56.51998046905272588, 4.886937129211982977 ) ) ;
#31744 = CARTESIAN_POINT ( 'NONE',  ( -6.343766875392317317, 29.24386013958156738, 0.9673776462358610884 ) ) ;
#31745 = CARTESIAN_POINT ( 'NONE',  ( -3.248591992300019715, 115.7029686349078759, 1.528045359830205729 ) ) ;
#31746 = CARTESIAN_POINT ( 'NONE',  ( -1.544744425833544099, 4.816215111148435923, 4.377641278133862279 ) ) ;
#31748 = VERTEX_POINT ( 'NONE', #33493 ) ;
#31747 = CARTESIAN_POINT ( 'NONE',  ( 0.3196863354298822846, 116.7093555017326452, 0.2333483032394377543 ) ) ;
#31749 = CARTESIAN_POINT ( 'NONE',  ( 2.261452999203317216, 104.6144662015480549, -4.834054640181143725 ) ) ;
#31750 = CARTESIAN_POINT ( 'NONE',  ( 4.504576368470070591, -15.30243295294880745, -0.5136648547128764841 ) ) ;
#31751 = CARTESIAN_POINT ( 'NONE',  ( -16.46135582144571430, 131.4813445454897192, 1.641276044305395088 ) ) ;
#31752 = CARTESIAN_POINT ( 'NONE',  ( -0.8578381542044509755, 18.04903173543935679, 0.4659799999690844019 ) ) ;
#31753 = AXIS2_PLACEMENT_3D ( 'NONE', #29186, #32600, #16615 ) ;
#31754 = CARTESIAN_POINT ( 'NONE',  ( 0.05603342037570913786, 10.86776798020533086, -0.9749832093204870986 ) ) ;
#31755 = EDGE_LOOP ( 'NONE', ( #7476, #3213, #33969, #32178 ) ) ;
#31756 = ORIENTED_EDGE ( 'NONE', *, *, #13641, .F. ) ;
#31757 = CARTESIAN_POINT ( 'NONE',  ( -6.070593021754335294E-14, 91.53346620154573543, 1.030917152101657972E-16 ) ) ;
#31758 = CARTESIAN_POINT ( 'NONE',  ( 5.278237183132049815, 122.2451909684448310, 0.2611397421478204861 ) ) ;
#31759 = CARTESIAN_POINT ( 'NONE',  ( -16.09504119906512898, 148.0691544347876345, 0.9470067175600013210 ) ) ;
#31760 = CARTESIAN_POINT ( 'NONE',  ( 2.948382749353823051, 50.13146620154573441, 1.837270642369387641 ) ) ;
#31761 = CARTESIAN_POINT ( 'NONE',  ( 3.302240090359226610, -14.10740904597654399, 3.820541190522989350 ) ) ;
#31762 = CARTESIAN_POINT ( 'NONE',  ( 11.48915734413142609, 123.4929228318607386, -1.183242792625787354 ) ) ;
#31763 = CIRCLE ( 'NONE', #13385, 8.794749999999998735 ) ;
#31764 = CARTESIAN_POINT ( 'NONE',  ( -13.08242246048941304, 122.4605402651681487, -1.816276721775475611 ) ) ;
#31765 = DIRECTION ( 'NONE',  ( -4.017660918040594346E-17, 1.000000000000000000, 2.376309959284834438E-19 ) ) ;
#31766 = CARTESIAN_POINT ( 'NONE',  ( 8.198496980573445114, 120.4865852927236318, 1.425346789075751852 ) ) ;
#31767 = CARTESIAN_POINT ( 'NONE',  ( 4.074910602682932925, 118.2429491485453497, -0.1454311599470143046 ) ) ;
#31768 = CARTESIAN_POINT ( 'NONE',  ( 15.28873023128500463, 143.4753230507764670, -0.02859522846259918843 ) ) ;
#31769 = TOROIDAL_SURFACE ( 'NONE', #14752, 0.7620000000000000107, 0.2540000000000000036 ) ;
#31770 = ORIENTED_EDGE ( 'NONE', *, *, #27726, .F. ) ;
#31771 = CARTESIAN_POINT ( 'NONE',  ( -2.445982073634199949, 107.2195770060406659, -4.733624241319121850 ) ) ;
#31772 = DIRECTION ( 'NONE',  ( -1.000000000000000000, -6.353134868986659519E-16, 0.000000000000000000 ) ) ;
#31773 = CARTESIAN_POINT ( 'NONE',  ( -18.58115504727956591, 80.30342350548193053, -1.270000000000003126 ) ) ;
#31774 = CARTESIAN_POINT ( 'NONE',  ( -58.63158931450232814, -0.2944865825853931751, 0.3706283016935131847 ) ) ;
#31775 = CARTESIAN_POINT ( 'NONE',  ( -2.092221094934305192, 20.21789226318614041, 8.165053130886693822 ) ) ;
#31776 = CARTESIAN_POINT ( 'NONE',  ( 10.33865867007032335, 123.8962982355681817, 1.239266749756491093 ) ) ;
#31777 = CYLINDRICAL_SURFACE ( 'NONE', #38269, 5.588000000000006295 ) ;
#31778 = CARTESIAN_POINT ( 'NONE',  ( 22.73457742531292780, 137.3553536570635742, 0.3842032436244985916 ) ) ;
#31779 = ADVANCED_FACE ( 'NONE', ( #14495 ), #33279, .T. ) ;
#31780 = CARTESIAN_POINT ( 'NONE',  ( -7.280302209287178528, 123.0424313102424492, -0.07662657258806349070 ) ) ;
#31781 = VECTOR ( 'NONE', #20310, 1000.000000000000114 ) ;
#31782 = CARTESIAN_POINT ( 'NONE',  ( -5.177913976931296069, 71.67999986514567468, -5.372099999999999653 ) ) ;
#31783 = CARTESIAN_POINT ( 'NONE',  ( -6.439802323014594534E-14, 156.3034662015457172, 9.765829976239106842E-17 ) ) ;
#31784 = CARTESIAN_POINT ( 'NONE',  ( 6.819937116507564845, -4.819529739946951885, -5.002256584970107056 ) ) ;
#31785 = CARTESIAN_POINT ( 'NONE',  ( 5.532858221982281499, 116.9390490013607717, -0.3964132980606658307 ) ) ;
#31786 = CIRCLE ( 'NONE', #18857, 0.2539999999999998925 ) ;
#31787 = CARTESIAN_POINT ( 'NONE',  ( 0.01386859376750094325, 119.8383472832138779, -0.6940411431075127480 ) ) ;
#31788 = DIRECTION ( 'NONE',  ( -5.206863593109713661E-17, 1.000000000000000000, -1.077750396879097183E-30 ) ) ;
#31789 = CARTESIAN_POINT ( 'NONE',  ( 4.773405134497627600, 114.7515004814629691, -1.662930411550287868 ) ) ;
#31790 = CARTESIAN_POINT ( 'NONE',  ( 4.815508964495446520, -10.08105153662837061, -6.929324068793707880 ) ) ;
#31791 = CARTESIAN_POINT ( 'NONE',  ( 1.569714848522641537, 117.3993836557345389, 1.461722088477706460 ) ) ;
#31792 = FACE_OUTER_BOUND ( 'NONE', #38573, .T. ) ;
#31793 = FACE_OUTER_BOUND ( 'NONE', #8487, .T. ) ;
#31794 = EDGE_CURVE ( 'NONE', #6455, #27023, #3204, .T. ) ;
#31795 = CARTESIAN_POINT ( 'NONE',  ( 0.2858543223547244105, 109.4728569552520554, -3.914881836256076664 ) ) ;
#31796 = CARTESIAN_POINT ( 'NONE',  ( -14.92885934485206079, 156.1361208441215922, 0.4494106821051805922 ) ) ;
#31797 = AXIS2_PLACEMENT_3D ( 'NONE', #4523, #40093, #23231 ) ;
#31798 = EDGE_LOOP ( 'NONE', ( #7366, #7409, #23993, #6950 ) ) ;
#31799 = CARTESIAN_POINT ( 'NONE',  ( -58.83227707057489653, -0.08366279998001102669, -5.813756590757272400E-15 ) ) ;
#31800 = ORIENTED_EDGE ( 'NONE', *, *, #37837, .F. ) ;
#31801 = CARTESIAN_POINT ( 'NONE',  ( -42.73979388487836673, 22.09733806376468124, -1.954747716862336171 ) ) ;
#31802 = CARTESIAN_POINT ( 'NONE',  ( -10.99239764355705695, 127.9870461113106472, -0.1667489162830026461 ) ) ;
#31803 = CARTESIAN_POINT ( 'NONE',  ( 5.089472049306802859, -15.08631191614791334, 3.825519591672899455 ) ) ;
#31804 = CARTESIAN_POINT ( 'NONE',  ( -12.66950698665823438, 121.4495935343099688, 1.177842983441548030 ) ) ;
#31805 = CARTESIAN_POINT ( 'NONE',  ( 14.35401710045865009, 121.2650221238243944, -0.8333810220845707661 ) ) ;
#31806 = CARTESIAN_POINT ( 'NONE',  ( 1.068493265602401987, 5.690783753869971484, 4.496582723949734017 ) ) ;
#31807 = CARTESIAN_POINT ( 'NONE',  ( -58.11310633828895789, 0.8178190558498232843, -1.239050447815041922 ) ) ;
#31808 = EDGE_CURVE ( 'NONE', #28149, #514, #25766, .T. ) ;
#31809 = ORIENTED_EDGE ( 'NONE', *, *, #36608, .T. ) ;
#31810 = CARTESIAN_POINT ( 'NONE',  ( -6.504806966450658722E-14, 124.9344662015457317, 5.107768156065721555E-17 ) ) ;
#31811 = DIRECTION ( 'NONE',  ( -0.8745520943968249084, 0.4849315768086533418, -5.271987356194193006E-16 ) ) ;
#31812 = CARTESIAN_POINT ( 'NONE',  ( -8.931878350220518570, 122.0520977060996586, 0.9029078837920736511 ) ) ;
#31813 = DIRECTION ( 'NONE',  ( -4.017660918040594346E-17, 1.000000000000000000, 2.376309959284834438E-19 ) ) ;
#31814 = CARTESIAN_POINT ( 'NONE',  ( 10.78346871132522189, 121.7859837122882283, -1.235232998807843874 ) ) ;
#31815 = CARTESIAN_POINT ( 'NONE',  ( -9.459309661781173162, 157.4068808874136209, -1.850812122078211219 ) ) ;
#31816 = CARTESIAN_POINT ( 'NONE',  ( -53.45432727069204759, 10.77832982246877691, -4.078803160923793136 ) ) ;
#31817 = CARTESIAN_POINT ( 'NONE',  ( 0.7132078119427314178, 156.3865044363621450, -0.5782112914057381259 ) ) ;
#31818 = ORIENTED_EDGE ( 'NONE', *, *, #24021, .F. ) ;
#31819 = CARTESIAN_POINT ( 'NONE',  ( -12.25802010074281512, 153.5964916033214820, -2.078998712700113938 ) ) ;
#31820 = CARTESIAN_POINT ( 'NONE',  ( 3.758269890760038034, -15.41186319813359162, 2.599103203065302292 ) ) ;
#31821 = CARTESIAN_POINT ( 'NONE',  ( -4.065972646788793554, 118.2429491485453070, -0.3080848862740693250 ) ) ;
#31822 = EDGE_CURVE ( 'NONE', #39307, #13530, #14475, .T. ) ;
#31823 = CARTESIAN_POINT ( 'NONE',  ( -47.84756666395259117, 19.38928433903615911, -5.209054514891951371 ) ) ;
#31824 = CARTESIAN_POINT ( 'NONE',  ( -4.805733446620805260, 117.6714400353627781, 0.9243893074020221867 ) ) ;
#31825 = CARTESIAN_POINT ( 'NONE',  ( 17.70445710129698114, 147.3864036964934598, 2.239206817186280674 ) ) ;
#31826 = CARTESIAN_POINT ( 'NONE',  ( -41.09670346151922615, 23.04688172092959775, 1.270085369932517194 ) ) ;
#31827 = EDGE_CURVE ( 'NONE', #27525, #22696, #37634, .T. ) ;
#31828 = CARTESIAN_POINT ( 'NONE',  ( 6.696816702757251605, -2.959147833993511778, 5.158690622954519078 ) ) ;
#31829 = CARTESIAN_POINT ( 'NONE',  ( 0.6563489144270290288, 156.3175253132196190, 0.2722359314208552261 ) ) ;
#31830 = CARTESIAN_POINT ( 'NONE',  ( -48.56815661899837977, 19.24492339269602681, -5.224590812749990931 ) ) ;
#31832 = ORIENTED_EDGE ( 'NONE', *, *, #24317, .T. ) ;
#31831 = CARTESIAN_POINT ( 'NONE',  ( -46.67338572489352089, 16.85372243840493311, -0.3683569569372189823 ) ) ;
#31833 = LINE ( 'NONE', #9261, #14861 ) ;
#31834 = CARTESIAN_POINT ( 'NONE',  ( -57.52317756609133426, 3.014644041894651405, 1.981665235817938076 ) ) ;
#31835 = CARTESIAN_POINT ( 'NONE',  ( -56.55101830787051398, 4.138461899075373651, 2.474321349783852764 ) ) ;
#31836 = FACE_OUTER_BOUND ( 'NONE', #16391, .T. ) ;
#31837 = CARTESIAN_POINT ( 'NONE',  ( -6.059261036834497460, 77.01756249999996840, -5.016499999999999737 ) ) ;
#31838 = CARTESIAN_POINT ( 'NONE',  ( -53.04800011021367112, 17.61732480354184815, -1.032319417969101073E-14 ) ) ;
#31839 = CARTESIAN_POINT ( 'NONE',  ( -13.42085051059978618, 156.9389434127184018, -0.1400394208249337025 ) ) ;
#31840 = VERTEX_POINT ( 'NONE', #16384 ) ;
#31841 = CARTESIAN_POINT ( 'NONE',  ( -49.15418877470109749, 24.05022684412165646, -0.2550087576077226803 ) ) ;
#31842 = CARTESIAN_POINT ( 'NONE',  ( -6.914645095069842817, 121.8817256395018518, -0.4219592037419029329 ) ) ;
#31843 = CARTESIAN_POINT ( 'NONE',  ( 4.999708720184146138, 117.4026903937521382, -0.8309563775561717991 ) ) ;
#31844 = ORIENTED_EDGE ( 'NONE', *, *, #27427, .F. ) ;
#31845 = CARTESIAN_POINT ( 'NONE',  ( 0.7130887386421452812, 115.7031546128015833, -1.731733134274537456 ) ) ;
#31846 = CARTESIAN_POINT ( 'NONE',  ( -7.044359374033601462, 122.0696255612902519, -0.2151282384624542410 ) ) ;
#31847 = CARTESIAN_POINT ( 'NONE',  ( 5.778079093609060024, -12.78747091716041240, 1.651671850763037463 ) ) ;
#31848 = CARTESIAN_POINT ( 'NONE',  ( -16.54768821719736138, 125.2933801378020888, 1.124873388181685252 ) ) ;
#31849 = CARTESIAN_POINT ( 'NONE',  ( 6.059261036834406866, 57.14999999999999858, -5.016499999999999737 ) ) ;
#31850 = CIRCLE ( 'NONE', #10075, 18.32410244842765934 ) ;
#31851 = CARTESIAN_POINT ( 'NONE',  ( 8.041834545246983268, 158.6767594643193604, 0.3248513814034967306 ) ) ;
#31852 = CARTESIAN_POINT ( 'NONE',  ( -0.001966947951488413372, 120.9974662015458620, 0.09843411867983418995 ) ) ;
#31853 = CARTESIAN_POINT ( 'NONE',  ( -5.008392216835970245, 117.3993836135851865, 0.7767235299482659894 ) ) ;
#31854 = CARTESIAN_POINT ( 'NONE',  ( -0.6963090749671848600, 14.53960050853193842, 0.6834203841726373962 ) ) ;
#31855 = CARTESIAN_POINT ( 'NONE',  ( -17.26848747421932018, 122.7565812399420651, -0.3979830900422687834 ) ) ;
#31856 = EDGE_CURVE ( 'NONE', #18068, #32282, #23323, .T. ) ;
#31857 = CYLINDRICAL_SURFACE ( 'NONE', #39457, 0.2540000000000023350 ) ;
#31858 = VERTEX_POINT ( 'NONE', #7035 ) ;
#31859 = CARTESIAN_POINT ( 'NONE',  ( -5.551648636414652671, 117.0334030889854233, 0.4298500987717784882 ) ) ;
#31860 = CARTESIAN_POINT ( 'NONE',  ( -58.36637034709521288, -0.2844058539389027196, -0.07201930941427876764 ) ) ;
#31861 = CARTESIAN_POINT ( 'NONE',  ( 16.99346516877617574, 153.7580772870718988, 2.083520914717074568 ) ) ;
#31862 = CARTESIAN_POINT ( 'NONE',  ( 7.743227489916772122, 119.4405053107883958, -1.058161572703685938 ) ) ;
#31863 = CARTESIAN_POINT ( 'NONE',  ( 7.903470162808407196, 13.94468365673557742, -2.927854470364564587 ) ) ;
#31864 = CARTESIAN_POINT ( 'NONE',  ( -10.97563396989523099, 119.3804150619309468, -1.219877759958876595 ) ) ;
#31865 = CARTESIAN_POINT ( 'NONE',  ( 4.844896927831375599, 117.8262454600737783, -0.6943141436239437247 ) ) ;
#31866 = CARTESIAN_POINT ( 'NONE',  ( 5.227511188233168404, 116.2365830367532595, 1.175287748399642451 ) ) ;
#31867 = B_SPLINE_CURVE_WITH_KNOTS ( 'NONE', 3,
 ( #25274, #40636, #18027, #15256, #24851, #14832, #2295, #8465, #12071, #41052 ),
 .UNSPECIFIED., .F., .F.,
 ( 4, 2, 2, 2, 4 ),
 ( 0.000000000000000000, 0.001159845853739277684, 0.002319691707478555368, 0.003479537561217833051, 0.004639383414957110735 ),
 .UNSPECIFIED. ) ;
#31868 = CARTESIAN_POINT ( 'NONE',  ( -5.978688551911978344, 155.3719879121972838, -0.01966617979267111863 ) ) ;
#31869 = EDGE_CURVE ( 'NONE', #17052, #17144, #39690, .T. ) ;
#31870 = CARTESIAN_POINT ( 'NONE',  ( -18.41737859239644948, 149.0103496150362901, -2.461622840412570845 ) ) ;
#31871 = CARTESIAN_POINT ( 'NONE',  ( 4.774069126156925691, -15.45330506282495442, 3.807469687449487772 ) ) ;
#31872 = DIRECTION ( 'NONE',  ( -0.9891443546370349837, 0.000000000000000000, -0.1469470846586743984 ) ) ;
#31873 = CARTESIAN_POINT ( 'NONE',  ( -4.862865218882401308, 117.4080073120805565, -1.166082678461140443 ) ) ;
#31874 = CARTESIAN_POINT ( 'NONE',  ( -1.957980696025146017, 117.9496056077522752, -1.362940820082817694 ) ) ;
#31875 = VERTEX_POINT ( 'NONE', #17 ) ;
#31876 = CARTESIAN_POINT ( 'NONE',  ( 15.71196619591391475, 131.3838724160208926, 2.228970979916469197 ) ) ;
#31877 = CARTESIAN_POINT ( 'NONE',  ( -6.637366883016756296E-14, 101.1854662015457365, -1.207165459283692464E-19 ) ) ;
#31878 = EDGE_CURVE ( 'NONE', #21592, #28149, #34909, .T. ) ;
#31879 = CIRCLE ( 'NONE', #13514, 0.2539999999999990599 ) ;
#31880 = AXIS2_PLACEMENT_3D ( 'NONE', #38599, #15993, #28993 ) ;
#31881 = CARTESIAN_POINT ( 'NONE',  ( -14.60500000000000043, 71.11999999999999034, 5.016499999999999737 ) ) ;
#31882 = CARTESIAN_POINT ( 'NONE',  ( -5.811537524186242365, 124.3836500214474654, -0.1011232793223458964 ) ) ;
#31883 = ADVANCED_FACE ( 'NONE', ( #16813 ), #39406, .F. ) ;
#31884 = B_SPLINE_CURVE_WITH_KNOTS ( 'NONE', 3,
 ( #5457, #2049, #31424, #25030, #8853, #21817, #34843, #5677, #30788, #31639, #24184, #8015, #14592, #27597, #11406, #22442, #12470, #25465, #12675, #25664, #6294, #9891, #125, #38671 ),
 .UNSPECIFIED., .F., .F.,
 ( 4, 2, 2, 2, 1, 2, 2, 2, 2, 1, 2, 2, 4 ),
 ( 0.000000000000000000, 0.2499999999999528155, 0.3749999999999274469, 0.4374999999999140687, 0.4687499999999092948, 0.4843749999999090172, 0.4999999999999087397, 0.6249999999999164002, 0.6874999999999221734, 0.7187499999999252820, 0.7343749999999282796, 0.7499999999999311662, 1.000000000000000000 ),
 .UNSPECIFIED. ) ;
#31885 = CARTESIAN_POINT ( 'NONE',  ( -0.3690887223898375868, -3.321408231106627973, -8.411989387140767604 ) ) ;
#31886 = CARTESIAN_POINT ( 'NONE',  ( 12.50622671840189604, 130.7145975665201831, 1.030918987520083707 ) ) ;
#31887 = CARTESIAN_POINT ( 'NONE',  ( 22.62544200675479900, 150.0155710288180444, -0.5141704484958252719 ) ) ;
#31888 = DIRECTION ( 'NONE',  ( 5.188838149069471174E-16, -1.699382548006136313E-16, -1.000000000000000000 ) ) ;
#31889 = CARTESIAN_POINT ( 'NONE',  ( -58.36308127269551704, -0.2775048351947507763, 0.1021033997340303756 ) ) ;
#31890 = CARTESIAN_POINT ( 'NONE',  ( -5.558013820752536027, 116.7166910876666606, -0.2637059437321115918 ) ) ;
#31891 = CARTESIAN_POINT ( 'NONE',  ( -4.074955089416341991, 118.2429491485453354, 0.1454234154749719787 ) ) ;
#31892 = CARTESIAN_POINT ( 'NONE',  ( 5.023959273832318218, 113.9634657096167842, -1.916936035570479202 ) ) ;
#31893 = ORIENTED_EDGE ( 'NONE', *, *, #8457, .T. ) ;
#31894 =( BOUNDED_SURFACE ( )  B_SPLINE_SURFACE ( 3, 2, ( 
 ( #13152, #22295, #42143 ),
 ( #19323, #32327, #25515 ),
 ( #3156, #38935, #34904 ),
 ( #16336, #9746, #38307 ),
 ( #26145, #16120, #22715 ),
 ( #41510, #32537, #3370 ),
 ( #15704, #5736, #18689 ),
 ( #35116, #28709, #36387 ),
 ( #29560, #26782, #34178 ),
 ( #13579, #7203, #40004 ),
 ( #5004, #27767, #10795 ),
 ( #36169, #40778, #605 ) ),
 .UNSPECIFIED., .F., .F., .F. ) 
 B_SPLINE_SURFACE_WITH_KNOTS ( ( 4, 2, 2, 2, 2, 4 ),
 ( 3, 3 ),
 ( -3.945052844332828156E-19, 0.0001838632285168906972, 0.0003677264570337817739, 0.0007354529140675639814, 0.001103179371101346189, 0.001470905828135128397 ),
 ( 0.000000000000000000, 1.000000000000000000 ),
 .UNSPECIFIED. ) 
 GEOMETRIC_REPRESENTATION_ITEM ( )  RATIONAL_B_SPLINE_SURFACE ( (
 ( 1.000000000000000000, 0.7071067811865591191, 1.000000000000000000),
 ( 1.000000000000000000, 0.7071067811865591191, 1.000000000000000000),
 ( 1.000000000000000000, 0.7071067811865436870, 1.000000000000000000),
 ( 1.000000000000000000, 0.7071067811865436870, 1.000000000000000000),
 ( 1.000000000000000000, 0.7071067811865398012, 1.000000000000000000),
 ( 1.000000000000000000, 0.7071067811865398012, 1.000000000000000000),
 ( 1.000000000000000000, 0.7071067811865398012, 1.000000000000000000),
 ( 1.000000000000000000, 0.7071067811865398012, 1.000000000000000000),
 ( 1.000000000000000000, 0.7071067811865514585, 1.000000000000000000),
 ( 1.000000000000000000, 0.7071067811865514585, 1.000000000000000000),
 ( 1.000000000000000000, 0.7071067811865475727, 1.000000000000000000),
 ( 1.000000000000000000, 0.7071067811865475727, 1.000000000000000000) ) ) 
 REPRESENTATION_ITEM ( '' )  SURFACE ( )  );
#31895 = CARTESIAN_POINT ( 'NONE',  ( -4.666616009249764829, 119.7854802332205537, -0.9105328040180735716 ) ) ;
#31896 = CARTESIAN_POINT ( 'NONE',  ( 5.256943553860875973, 116.0444662015457027, 1.293952898321280021 ) ) ;
#31897 = CARTESIAN_POINT ( 'NONE',  ( -15.89661694251515556, 145.9828583539951126, -0.9138632209041558374 ) ) ;
#31898 = LINE ( 'NONE', #29111, #10411 ) ;
#31899 = CARTESIAN_POINT ( 'NONE',  ( 23.21373371908085304, 149.6306211361744829, 0.4638656453230914356 ) ) ;
#31900 = B_SPLINE_CURVE_WITH_KNOTS ( 'NONE', 3,
 ( #31955, #19571, #9787, #32164, #12570, #15959 ),
 .UNSPECIFIED., .F., .F.,
 ( 4, 2, 4 ),
 ( 0.0007477044786394815333, 0.001108740074962825213, 0.001469775671286169001 ),
 .UNSPECIFIED. ) ;
#31901 = VERTEX_POINT ( 'NONE', #19576 ) ;
#31902 = CARTESIAN_POINT ( 'NONE',  ( -1.576536484031922480, 10.66345178295009788, -4.350723848753511369 ) ) ;
#31903 = CARTESIAN_POINT ( 'NONE',  ( -4.917116127314222318, 105.1214984364436020, 2.097186129389184917 ) ) ;
#31904 = CARTESIAN_POINT ( 'NONE',  ( -4.923269767626008431, 117.4099945271726142, 0.9488514777737178107 ) ) ;
#31905 = DIRECTION ( 'NONE',  ( 0.9336303900108815501, 0.3582377630124009560, 4.235673982319039874E-16 ) ) ;
#31906 = CYLINDRICAL_SURFACE ( 'NONE', #5817, 0.5080000000000007843 ) ;
#31907 = CARTESIAN_POINT ( 'NONE',  ( 6.999671179798840015, 121.6295281583065133, 0.7244140712011665206 ) ) ;
#31908 = VECTOR ( 'NONE', #38501, 1000.000000000000000 ) ;
#31909 = CARTESIAN_POINT ( 'NONE',  ( 3.724956840101937505, 21.94285949141939440, 2.734508905299370518 ) ) ;
#31910 = CARTESIAN_POINT ( 'NONE',  ( 8.073283135001478428, 117.9965348323767671, 0.8851005009521595301 ) ) ;
#31911 = CARTESIAN_POINT ( 'NONE',  ( 2.862426770350078531, 104.6144662015457101, -3.896337952179533826 ) ) ;
#31913 = CARTESIAN_POINT ( 'NONE',  ( 19.06828360855645599, 152.1029585079319020, -1.398049597035978087 ) ) ;
#31912 = CARTESIAN_POINT ( 'NONE',  ( 4.224297255521886285, 111.8944766893745424, 2.913178037176576307 ) ) ;
#31914 = CARTESIAN_POINT ( 'NONE',  ( -11.27566272104538569, 154.5781333488962446, 1.670651684902624057 ) ) ;
#31915 = AXIS2_PLACEMENT_3D ( 'NONE', #36997, #11835, #31643 ) ;
#31916 = CARTESIAN_POINT ( 'NONE',  ( -0.2796867633624597893, 20.41853924017881283, 4.627572958784220702 ) ) ;
#31917 = CARTESIAN_POINT ( 'NONE',  ( -22.93196816944047001, 148.6798292920915117, -1.431318312106270252 ) ) ;
#31918 = ORIENTED_EDGE ( 'NONE', *, *, #27142, .F. ) ;
#31919 = EDGE_CURVE ( 'NONE', #7672, #38078, #32584, .T. ) ;
#31920 = CARTESIAN_POINT ( 'NONE',  ( -57.22211421646271390, 1.778355698664496609, 0.1074917508089385937 ) ) ;
#31921 = CARTESIAN_POINT ( 'NONE',  ( -9.326662024493499459, 153.8845013697122965, 0.4488502173044094379 ) ) ;
#31922 = CARTESIAN_POINT ( 'NONE',  ( 2.071654280177509300, -15.34349575202162441, 5.977339193430266207 ) ) ;
#31923 = LINE ( 'NONE', #12945, #27496 ) ;
#31924 = CARTESIAN_POINT ( 'NONE',  ( -4.660057157337337941, 118.0075560824071630, -0.7769649848974667927 ) ) ;
#31925 = CARTESIAN_POINT ( 'NONE',  ( 0.6438746309740379647, 120.9974662015465867, 0.01286614746332145724 ) ) ;
#31926 = VERTEX_POINT ( 'NONE', #10000 ) ;
#31927 = CARTESIAN_POINT ( 'NONE',  ( 4.492596771379812282, 157.9011380394538833, 1.833279187945892952 ) ) ;
#31928 = CARTESIAN_POINT ( 'NONE',  ( 5.177913976931214357, 57.15000000000004832, 5.372099999999999653 ) ) ;
#31929 = CARTESIAN_POINT ( 'NONE',  ( 14.73199999999999932, 12.96416000000000146, 0.000000000000000000 ) ) ;
#31930 = EDGE_CURVE ( 'NONE', #31070, #12640, #32195, .T. ) ;
#31931 = CARTESIAN_POINT ( 'NONE',  ( 4.866147868668515564, 117.4089627612368076, -0.9906677743061890196 ) ) ;
#31932 = CARTESIAN_POINT ( 'NONE',  ( 18.56067064112282594, 154.1690995007799927, -0.05235235476399361515 ) ) ;
#31933 = AXIS2_PLACEMENT_3D ( 'NONE', #7198, #11208, #11414 ) ;
#31934 = AXIS2_PLACEMENT_3D ( 'NONE', #34110, #40709, #12144 ) ;
#31935 = LINE ( 'NONE', #21478, #34987 ) ;
#31936 = CARTESIAN_POINT ( 'NONE',  ( -10.45888906141547992, 56.51499999999998636, 4.393716635381797353 ) ) ;
#31937 = CARTESIAN_POINT ( 'NONE',  ( -46.60530155212504155, 26.17382724835476537, 0.4656666666666581800 ) ) ;
#31938 = CARTESIAN_POINT ( 'NONE',  ( 2.032084454478232161, -15.08528485642818318, 5.800687065324998670 ) ) ;
#31939 = CARTESIAN_POINT ( 'NONE',  ( -48.38589991294942649, 19.15920805527091630, 5.452675306770309760 ) ) ;
#31940 = DIRECTION ( 'NONE',  ( -1.000000000000000000, 9.563967653961371147E-17, 0.000000000000000000 ) ) ;
#31941 = CARTESIAN_POINT ( 'NONE',  ( -4.625339627765448824, 118.0227720238258087, 0.6694514315784764191 ) ) ;
#31942 = VERTEX_POINT ( 'NONE', #3634 ) ;
#31943 = CARTESIAN_POINT ( 'NONE',  ( -0.4613933488989553910, 118.7629491485454025, -1.278559111267616455 ) ) ;
#31944 = CARTESIAN_POINT ( 'NONE',  ( -8.329558457569385510, 119.8456229460195885, -1.441662697695123008 ) ) ;
#31945 = CARTESIAN_POINT ( 'NONE',  ( -4.398525312958116551, 119.2572634999566930, -0.5937511404893218714 ) ) ;
#31946 = CARTESIAN_POINT ( 'NONE',  ( 4.599167112255276635, 117.9522226071726436, 0.9463719716926317638 ) ) ;
#31947 = CARTESIAN_POINT ( 'NONE',  ( 3.198224922426783579, -14.19254063666773291, 2.189163805996276579 ) ) ;
#31948 = CARTESIAN_POINT ( 'NONE',  ( -11.15578272721385211, 126.1638007343821641, -1.112962985253807657 ) ) ;
#31949 = FACE_OUTER_BOUND ( 'NONE', #33455, .T. ) ;
#31950 = CARTESIAN_POINT ( 'NONE',  ( -4.416771755448872128, 71.99420641645033925, 1.524000000000005128 ) ) ;
#31951 = CARTESIAN_POINT ( 'NONE',  ( 5.362262919126890459, 116.9387654363850260, -0.7435593652664852504 ) ) ;
#31952 = CARTESIAN_POINT ( 'NONE',  ( -10.79589323670149525, 123.3109526380878833, -1.504350731661493912 ) ) ;
#31953 = CARTESIAN_POINT ( 'NONE',  ( 18.86374853661768825, 125.3403196291361610, 0.3769425889880999581 ) ) ;
#31954 = CARTESIAN_POINT ( 'NONE',  ( 5.274109024393328404, 115.7029491485453150, -0.8140283081321302294 ) ) ;
#31955 = CARTESIAN_POINT ( 'NONE',  ( 5.348924234570989533, 56.51499999999999346, -4.492130288940734850 ) ) ;
#31956 = CARTESIAN_POINT ( 'NONE',  ( 1.616848224653315569, 9.589005055319924864, -4.350374724214612243 ) ) ;
#31958 = ORIENTED_EDGE ( 'NONE', *, *, #32666, .T. ) ;
#31957 = CARTESIAN_POINT ( 'NONE',  ( 21.11962238282686499, 132.3956117394162106, 1.087766252141818324 ) ) ;
#31959 = CARTESIAN_POINT ( 'NONE',  ( 3.569197635593082563, 104.6144662015456959, -3.263097013630751775 ) ) ;
#31960 = CARTESIAN_POINT ( 'NONE',  ( 1.983586949722073500, -15.35435952563934947, 5.265070481109153988 ) ) ;
#31961 = CARTESIAN_POINT ( 'NONE',  ( -12.54292998015204752, 122.5542284311838870, 1.320227961537941086 ) ) ;
#31962 = CARTESIAN_POINT ( 'NONE',  ( -0.2236011429256814231, 15.24623788552754888, -0.9474642044971398613 ) ) ;
#31963 = CARTESIAN_POINT ( 'NONE',  ( 0.7290388503741822568, 0.07276798020498101427, -0.6497956273326017662 ) ) ;
#31964 = ORIENTED_EDGE ( 'NONE', *, *, #4603, .T. ) ;
#31965 = AXIS2_PLACEMENT_3D ( 'NONE', #27158, #13544, #16725 ) ;
#31966 = VERTEX_POINT ( 'NONE', #23179 ) ;
#31967 = CARTESIAN_POINT ( 'NONE',  ( -4.973569738608247803, 117.3993868453981548, -0.9750659555622913643 ) ) ;
#31968 = CARTESIAN_POINT ( 'NONE',  ( 4.275575466068057828, 118.7880935209305591, 0.6699701396488104699 ) ) ;
#31969 = DIRECTION ( 'NONE',  ( 1.000000000000000000, 0.000000000000000000, 0.000000000000000000 ) ) ;
#31970 = CARTESIAN_POINT ( 'NONE',  ( -9.727312926402552407, 123.7664141286412871, 0.5879621312111034115 ) ) ;
#31971 = CARTESIAN_POINT ( 'NONE',  ( -8.981069108608934926, 123.9698733229553937, -0.1794631345465900474 ) ) ;
#31972 = CARTESIAN_POINT ( 'NONE',  ( 3.119424175201863214, -14.34824051949108714, 4.229366443754182470 ) ) ;
#31973 = CARTESIAN_POINT ( 'NONE',  ( 9.240212912644766519, 121.6705353891887995, -1.055487293716821817 ) ) ;
#31974 = CARTESIAN_POINT ( 'NONE',  ( -12.43266001442903068, 122.1796674805547980, -1.793313828261402065 ) ) ;
#31975 = DIRECTION ( 'NONE',  ( 1.000000000000000000, 2.185478394931408997E-15, 0.000000000000000000 ) ) ;
#31976 = LINE ( 'NONE', #22357, #8398 ) ;
#31977 = CARTESIAN_POINT ( 'NONE',  ( -5.561288968297983359, 31.82205145332388341, 3.034443710062491917 ) ) ;
#31978 = CARTESIAN_POINT ( 'NONE',  ( 15.33898570969095942, 143.5038931315047535, -0.1524207748662384510 ) ) ;
#31979 = EDGE_LOOP ( 'NONE', ( #33823, #2035, #18318, #9470 ) ) ;
#31980 = CARTESIAN_POINT ( 'NONE',  ( 3.177488185987922709, -14.13217061847354472, 2.003775387181677026 ) ) ;
#31981 = CYLINDRICAL_SURFACE ( 'NONE', #20359, 0.2540000000000006142 ) ;
#31982 = CARTESIAN_POINT ( 'NONE',  ( 17.14499999999999957, 71.11999999999999034, 5.016499999999999737 ) ) ;
#31983 = CARTESIAN_POINT ( 'NONE',  ( -58.54549369844274054, -0.1193337916060716042, 0.6006683616752106492 ) ) ;
#31984 = CARTESIAN_POINT ( 'NONE',  ( -4.326994387844902867, 19.77997674669536465, 7.266063235268683584 ) ) ;
#31985 = CARTESIAN_POINT ( 'NONE',  ( 11.23392777908751761, 153.2158294759273360, 1.564101052410651338 ) ) ;
#31986 = CARTESIAN_POINT ( 'NONE',  ( -6.585902005698190595E-14, 91.53346620154573543, 1.207165459464729879E-19 ) ) ;
#31987 = CARTESIAN_POINT ( 'NONE',  ( 9.815320032039958065, 117.9943556427423488, 0.1502691370658186254 ) ) ;
#31988 = CARTESIAN_POINT ( 'NONE',  ( -4.033305401784485156, 109.8300753404742096, 3.515372713824419737 ) ) ;
#31989 = CARTESIAN_POINT ( 'NONE',  ( -8.216341275949833545, 69.50096819940942794, -1.269999999999995799 ) ) ;
#31990 = CARTESIAN_POINT ( 'NONE',  ( 5.964965236245641123, 155.3820107761045790, 0.1591880423168910430 ) ) ;
#31991 = CARTESIAN_POINT ( 'NONE',  ( 18.34395142906165077, 131.7683309214445728, 2.187682908440788054 ) ) ;
#31992 = CARTESIAN_POINT ( 'NONE',  ( 8.062851560922409178, 27.27981867468588462, -2.430221966868060690 ) ) ;
#31993 = CARTESIAN_POINT ( 'NONE',  ( 2.189084557043657675, 116.7689930370939919, -0.4207698416637195571 ) ) ;
#31994 = CARTESIAN_POINT ( 'NONE',  ( -0.3588522330933500704, 120.9711055683163323, -0.4900691623393883534 ) ) ;
#31995 = CARTESIAN_POINT ( 'NONE',  ( 4.560443946511397506, -11.68866997254031936, 0.6947937310338139216 ) ) ;
#31996 = CARTESIAN_POINT ( 'NONE',  ( -0.1568781454184781377, 105.9760921070151767, -5.301024823544129738 ) ) ;
#31997 = CARTESIAN_POINT ( 'NONE',  ( 0.2838385327444274964, 29.22985346960623332, -4.617364983570896086 ) ) ;
#31998 = CARTESIAN_POINT ( 'NONE',  ( -4.800085724567980883, 115.7029491485352537, -1.472342921364584889 ) ) ;
#31999 = DIRECTION ( 'NONE',  ( 6.353134868986659519E-16, -1.000000000000000000, 0.000000000000000000 ) ) ;
#32000 = CARTESIAN_POINT ( 'NONE',  ( 3.162461164278121739, -14.57801340048104777, 3.369881103115548893 ) ) ;
#32001 = CARTESIAN_POINT ( 'NONE',  ( 0.3839444928496320020, 119.8383472832136931, -0.6866461459122011890 ) ) ;
#32002 = CARTESIAN_POINT ( 'NONE',  ( -3.207477133065458563, 159.4163042773305676, 0.4796247595147200005 ) ) ;
#32003 = ORIENTED_EDGE ( 'NONE', *, *, #24798, .T. ) ;
#32004 = CARTESIAN_POINT ( 'NONE',  ( -41.23752580366542730, 23.26788267949596190, 1.523999999999994248 ) ) ;
#32005 = ORIENTED_EDGE ( 'NONE', *, *, #22941, .F. ) ;
#32006 = CARTESIAN_POINT ( 'NONE',  ( -17.14500000000466784, 71.11999999999886768, 1.269999999999998241 ) ) ;
#32007 = CARTESIAN_POINT ( 'NONE',  ( 2.810429210790068133, -15.63944505633836712, 5.584101034811558506 ) ) ;
#32008 = CARTESIAN_POINT ( 'NONE',  ( -13.26531225419064519, 121.8780043825237982, 1.199064809579205360 ) ) ;
#32009 = VECTOR ( 'NONE', #32119, 1000.000000000000000 ) ;
#32010 = CARTESIAN_POINT ( 'NONE',  ( 21.83021172428700751, 149.6930991844618291, -1.147003836765864371 ) ) ;
#32011 = CARTESIAN_POINT ( 'NONE',  ( -2.948169924849943335, 1.592661447142720732, -3.562413953034572867 ) ) ;
#32012 = CARTESIAN_POINT ( 'NONE',  ( -57.39852392895783595, 2.352836174085538357, -1.895304619997750128 ) ) ;
#32013 = ORIENTED_EDGE ( 'NONE', *, *, #10470, .T. ) ;
#32014 = CARTESIAN_POINT ( 'NONE',  ( -58.43299954449003764, -0.3955325680175592606, -0.3375922266956626894 ) ) ;
#32015 = CARTESIAN_POINT ( 'NONE',  ( 0.3991458833604034084, 123.7646714092001190, 0.1312610764096186766 ) ) ;
#32016 = CARTESIAN_POINT ( 'NONE',  ( -3.911441847776591985, 70.75305732235845824, -1.269999999999993801 ) ) ;
#32017 = B_SPLINE_SURFACE_WITH_KNOTS ( 'NONE', 3, 3, ( 
 ( #38600, #11761, #22373, #1984, #27947, #40956, #37750, #26434, #19197, #25797, #39438, #35826, #682, #32204, #9824, #6642, #20030 ),
 ( #32618, #29420, #13446, #47, #22790, #23211, #260, #39223, #32410, #10033, #13654, #22583, #10241, #28994, #3451, #9614, #16198 ),
 ( #16628, #10456, #3240, #26644, #33048, #36245, #35615, #42010, #16414, #7066, #3879, #16844, #6429, #19606, #13235, #15994, #23005 ),
 ( #29844, #36033, #39651, #29203, #35398, #3037, #12806, #26218, #473, #38803, #6226, #19402, #13013, #6847, #19817, #26006, #39016 ),
 ( #32834, #3663, #29635, #1522, #20446, #33473, #7697, #17884, #39865, #21074, #890, #7274, #27069, #36454, #33262, #17266, #11085 ),
 ( #10872, #17469, #23860, #20865, #17673, #40292, #1726, #14065, #4303, #23643, #36665, #1311, #30256, #1097, #33890, #24277, #36879 ) ),
 .UNSPECIFIED., .F., .F., .F.,
 ( 4, 2, 4 ),
 ( 4, 1, 1, 1, 1, 1, 1, 1, 1, 1, 1, 1, 1, 1, 4 ),
 ( 0.000000000000000000, 0.4999999999999997780, 1.000000000000000000 ),
 ( 0.000000000000000000, 0.08300113939718137268, 0.1732806554784933895, 0.2717672377176819087, 0.3752096606209606167, 0.4787223716043260135, 0.5772295444745598747, 0.6668133826162351285, 0.7470991451079272982, 0.7815930070524458317, 0.8169452614683294644, 0.8547689062991584708, 0.8968063284581728745, 0.9447228702782888288, 1.000000000000000000 ),
 .UNSPECIFIED. ) ;
#32018 = CARTESIAN_POINT ( 'NONE',  ( -16.16280394421536215, 139.8573806175465961, 1.392748567604541909 ) ) ;
#32019 = DIRECTION ( 'NONE',  ( -0.8745520943968235761, 0.4849315768086558398, -5.691349986800547879E-16 ) ) ;
#32020 = CARTESIAN_POINT ( 'NONE',  ( 18.96108613168456358, 147.8663216482595146, -1.723626476717959211 ) ) ;
#32021 = CIRCLE ( 'NONE', #3448, 0.2540000000000045555 ) ;
#32022 = CARTESIAN_POINT ( 'NONE',  ( -6.974227900756753584, 158.0922581832940921, -1.731937547952115297 ) ) ;
#32023 = CARTESIAN_POINT ( 'NONE',  ( -55.65298819915649631, 5.540485941798511504, -2.823722248809264368 ) ) ;
#32024 = ORIENTED_EDGE ( 'NONE', *, *, #24223, .F. ) ;
#32025 = CARTESIAN_POINT ( 'NONE',  ( 3.641174103387447403, 120.8049117488720015, -0.2662595081522518559 ) ) ;
#32026 = EDGE_LOOP ( 'NONE', ( #41780, #10116, #41653, #236 ) ) ;
#32027 = CARTESIAN_POINT ( 'NONE',  ( -17.92322948971689911, 147.1528319293316542, -2.295422193410857403 ) ) ;
#32028 = CARTESIAN_POINT ( 'NONE',  ( 2.500182370989485925, -15.36189011820890471, 4.810483652035355107 ) ) ;
#32029 = CARTESIAN_POINT ( 'NONE',  ( -4.146183484540335584, 118.2391778865621745, -0.3987970906756914680 ) ) ;
#32030 = EDGE_CURVE ( 'NONE', #35273, #40327, #7024, .T. ) ;
#32031 = CARTESIAN_POINT ( 'NONE',  ( -58.28497307353767809, -0.1385909279409680561, -1.048413496073990905E-14 ) ) ;
#32032 = CARTESIAN_POINT ( 'NONE',  ( -4.906328757273882957, 117.7163485839802064, 0.7384961846826334497 ) ) ;
#32033 = CARTESIAN_POINT ( 'NONE',  ( 15.61558020634879007, 150.8349565870724120, 2.213412335539846509 ) ) ;
#32034 = CARTESIAN_POINT ( 'NONE',  ( -17.14500000000466784, 71.11999999999886768, -1.524000000000000909 ) ) ;
#32035 = VECTOR ( 'NONE', #2108, 999.9999999999998863 ) ;
#32036 = CARTESIAN_POINT ( 'NONE',  ( -2.768688662514669385, 30.30441277318858795, -3.700580903672975541 ) ) ;
#32037 = CARTESIAN_POINT ( 'NONE',  ( 8.927705404389048027, 123.7033391712731145, 0.4040904458349093287 ) ) ;
#32038 = LINE ( 'NONE', #22215, #18765 ) ;
#32039 = CARTESIAN_POINT ( 'NONE',  ( -49.09053848811835508, 14.44377425990215436, -0.7907028275641611037 ) ) ;
#32040 = CARTESIAN_POINT ( 'NONE',  ( -6.442660433036017764, 29.32943145771791649, -0.01012415147099491285 ) ) ;
#32041 = AXIS2_PLACEMENT_3D ( 'NONE', #33254, #14058, #8094 ) ;
#32042 = CARTESIAN_POINT ( 'NONE',  ( -46.67299067999364581, 26.04487158941909897, -1.318362843711971211 ) ) ;
#32043 = CARTESIAN_POINT ( 'NONE',  ( -49.89905798257149883, 16.45710724715066320, 4.946581931842602309 ) ) ;
#32044 = CARTESIAN_POINT ( 'NONE',  ( -8.631383859283502602, 118.4111954750946296, -1.057371476713716785 ) ) ;
#32045 = CARTESIAN_POINT ( 'NONE',  ( -5.475330206976889436, 77.01756249999996840, -5.107412922131463695 ) ) ;
#32046 = CARTESIAN_POINT ( 'NONE',  ( -56.07077906059188166, 6.725046902222183931, 2.233835758070424671 ) ) ;
#32047 = CARTESIAN_POINT ( 'NONE',  ( -18.59469708476141747, 154.1615476314759974, -0.06268175667117097116 ) ) ;
#32048 = ORIENTED_EDGE ( 'NONE', *, *, #7941, .F. ) ;
#32049 = CARTESIAN_POINT ( 'NONE',  ( -54.68491514712287227, 9.937145987696780480, -2.757516356780049804 ) ) ;
#32050 = CARTESIAN_POINT ( 'NONE',  ( -7.809620049061188674, 122.4698989756058864, -0.5308360719997577970 ) ) ;
#32051 = PLANE ( 'NONE',  #38722 ) ;
#32052 = ORIENTED_EDGE ( 'NONE', *, *, #38139, .F. ) ;
#32053 = CARTESIAN_POINT ( 'NONE',  ( 1.844371434233660345, 115.7029491485453718, -1.651278223000081757 ) ) ;
#32054 = CARTESIAN_POINT ( 'NONE',  ( -15.72560005962105123, 146.8994026175788008, -0.4425663129111795380 ) ) ;
#32055 = CARTESIAN_POINT ( 'NONE',  ( 5.397943591185104140, -12.01093657298729589, 0.9516947191793155847 ) ) ;
#32056 = CARTESIAN_POINT ( 'NONE',  ( -14.39412078427935882, 121.9874158357064857, 1.026313471838276481 ) ) ;
#32057 = CARTESIAN_POINT ( 'NONE',  ( -22.95370498042275642, 82.54569470718179502, -1.524000000000005794 ) ) ;
#32058 = CARTESIAN_POINT ( 'NONE',  ( 1.837930215757002772, 116.5452236745340429, 0.1764961812833933386 ) ) ;
#32059 = CARTESIAN_POINT ( 'NONE',  ( 5.965539070479145778, 121.5454242706025383, 0.2305103670981815123 ) ) ;
#32060 = CARTESIAN_POINT ( 'NONE',  ( 5.175750742582734709, 115.6909491485453145, -1.072434772098743716 ) ) ;
#32061 = CARTESIAN_POINT ( 'NONE',  ( -0.6518678778066554491, 5.040965284779599820, 0.7259998264446282379 ) ) ;
#32062 = EDGE_CURVE ( 'NONE', #3374, #23884, #31487, .T. ) ;
#32063 = CARTESIAN_POINT ( 'NONE',  ( -9.792313404876155758, 118.0024801742749929, -0.3345192158099827839 ) ) ;
#32064 = B_SPLINE_CURVE_WITH_KNOTS ( 'NONE', 3,
 ( #22472, #13122, #19294, #16090, #9306, #42113, #3561, #12496, #29312, #2718, #35502 ),
 .UNSPECIFIED., .F., .F.,
 ( 4, 1, 1, 1, 1, 1, 1, 1, 4 ),
 ( 0.000000000000000000, 0.1250000000000006939, 0.2500000000000013878, 0.3750000000000020539, 0.5000000000000027756, 0.6250000000000061062, 0.7499999999999986677, 0.8750000000000019984, 1.000000000000000000 ),
 .UNSPECIFIED. ) ;
#32065 = DIRECTION ( 'NONE',  ( -0.8745520943968243532, 0.4849315768086547296, -6.829619984160642269E-16 ) ) ;
#32066 = DIRECTION ( 'NONE',  ( 0.8572391118119511155, 0.5149185422762101449, 3.573031421855331076E-16 ) ) ;
#32067 = VERTEX_POINT ( 'NONE', #26613 ) ;
#32068 = CARTESIAN_POINT ( 'NONE',  ( -5.607450786634617046, 117.5654562724977694, 0.7054197920332473393 ) ) ;
#32069 = VERTEX_POINT ( 'NONE', #39620 ) ;
#32070 = CARTESIAN_POINT ( 'NONE',  ( -58.36783630777247822, -0.2874788285674993449, -0.05365640064145733856 ) ) ;
#32071 = CARTESIAN_POINT ( 'NONE',  ( 2.834005798679493093, 158.8946464937287999, 1.432308184773210424 ) ) ;
#32072 = CARTESIAN_POINT ( 'NONE',  ( 15.79478014299080435, 153.2725199748809928, -1.714666983805330558 ) ) ;
#32073 = CARTESIAN_POINT ( 'NONE',  ( -0.5057995593169576365, 15.89392266832286182, -8.404578209849391968 ) ) ;
#32074 = CARTESIAN_POINT ( 'NONE',  ( -18.58655447097580549, 128.6297099747515347, -1.738804191113343833 ) ) ;
#32075 = CARTESIAN_POINT ( 'NONE',  ( 4.696390023408538283, 117.9631523383233969, -0.7094749930045800568 ) ) ;
#32076 = AXIS2_PLACEMENT_3D ( 'NONE', #11319, #37516, #18122 ) ;
#32077 = CARTESIAN_POINT ( 'NONE',  ( 14.91134437184010864, 120.3281135999119158, 0.2979641475767020875 ) ) ;
#32078 = CARTESIAN_POINT ( 'NONE',  ( -10.26263990951799165, 126.0184183664171655, -0.1119868329536247709 ) ) ;
#32079 = CARTESIAN_POINT ( 'NONE',  ( -12.88625155327550331, 123.9867020804889961, -1.879256283450041032 ) ) ;
#32080 = CARTESIAN_POINT ( 'NONE',  ( 2.577823224604873786, -15.72362945599133077, 5.534267358606157039 ) ) ;
#32081 = AXIS2_PLACEMENT_3D ( 'NONE', #8041, #33406, #4865 ) ;
#32082 = DIRECTION ( 'NONE',  ( -0.9998004120163609398, 0.000000000000000000, -0.01997839162482749342 ) ) ;
#32083 = EDGE_CURVE ( 'NONE', #2129, #16441, #19251, .T. ) ;
#32084 = CARTESIAN_POINT ( 'NONE',  ( -47.61549956331938205, 19.66157307908738261, -5.197827534590572895 ) ) ;
#32085 = ORIENTED_EDGE ( 'NONE', *, *, #22477, .F. ) ;
#32086 = CARTESIAN_POINT ( 'NONE',  ( -0.01111639999525440396, 119.1634951276629550, 0.5563101126475827884 ) ) ;
#32087 = CARTESIAN_POINT ( 'NONE',  ( -5.177913976931285411, 57.14999999999998437, 5.372100000000002318 ) ) ;
#32088 = CIRCLE ( 'NONE', #1493, 4.826000000000001400 ) ;
#32089 = CARTESIAN_POINT ( 'NONE',  ( -20.05275907367747124, 79.68882802557934042, 1.269999999999994467 ) ) ;
#32090 = CARTESIAN_POINT ( 'NONE',  ( -3.676218128927596140, 120.6652674781340551, 0.2791188998294429346 ) ) ;
#32091 = CARTESIAN_POINT ( 'NONE',  ( -7.004517537292900720, 30.72436916340981838, -4.697416855195242213 ) ) ;
#32092 = CARTESIAN_POINT ( 'NONE',  ( 3.627630705028838776, 120.8049117488720015, 0.4115075270184373468 ) ) ;
#32093 = EDGE_CURVE ( 'NONE', #31609, #31858, #22553, .T. ) ;
#32094 = CARTESIAN_POINT ( 'NONE',  ( 21.87092457242483334, 136.8312970274703844, -0.6093905233339393934 ) ) ;
#32095 = B_SPLINE_CURVE_WITH_KNOTS ( 'NONE', 3,
 ( #23914, #30309, #7955, #17940, #27745, #30942, #10924, #40344, #37134, #17319, #17726, #8367, #34155, #30729, #21127 ),
 .UNSPECIFIED., .F., .F.,
 ( 4, 2, 2, 2, 1, 2, 2, 4 ),
 ( 0.5000000000000000000, 0.5624999999999930056, 0.6249999999999928946, 0.7500000000000000000, 0.7812499999999951150, 0.8749999999999963363, 0.9374999999999982236, 1.000000000000000000 ),
 .UNSPECIFIED. ) ;
#32096 = CARTESIAN_POINT ( 'NONE',  ( -17.99070523305417169, 61.93444992276926797, 1.269999999999999574 ) ) ;
#32097 = CIRCLE ( 'NONE', #10334, 0.5080000000000002292 ) ;
#32098 = DIRECTION ( 'NONE',  ( 5.188838149069472160E-16, -1.699382548006136559E-16, -1.000000000000000000 ) ) ;
#32099 = CIRCLE ( 'NONE', #14386, 0.5080000000000002292 ) ;
#32100 = UNCERTAINTY_MEASURE_WITH_UNIT (LENGTH_MEASURE( 1.000000000000000082E-05 ), #40319, 'distance_accuracy_value', 'NONE');
#32101 = CARTESIAN_POINT ( 'NONE',  ( -0.0007535234283144901868, 116.4338605912342786, 0.03770939363766612207 ) ) ;
#32102 = PRODUCT_RELATED_PRODUCT_CATEGORY ( 'part', '', ( #35769 ) ) ;
#32103 = ORIENTED_EDGE ( 'NONE', *, *, #30517, .F. ) ;
#32104 = CARTESIAN_POINT ( 'NONE',  ( 4.491921773069756263, 119.5748936864404754, -0.7466653829840709244 ) ) ;
#32105 = CARTESIAN_POINT ( 'NONE',  ( 4.840862041047174991, -14.92388815503642441, 4.310681236375266678 ) ) ;
#32106 = CARTESIAN_POINT ( 'NONE',  ( -7.635798533888348061, 122.3449549946481056, -0.5106263504299666245 ) ) ;
#32107 = DIRECTION ( 'NONE',  ( 0.9998004120163608288, 0.000000000000000000, 0.01997839162482749342 ) ) ;
#32108 = CARTESIAN_POINT ( 'NONE',  ( 2.735903701988537051, 116.5290148844309357, 0.06805092059891054701 ) ) ;
#32109 = VERTEX_POINT ( 'NONE', #14446 ) ;
#32110 = CARTESIAN_POINT ( 'NONE',  ( 3.700881553190929374, 8.714383148187751615, -2.768892949411812854 ) ) ;
#32111 = EDGE_CURVE ( 'NONE', #27588, #11942, #36283, .T. ) ;
#32112 = CARTESIAN_POINT ( 'NONE',  ( -29.24370919313948036, 62.65993627036882430, 1.269999999999993801 ) ) ;
#32113 = CARTESIAN_POINT ( 'NONE',  ( -13.46199999999999264, 17.14499999999999957, 0.000000000000000000 ) ) ;
#32114 = CARTESIAN_POINT ( 'NONE',  ( 3.204964616970041646, 108.0380215227886680, 4.255332277598883550 ) ) ;
#32115 = CARTESIAN_POINT ( 'NONE',  ( -7.016717161013801274, 121.3008223241220662, 0.6504084514987088506 ) ) ;
#32116 = EDGE_CURVE ( 'NONE', #7000, #18324, #33653, .T. ) ;
#32117 = CARTESIAN_POINT ( 'NONE',  ( -1.246715508051662535, 10.49814879194060069, 4.449005273994115939 ) ) ;
#32118 = CARTESIAN_POINT ( 'NONE',  ( 12.78669781772265956, 156.8686255264331635, 1.389142476906146895 ) ) ;
#32119 = DIRECTION ( 'NONE',  ( -6.353134868986659519E-16, 1.000000000000000000, -0.000000000000000000 ) ) ;
#32121 = CARTESIAN_POINT ( 'NONE',  ( 17.54996479678707288, 128.5781302034472162, -1.330722490425295446 ) ) ;
#32120 = CARTESIAN_POINT ( 'NONE',  ( 3.116451998213339625, -14.00698646007624149, 1.619014592372306716 ) ) ;
#32122 = CARTESIAN_POINT ( 'NONE',  ( -3.984361711520921556, 7.699456178644025428, -2.362637291489932068 ) ) ;
#32123 = CARTESIAN_POINT ( 'NONE',  ( -16.55455218413314356, 122.7279807066903032, -1.056987703419675739 ) ) ;
#32124 = EDGE_CURVE ( 'NONE', #5098, #38197, #38226, .T. ) ;
#32125 = VERTEX_POINT ( 'NONE', #4898 ) ;
#32126 = CARTESIAN_POINT ( 'NONE',  ( -8.223969002016936258, 122.7966848691156514, 0.2142357769474922125 ) ) ;
#32127 = CARTESIAN_POINT ( 'NONE',  ( 5.090702275550843758, -14.49510550894771121, 4.025111979839017806 ) ) ;
#32128 = DIRECTION ( 'NONE',  ( -0.01997839162482737546, -1.040247600000939284E-18, 0.9998004120163610509 ) ) ;
#32129 = AXIS2_PLACEMENT_3D ( 'NONE', #13246, #23437, #3048 ) ;
#32130 = CARTESIAN_POINT ( 'NONE',  ( -4.599484297918647435, 117.9522697134765963, -0.9462753457481243302 ) ) ;
#32131 = CARTESIAN_POINT ( 'NONE',  ( 2.888995153171149077, 156.0927491134738716, 0.02440385714215731819 ) ) ;
#32132 = ORIENTED_EDGE ( 'NONE', *, *, #9989, .T. ) ;
#32133 = CARTESIAN_POINT ( 'NONE',  ( 19.73710541150934006, 148.2167131080949787, 2.515028838702476399 ) ) ;
#32134 = FACE_OUTER_BOUND ( 'NONE', #17961, .T. ) ;
#32135 = CARTESIAN_POINT ( 'NONE',  ( 0.03519895179119666290, 115.7029491485446613, -1.761499482103947800 ) ) ;
#32136 = CARTESIAN_POINT ( 'NONE',  ( -16.34457059127857192, 122.7783120765077030, 0.5554794724330636146 ) ) ;
#32137 = CARTESIAN_POINT ( 'NONE',  ( 5.008145846585815519, 117.3993852234726916, -0.7758522831737841852 ) ) ;
#32138 = AXIS2_PLACEMENT_3D ( 'NONE', #21580, #37583, #28207 ) ;
#32139 = CARTESIAN_POINT ( 'NONE',  ( 22.51579307796273000, 137.1624432810789358, 0.01304004454942963957 ) ) ;
#32140 =( BOUNDED_CURVE ( )  B_SPLINE_CURVE ( 3, ( #39430, #19809, #38794, #26638 ),
 .UNSPECIFIED., .F., .T. ) 
 B_SPLINE_CURVE_WITH_KNOTS ( ( 4, 4 ),
 ( 1.570796326794896558, 3.141592653589793116 ),
 .UNSPECIFIED. ) 
 CURVE ( )  GEOMETRIC_REPRESENTATION_ITEM ( )  RATIONAL_B_SPLINE_CURVE ( ( 1.000000000000000000, 0.8047378541243649375, 0.8047378541243649375, 1.000000000000000000 ) ) 
 REPRESENTATION_ITEM ( '' )  );
#32141 = CARTESIAN_POINT ( 'NONE',  ( -5.166338518188872797, 115.7029491485453576, -1.236684454698984803 ) ) ;
#32142 = CARTESIAN_POINT ( 'NONE',  ( -52.53071462815427850, 11.66508355409500908, 4.037383736418494351 ) ) ;
#32143 = CARTESIAN_POINT ( 'NONE',  ( -46.68395179480138779, 26.03198510454123848, 1.523999999999990695 ) ) ;
#32144 = CARTESIAN_POINT ( 'NONE',  ( -4.757346425016632629, 117.3993836136054227, -1.207075064339077963 ) ) ;
#32145 = CARTESIAN_POINT ( 'NONE',  ( -46.68395179480138779, 26.03198510454123848, 1.523999999999991140 ) ) ;
#32146 = CARTESIAN_POINT ( 'NONE',  ( -58.66687843194859653, -0.3140260920009522727, 0.3203103694181388961 ) ) ;
#32147 = CARTESIAN_POINT ( 'NONE',  ( -4.590336119847570728, 118.0156493547208498, 0.6988070414943094999 ) ) ;
#32148 = ADVANCED_FACE ( 'NONE', ( #4269 ), #26246, .T. ) ;
#32149 = ORIENTED_EDGE ( 'NONE', *, *, #6882, .T. ) ;
#32150 = ORIENTED_EDGE ( 'NONE', *, *, #34923, .T. ) ;
#32151 = CARTESIAN_POINT ( 'NONE',  ( -17.14499999999999957, 71.11999999999999034, 5.016499999999999737 ) ) ;
#32152 = CARTESIAN_POINT ( 'NONE',  ( -3.332875914431231212, 118.5088515392226469, -0.9208157437338316820 ) ) ;
#32153 = CARTESIAN_POINT ( 'NONE',  ( -7.253313547007707029, 123.0461458356614628, -0.2138788351844317370 ) ) ;
#32154 = CARTESIAN_POINT ( 'NONE',  ( 4.641283449628422986, 117.8847305990883712, 1.004414769134842622 ) ) ;
#32155 = CARTESIAN_POINT ( 'NONE',  ( 3.092642723064080279, -14.67800799544728285, 3.675123631970977911 ) ) ;
#32156 = CARTESIAN_POINT ( 'NONE',  ( -6.495892026627714699, 121.2869106855140018, -0.7936256953933332747 ) ) ;
#32157 = VECTOR ( 'NONE', #27908, 1000.000000000000227 ) ;
#32158 = CARTESIAN_POINT ( 'NONE',  ( -3.600781874455683429, 115.7029491485453576, -1.622423596436841642 ) ) ;
#32159 = CARTESIAN_POINT ( 'NONE',  ( 10.92199999999999704, 57.14999999999999858, 4.381499999999999950 ) ) ;
#32160 = LINE ( 'NONE', #35782, #13090 ) ;
#32161 = CARTESIAN_POINT ( 'NONE',  ( 4.033305401784356370, 109.8300753404742096, -3.515372713824419737 ) ) ;
#32162 = CARTESIAN_POINT ( 'NONE',  ( -13.52836484031764286, 128.5255724691869830, -1.838026323690954200 ) ) ;
#32163 = CARTESIAN_POINT ( 'NONE',  ( -6.229205138088443228, 29.61971902930247325, 1.795445774805027428 ) ) ;
#32164 = CARTESIAN_POINT ( 'NONE',  ( 5.817719362921480730, 56.51499999999997925, -4.384519708708640273 ) ) ;
#32165 = CARTESIAN_POINT ( 'NONE',  ( 3.315635589170361275, -10.27688868798473543, -3.234826238065520609 ) ) ;
#32167 = EDGE_LOOP ( 'NONE', ( #14669, #30187, #16347, #2779 ) ) ;
#32166 = CARTESIAN_POINT ( 'NONE',  ( 22.32005725002918339, 150.7328461917231550, 1.166919501784766666 ) ) ;
#32168 = CARTESIAN_POINT ( 'NONE',  ( 3.161960256423347992, 104.6144662015368709, -4.310165282358256356 ) ) ;
#32169 = CARTESIAN_POINT ( 'NONE',  ( 3.790367410748021637, -15.17722879538144198, -0.1767333597861489025 ) ) ;
#32170 = CARTESIAN_POINT ( 'NONE',  ( -6.722174884994048583, 119.4737997143703012, 1.022258653430868192 ) ) ;
#32171 = CARTESIAN_POINT ( 'NONE',  ( 0.3859925973045487679, 4.674766832570296238, -0.8944012262243137279 ) ) ;
#32172 = AXIS2_PLACEMENT_3D ( 'NONE', #4456, #30620, #26804 ) ;
#32173 = EDGE_CURVE ( 'NONE', #1003, #1503, #11055, .T. ) ;
#32174 = CARTESIAN_POINT ( 'NONE',  ( 0.9436028068379492817, -1.428137797730904879, 0.2459283266283248115 ) ) ;
#32175 = ORIENTED_EDGE ( 'NONE', *, *, #33529, .F. ) ;
#32176 = VECTOR ( 'NONE', #26000, 1000.000000000000227 ) ;
#32177 = EDGE_CURVE ( 'NONE', #22529, #21064, #14654, .T. ) ;
#32178 = ORIENTED_EDGE ( 'NONE', *, *, #3012, .F. ) ;
#32179 = CARTESIAN_POINT ( 'NONE',  ( -41.05189575270515689, 23.09451173561988924, 0.6632222222222170505 ) ) ;
#32180 = CARTESIAN_POINT ( 'NONE',  ( 2.027571083617039971, 109.8863472468248119, 3.714074494666526949 ) ) ;
#32181 = DIRECTION ( 'NONE',  ( 0.000000000000000000, 0.000000000000000000, 1.000000000000000000 ) ) ;
#32182 = CARTESIAN_POINT ( 'NONE',  ( -16.17714305270736830, 147.4171829256358137, 0.7878123557203799976 ) ) ;
#32183 = DIRECTION ( 'NONE',  ( 0.000000000000000000, 1.000000000000000000, 0.000000000000000000 ) ) ;
#32184 = CARTESIAN_POINT ( 'NONE',  ( 3.919216764667305064, -12.20455369412110080, 1.363517133079271026 ) ) ;
#32185 = CARTESIAN_POINT ( 'NONE',  ( 11.30191013352078677, 123.2561760277034324, -1.170227508207775102 ) ) ;
#32186 = CARTESIAN_POINT ( 'NONE',  ( 0.03212618750946916180, 158.2819368290249713, -1.607725792532325393 ) ) ;
#32187 = CARTESIAN_POINT ( 'NONE',  ( -33.20758249455312239, 49.81222039523557044, -1.270000000000005569 ) ) ;
#32188 = CARTESIAN_POINT ( 'NONE',  ( 8.464818653216008570, 119.1964225064569263, 1.333813180544818344 ) ) ;
#32189 = CARTESIAN_POINT ( 'NONE',  ( -4.138655142084676442, 33.37459457963606724, 1.694288919380972924 ) ) ;
#32190 = CARTESIAN_POINT ( 'NONE',  ( 15.34424630368610032, 148.0267799683202554, -0.1426181633603110233 ) ) ;
#32191 = EDGE_LOOP ( 'NONE', ( #32052, #2890, #8667, #41724 ) ) ;
#32192 = DIRECTION ( 'NONE',  ( -1.000000000000000000, 0.000000000000000000, 0.000000000000000000 ) ) ;
#32193 = CIRCLE ( 'NONE', #4333, 0.6350000000000001199 ) ;
#32194 = CARTESIAN_POINT ( 'NONE',  ( -3.932819197772147390, 27.98301002373794333, 0.4898618918306563708 ) ) ;
#32195 = CIRCLE ( 'NONE', #1593, 9.048749999999998295 ) ;
#32196 = DIRECTION ( 'NONE',  ( 0.000000000000000000, 0.000000000000000000, -1.000000000000000000 ) ) ;
#32197 = CARTESIAN_POINT ( 'NONE',  ( 16.19371004148908710, 147.7868695473139553, 1.594401216537396637 ) ) ;
#32198 = CARTESIAN_POINT ( 'NONE',  ( 4.756911902486301358, 117.3993836135862949, 1.207145067066230038 ) ) ;
#32199 = CARTESIAN_POINT ( 'NONE',  ( 22.83585328881709131, 150.4073064562084880, 0.3794817294851796086 ) ) ;
#32200 = CARTESIAN_POINT ( 'NONE',  ( -6.109903564962424483, 119.5248422734510427, 0.2725184514339176189 ) ) ;
#32201 = VECTOR ( 'NONE', #34654, 1000.000000000000000 ) ;
#32202 = CARTESIAN_POINT ( 'NONE',  ( -0.1363197777916403119, 115.6909491485452435, 1.761379840720195711 ) ) ;
#32203 = CARTESIAN_POINT ( 'NONE',  ( -32.51099854767154085, 68.28336360077705081, 1.523999999999991140 ) ) ;
#32204 = CARTESIAN_POINT ( 'NONE',  ( -5.095652749712312080, 31.83908346630384756, 0.3959475160674750249 ) ) ;
#32205 = CARTESIAN_POINT ( 'NONE',  ( 20.68324476251063615, 149.5879773183856685, 2.343194491808722191 ) ) ;
#32206 = CARTESIAN_POINT ( 'NONE',  ( -4.384008014420753163, 17.61986127277741332, -1.463615122064717111 ) ) ;
#32207 = CARTESIAN_POINT ( 'NONE',  ( 3.492884981554987611, 28.57741388400067706, -7.667201904029750992 ) ) ;
#32208 = CARTESIAN_POINT ( 'NONE',  ( -2.161519886931281942, 116.7289984965020864, -0.4898792010161093780 ) ) ;
#32209 = CARTESIAN_POINT ( 'NONE',  ( 0.08519874065837408639, 108.5751225745497948, -4.263693374914160117 ) ) ;
#32210 = CARTESIAN_POINT ( 'NONE',  ( -23.11127252101368867, 149.9001116002701224, -0.4618182267416073850 ) ) ;
#32211 = CARTESIAN_POINT ( 'NONE',  ( 3.691922595743098334, 109.5877055502880495, -3.633197977425771441 ) ) ;
#32212 = CARTESIAN_POINT ( 'NONE',  ( 2.761911675679841860, 104.6144662015501012, 4.566626345672048615 ) ) ;
#32213 = CARTESIAN_POINT ( 'NONE',  ( -3.130497002865707312, 23.39511390029671745, 3.426874451367011520 ) ) ;
#32214 = CYLINDRICAL_SURFACE ( 'NONE', #24585, 9.048749999999998295 ) ;
#32215 = CARTESIAN_POINT ( 'NONE',  ( -26.01970228765382132, 72.88622078690372064, 1.269999999999992468 ) ) ;
#32216 = CARTESIAN_POINT ( 'NONE',  ( 3.211984996733021624, -14.06435921420946755, 2.432701253525752172 ) ) ;
#32217 = CARTESIAN_POINT ( 'NONE',  ( 0.3374525697214812436, 106.5118632461160217, -5.070939582669566903 ) ) ;
#32218 = CARTESIAN_POINT ( 'NONE',  ( -14.33434017258165127, 120.4308286971427862, 0.3827902340739950393 ) ) ;
#32219 = ORIENTED_EDGE ( 'NONE', *, *, #15810, .F. ) ;
#32220 = CARTESIAN_POINT ( 'NONE',  ( 6.059261036834384662, 88.73331249999999670, 5.016499999999999737 ) ) ;
#32221 = ADVANCED_FACE ( 'NONE', ( #33233 ), #10841, .T. ) ;
#32222 = VERTEX_POINT ( 'NONE', #4061 ) ;
#32223 = CARTESIAN_POINT ( 'NONE',  ( -42.18235783619700641, 22.15054559413666624, -1.778153187291473758 ) ) ;
#32224 = CIRCLE ( 'NONE', #40419, 0.2539999999999998925 ) ;
#32225 = CARTESIAN_POINT ( 'NONE',  ( 4.774069126156925691, -15.45330506282495442, 3.807469687449487772 ) ) ;
#32226 = CARTESIAN_POINT ( 'NONE',  ( -17.07772634048058791, 128.5677977248401476, 1.430458439683571115 ) ) ;
#32227 = CARTESIAN_POINT ( 'NONE',  ( 11.01560508856915099, 119.3804150619309468, -0.7804404673305008755 ) ) ;
#32228 = ADVANCED_FACE ( 'NONE', ( #24246 ), #17020, .T. ) ;
#32229 = CARTESIAN_POINT ( 'NONE',  ( -1.576536484031922480, 10.66345178295009788, -4.350723848753511369 ) ) ;
#32230 = CARTESIAN_POINT ( 'NONE',  ( -58.04839436022131594, 0.9580029038198520919, -1.310276026340456479 ) ) ;
#32231 = ORIENTED_EDGE ( 'NONE', *, *, #30489, .F. ) ;
#32232 = CARTESIAN_POINT ( 'NONE',  ( -58.16644339752609483, 0.1874380212898556775, -0.9010643026010315415 ) ) ;
#32233 = CARTESIAN_POINT ( 'NONE',  ( -0.009645608633146510874, 120.9711055683165597, 0.4827056984855356836 ) ) ;
#32234 = CARTESIAN_POINT ( 'NONE',  ( -17.58003597271454765, 146.9817191466759141, 1.463309413676198378 ) ) ;
#32235 = CARTESIAN_POINT ( 'NONE',  ( -3.590474171207809651E-14, 56.51499999999999346, 0.000000000000000000 ) ) ;
#32236 = CARTESIAN_POINT ( 'NONE',  ( 3.344131534676130890, 119.2933411826354728, -0.7437009012386069928 ) ) ;
#32237 = CARTESIAN_POINT ( 'NONE',  ( -11.72614449088027833, 156.4111399680655552, -2.003450915338490734 ) ) ;
#32238 = CARTESIAN_POINT ( 'NONE',  ( -58.83227707057486811, -0.08366279997995551554, -1.273395421382134774E-15 ) ) ;
#32239 = AXIS2_PLACEMENT_3D ( 'NONE', #7899, #4298, #40494 ) ;
#32240 = VERTEX_POINT ( 'NONE', #23613 ) ;
#32241 = CARTESIAN_POINT ( 'NONE',  ( 4.503783518555258603, 118.1168598955523663, -0.5561582125388926379 ) ) ;
#32242 = CARTESIAN_POINT ( 'NONE',  ( 15.60301224545398036, 143.6313904367523833, -0.5515178422673748804 ) ) ;
#32243 = ORIENTED_EDGE ( 'NONE', *, *, #29820, .T. ) ;
#32244 = CARTESIAN_POINT ( 'NONE',  ( 0.02768739821002592222, 156.9833357668885014, -1.385590625008458643 ) ) ;
#32245 = CARTESIAN_POINT ( 'NONE',  ( 3.347262984424072219, -14.85936863781750539, 0.1546827838429291613 ) ) ;
#32246 = VECTOR ( 'NONE', #7537, 1000.000000000000000 ) ;
#32247 = DIRECTION ( 'NONE',  ( 4.017660918040594346E-17, -1.000000000000000000, -2.376309959284834438E-19 ) ) ;
#32248 = CARTESIAN_POINT ( 'NONE',  ( -57.34787435976332404, 1.552391619547691004, -1.028525222821079960E-14 ) ) ;
#32249 = CARTESIAN_POINT ( 'NONE',  ( -4.833894161298425196, 117.7366906883232218, 0.8571493831372747341 ) ) ;
#32250 = CARTESIAN_POINT ( 'NONE',  ( 2.540463897194693121, 119.9929590031203901, 0.6352340916430190276 ) ) ;
#32251 = CARTESIAN_POINT ( 'NONE',  ( 2.711364258112229031, 37.31625399494021877, -1.095520810760639341 ) ) ;
#32252 = AXIS2_PLACEMENT_3D ( 'NONE', #22371, #23209, #6224 ) ;
#32253 = CARTESIAN_POINT ( 'NONE',  ( -4.191205975170537279, 21.45845178295031630, -1.961646697876042511 ) ) ;
#32254 = CARTESIAN_POINT ( 'NONE',  ( 9.348637138742738273, 124.2740283646700306, 0.4211050520620436832 ) ) ;
#32255 = DIRECTION ( 'NONE',  ( 6.353134868986659519E-16, -1.000000000000000000, 0.000000000000000000 ) ) ;
#32257 = EDGE_LOOP ( 'NONE', ( #30658, #9565, #187, #17736 ) ) ;
#32256 = CARTESIAN_POINT ( 'NONE',  ( -47.25474348537468927, 18.41641806589853303, -3.087470713317427506 ) ) ;
#32258 = CARTESIAN_POINT ( 'NONE',  ( -0.8127763598983991367, 118.1588900138767997, 0.8680101205736402425 ) ) ;
#32259 = CARTESIAN_POINT ( 'NONE',  ( -48.20156657701304681, 19.76063879377972654, 5.201425424509390716 ) ) ;
#32260 = CARTESIAN_POINT ( 'NONE',  ( -49.26208180856533403, 17.44698433589570641, 5.073594244243587958 ) ) ;
#32261 = FACE_OUTER_BOUND ( 'NONE', #36180, .T. ) ;
#32262 = DIRECTION ( 'NONE',  ( -9.627370216492862708E-17, -1.000000000000000000, 0.000000000000000000 ) ) ;
#32263 = CARTESIAN_POINT ( 'NONE',  ( -56.26154134543016738, 7.775270144418325202, 0.1976385065555384957 ) ) ;
#32264 = CARTESIAN_POINT ( 'NONE',  ( -1.415223785869884399, 159.6020224343070026, 0.1017758242917467665 ) ) ;
#32265 = EDGE_LOOP ( 'NONE', ( #28256, #35812 ) ) ;
#32266 = CARTESIAN_POINT ( 'NONE',  ( -54.50298212578950796, 9.515077312548310573, -3.630897911711918002 ) ) ;
#32267 = CARTESIAN_POINT ( 'NONE',  ( -7.822086219072885704, 122.4005678741224443, -0.6184629442691977896 ) ) ;
#32268 = ORIENTED_EDGE ( 'NONE', *, *, #32458, .F. ) ;
#32269 = CARTESIAN_POINT ( 'NONE',  ( 2.054978793759712818, 115.7029326100966671, -1.635623593644852658 ) ) ;
#32270 = CARTESIAN_POINT ( 'NONE',  ( -15.78746250177974808, 146.2429432508320417, -0.4439881280938304808 ) ) ;
#32271 = CARTESIAN_POINT ( 'NONE',  ( 4.721559244837001401, -14.40436002768456802, 4.408607674763740825 ) ) ;
#32272 = CARTESIAN_POINT ( 'NONE',  ( -10.67497907003079050, 119.8050749133877275, 0.9899969268117744248 ) ) ;
#32273 = CARTESIAN_POINT ( 'NONE',  ( 3.174366308151880922, 104.6144662015457243, 0.06343139340882769650 ) ) ;
#32274 = CARTESIAN_POINT ( 'NONE',  ( 3.280774808777962903, 159.4678586119998442, 0.2050961497903014685 ) ) ;
#32275 = CARTESIAN_POINT ( 'NONE',  ( 9.092361046020325688, 153.9681463960921803, 0.2977057961392346463 ) ) ;
#32276 = CARTESIAN_POINT ( 'NONE',  ( 5.205984836500144652, 115.6909491485453145, -1.025315722821639408 ) ) ;
#32277 = CARTESIAN_POINT ( 'NONE',  ( -0.7871466699833823411, 12.39035052102135914, -0.5757299225971378442 ) ) ;
#32278 = CARTESIAN_POINT ( 'NONE',  ( -18.76446887325688806, 125.2887878443791294, -0.4910110098351362362 ) ) ;
#32279 = DIRECTION ( 'NONE',  ( 5.188838149069472160E-16, -1.699382548006136559E-16, -1.000000000000000000 ) ) ;
#32280 = EDGE_CURVE ( 'NONE', #30579, #38903, #37850, .T. ) ;
#32281 = DIRECTION ( 'NONE',  ( -0.8745520943968162486, 0.4849315768086691625, -5.424246918827962036E-16 ) ) ;
#32282 = VERTEX_POINT ( 'NONE', #41298 ) ;
#32283 = CARTESIAN_POINT ( 'NONE',  ( -2.346178836033175230, 116.4819223308117984, 0.2686778099839046696 ) ) ;
#32284 = ORIENTED_EDGE ( 'NONE', *, *, #12352, .F. ) ;
#32285 = CARTESIAN_POINT ( 'NONE',  ( -58.36986766252679359, -0.2916724680131291825, -0.008878031541896621096 ) ) ;
#32286 = CARTESIAN_POINT ( 'NONE',  ( -0.02399864187743109417, 159.1630378086529731, 1.200990174154242363 ) ) ;
#32287 = CARTESIAN_POINT ( 'NONE',  ( 18.54838064703195499, 135.7714211226372640, -1.677382267734012666 ) ) ;
#32288 = CARTESIAN_POINT ( 'NONE',  ( -8.422295717417405569, 8.547183656736235591, -0.3195422701574849311 ) ) ;
#32289 = CARTESIAN_POINT ( 'NONE',  ( -12.43751437118963743, 120.3283006479967128, -1.391730434942824557 ) ) ;
#32290 = CARTESIAN_POINT ( 'NONE',  ( 4.847166225461900346, 117.7641644975736739, -0.8119836883907423086 ) ) ;
#32291 = CARTESIAN_POINT ( 'NONE',  ( 1.381059818124765526, 106.2379067940291293, 5.172899357470507553 ) ) ;
#32292 = CARTESIAN_POINT ( 'NONE',  ( -9.076946558997759595, 124.0722828908287454, -0.1472919029216549491 ) ) ;
#32293 = CARTESIAN_POINT ( 'NONE',  ( -18.92921826512576899, 147.2511928822236769, -2.484298966539742359 ) ) ;
#32294 = CARTESIAN_POINT ( 'NONE',  ( 5.416639188517969217, -15.16156180871851333, 2.817365454923381307 ) ) ;
#32295 = CARTESIAN_POINT ( 'NONE',  ( 1.172031118611134874E-15, 12.17394877578616885, 0.000000000000000000 ) ) ;
#32296 = CARTESIAN_POINT ( 'NONE',  ( -47.67648637180143822, 19.71513033058998232, -5.327979952964785326 ) ) ;
#32297 = VERTEX_POINT ( 'NONE', #2540 ) ;
#32298 = CARTESIAN_POINT ( 'NONE',  ( 16.28588378367221168, 151.0861551944122141, 2.361334407247334788 ) ) ;
#32299 = CARTESIAN_POINT ( 'NONE',  ( 1.231754723633442730E-15, 12.17394877578617063, 0.000000000000000000 ) ) ;
#32300 = LINE ( 'NONE', #31881, #37519 ) ;
#32301 = CARTESIAN_POINT ( 'NONE',  ( -3.181806805318239562, 118.0279923103727242, 0.7725587567394768262 ) ) ;
#32302 = CARTESIAN_POINT ( 'NONE',  ( -6.940074030747619638, 22.95585651114365788, 4.785772612677765991 ) ) ;
#32303 = CARTESIAN_POINT ( 'NONE',  ( 6.262986112992323662, 155.3815620563194955, 0.9009107504210208672 ) ) ;
#32304 = CARTESIAN_POINT ( 'NONE',  ( 22.69192130277340880, 142.3612397021088611, -0.6360799666370218208 ) ) ;
#32305 = DIRECTION ( 'NONE',  ( -5.188838149069471174E-16, 1.699382548006136313E-16, 1.000000000000000000 ) ) ;
#32306 = LINE ( 'NONE', #41911, #35855 ) ;
#32307 = EDGE_CURVE ( 'NONE', #25039, #30173, #19834, .T. ) ;
#32308 = CARTESIAN_POINT ( 'NONE',  ( -5.757472737270721730, 159.1136035536173097, -0.1150480073142621795 ) ) ;
#32309 = EDGE_LOOP ( 'NONE', ( #35303, #11102, #26500, #20448 ) ) ;
#32310 = CARTESIAN_POINT ( 'NONE',  ( -8.104605239258354743, 120.9518455590310566, -1.347037562020136470 ) ) ;
#32311 = CARTESIAN_POINT ( 'NONE',  ( -6.603988835907287056E-14, 91.53346620154573543, -3.493462572467304738E-18 ) ) ;
#32312 = CARTESIAN_POINT ( 'NONE',  ( -15.91353055065151345, 146.3070982487133165, -0.9133378546330939152 ) ) ;
#32313 = CARTESIAN_POINT ( 'NONE',  ( 2.381342306750187099, -14.83133394530772264, 5.477793184119461145 ) ) ;
#32314 = CARTESIAN_POINT ( 'NONE',  ( 6.059261036834405978, 56.81853847168531502, -4.948064083792231393 ) ) ;
#32315 = CARTESIAN_POINT ( 'NONE',  ( 5.757472737270592944, 159.1136035536173097, 0.1150480073142623738 ) ) ;
#32316 = EDGE_CURVE ( 'NONE', #31392, #15637, #34817, .T. ) ;
#32317 = ORIENTED_EDGE ( 'NONE', *, *, #19110, .T. ) ;
#32318 = CARTESIAN_POINT ( 'NONE',  ( -4.492784857928645792, 12.16275517495587977, -1.104450737933446725 ) ) ;
#32319 = CARTESIAN_POINT ( 'NONE',  ( -1.794468298957929475, 116.4672891243423578, -0.03585774721038168661 ) ) ;
#32320 = DIRECTION ( 'NONE',  ( -0.1906721105965039909, 0.9816537812491094028, -2.657572025465702696E-16 ) ) ;
#32321 = CARTESIAN_POINT ( 'NONE',  ( -17.14500000000466784, 71.11999999999886768, 1.523999999999998689 ) ) ;
#32322 = LINE ( 'NONE', #2536, #39217 ) ;
#32323 = CARTESIAN_POINT ( 'NONE',  ( -7.021952432075939221, 121.4379088036047563, 0.5782915293065207241 ) ) ;
#32324 = CARTESIAN_POINT ( 'NONE',  ( 4.627658001546194555, 13.29687521248714610, 0.05192310334374634212 ) ) ;
#32325 = CARTESIAN_POINT ( 'NONE',  ( 5.450899203173912966, 159.0107326448372191, 0.9576670044529983494 ) ) ;
#32326 = CARTESIAN_POINT ( 'NONE',  ( 15.77133435453283461, 146.5691041611200660, 0.3151487940933137555 ) ) ;
#32328 = CARTESIAN_POINT ( 'NONE',  ( 6.811759424595715373, 118.6475953829349379, -0.9158128249201541449 ) ) ;
#32327 = CARTESIAN_POINT ( 'NONE',  ( 5.224239059777379346, 56.51499999999816737, 5.327449085207758728 ) ) ;
#32329 = CARTESIAN_POINT ( 'NONE',  ( 2.245307460665866728, 11.68515688572553479, 4.070821060848484940 ) ) ;
#32330 = CARTESIAN_POINT ( 'NONE',  ( -22.49588706318651532, 149.6594668941642681, -1.627141970658571690 ) ) ;
#32331 = ORIENTED_EDGE ( 'NONE', *, *, #40180, .F. ) ;
#32332 = EDGE_CURVE ( 'NONE', #14467, #6398, #40179, .T. ) ;
#32333 = CARTESIAN_POINT ( 'NONE',  ( -0.6320890182444199867, 120.8998192842950488, 0.1133706938477904158 ) ) ;
#32334 = CARTESIAN_POINT ( 'NONE',  ( 5.507117158935161072, -13.70471586423162336, 3.054220594615255191 ) ) ;
#32335 = CARTESIAN_POINT ( 'NONE',  ( -5.008697454415233175, 117.3984623471881292, 0.7756180019310896512 ) ) ;
#32337 = ORIENTED_EDGE ( 'NONE', *, *, #8984, .T. ) ;
#32336 = AXIS2_PLACEMENT_3D ( 'NONE', #16160, #9578, #15957 ) ;
#32338 = EDGE_CURVE ( 'NONE', #1116, #38737, #36095, .T. ) ;
#32339 = CARTESIAN_POINT ( 'NONE',  ( 5.838901281334536897, 119.0696708348911699, 1.193623469369259116 ) ) ;
#32340 = FACE_OUTER_BOUND ( 'NONE', #36446, .T. ) ;
#32341 = DIRECTION ( 'NONE',  ( -4.017660918040594346E-17, 1.000000000000000000, 2.376309959284834438E-19 ) ) ;
#32342 = CARTESIAN_POINT ( 'NONE',  ( -15.42041356977108535, 121.5363848317736739, 0.5399810379570649799 ) ) ;
#32343 = ADVANCED_FACE ( 'NONE', ( #15501 ), #2773, .T. ) ;
#32344 = CARTESIAN_POINT ( 'NONE',  ( 0.002459394112954048622, 156.3065584682211124, -0.1230781383047672012 ) ) ;
#32345 = CARTESIAN_POINT ( 'NONE',  ( 16.72896750809238853, 155.2649736186859570, -0.2017331744915135117 ) ) ;
#32346 = CARTESIAN_POINT ( 'NONE',  ( -6.059261036834472591, 56.51499999999997925, -4.381499999999997286 ) ) ;
#32347 = CARTESIAN_POINT ( 'NONE',  ( -48.84023001699601707, 18.03124979360562463, 5.100068162039153918 ) ) ;
#32348 = CARTESIAN_POINT ( 'NONE',  ( -46.60530155212503445, 26.17382724835477958, 1.523999999999990917 ) ) ;
#32349 = CARTESIAN_POINT ( 'NONE',  ( -4.962828339513733589, 117.4036766243672076, -1.029743607666975036 ) ) ;
#32350 = EDGE_CURVE ( 'NONE', #18118, #4948, #2110, .T. ) ;
#32351 = VERTEX_POINT ( 'NONE', #5735 ) ;
#32352 = CARTESIAN_POINT ( 'NONE',  ( -47.07934102874904170, 22.98505637820369429, 3.579966862081928713 ) ) ;
#32353 = CYLINDRICAL_SURFACE ( 'NONE', #12505, 3.175000000000001155 ) ;
#32354 = CARTESIAN_POINT ( 'NONE',  ( -4.554716542840457016, 118.0727055014217939, 0.6229934779673420575 ) ) ;
#32355 = FACE_OUTER_BOUND ( 'NONE', #17179, .T. ) ;
#32356 = B_SPLINE_SURFACE_WITH_KNOTS ( 'NONE', 5, 3, ( 
 ( #5870, #31837, #28851, #25651 ),
 ( #6282, #2467, #15429, #6077 ),
 ( #19253, #28218, #8626, #15634 ),
 ( #28639, #38449, #12458, #12026 ),
 ( #41650, #32045, #2882, #25452 ),
 ( #25018, #41864, #9265, #22224 ),
 ( #38020, #21589, #8841, #29054 ),
 ( #38239, #21804, #18622, #25235 ) ),
 .UNSPECIFIED., .F., .F., .F.,
 ( 6, 2, 6 ),
 ( 4, 4 ),
 ( 0.000000000000000000, 0.5000000000000000000, 1.000000000000000000 ),
 ( -0.002373312499999995218, 0.03277393749999999578 ),
 .UNSPECIFIED. ) ;
#32357 = ORIENTED_EDGE ( 'NONE', *, *, #16771, .F. ) ;
#32358 = CARTESIAN_POINT ( 'NONE',  ( -0.7583562475726235430, 118.7629491485454025, -1.270948893816612690 ) ) ;
#32359 = CARTESIAN_POINT ( 'NONE',  ( -8.356341240008237747, 119.7161836924744023, -1.429665635506445653 ) ) ;
#32360 = CARTESIAN_POINT ( 'NONE',  ( -5.246142718657168302, 116.7267603939287426, -1.018146482794727525 ) ) ;
#32361 = CARTESIAN_POINT ( 'NONE',  ( 4.716113435506099627, 117.7575315690381927, 1.081390950261145623 ) ) ;
#32362 = CARTESIAN_POINT ( 'NONE',  ( 2.931439949929583122, -14.82325452411255640, 4.117531814738872420 ) ) ;
#32363 = CARTESIAN_POINT ( 'NONE',  ( -10.11490785437018403, 123.9924233945428682, -1.115122180374877869 ) ) ;
#32364 = CARTESIAN_POINT ( 'NONE',  ( -2.094230385292464192, 115.7021042694705955, -1.712899454762304430 ) ) ;
#32365 = DIRECTION ( 'NONE',  ( -1.000000000000000000, 0.000000000000000000, 0.000000000000000000 ) ) ;
#32366 = CARTESIAN_POINT ( 'NONE',  ( -23.16987411132078023, 77.52691185402750307, -1.524000000000004906 ) ) ;
#32367 = CARTESIAN_POINT ( 'NONE',  ( 6.897523911741961555, 121.8252198949890186, -0.01845719934638743662 ) ) ;
#32368 = CARTESIAN_POINT ( 'NONE',  ( -16.94675455810626374, 147.0740084267719396, -1.925552282123431214 ) ) ;
#32369 = CARTESIAN_POINT ( 'NONE',  ( -0.03245814172817904769, 157.7902383798253538, 1.624338139048501883 ) ) ;
#32370 = AXIS2_PLACEMENT_3D ( 'NONE', #26776, #16755, #13981 ) ;
#32371 = FACE_OUTER_BOUND ( 'NONE', #1430, .T. ) ;
#32372 = CARTESIAN_POINT ( 'NONE',  ( 3.064284189169764971, -3.155149710853871525, 3.465721614369133174 ) ) ;
#32374 = ORIENTED_EDGE ( 'NONE', *, *, #38050, .T. ) ;
#32373 = CARTESIAN_POINT ( 'NONE',  ( 15.17352684163996734, 120.8830733721255370, 0.9063557954379340975 ) ) ;
#32375 = DIRECTION ( 'NONE',  ( -6.353134868986659519E-16, 1.000000000000000000, 0.000000000000000000 ) ) ;
#32376 = CARTESIAN_POINT ( 'NONE',  ( 3.819321967970790599, -15.20641387874817418, 0.06971680219106241028 ) ) ;
#32377 = CARTESIAN_POINT ( 'NONE',  ( -15.17663987144310056, 128.5586215118215705, 1.546218023206676229 ) ) ;
#32378 = CARTESIAN_POINT ( 'NONE',  ( 0.6656887758738300187, 13.74536131906779879, -0.7131539583378491143 ) ) ;
#32379 = CARTESIAN_POINT ( 'NONE',  ( -2.795228999030447969, 116.6385632091030544, -0.2515850966972202896 ) ) ;
#32380 = CARTESIAN_POINT ( 'NONE',  ( 0.8411255309083253140, 9.366862202269544468, -0.4933303560167117130 ) ) ;
#32381 = ORIENTED_EDGE ( 'NONE', *, *, #7916, .T. ) ;
#32382 = ORIENTED_EDGE ( 'NONE', *, *, #40219, .F. ) ;
#32383 = CARTESIAN_POINT ( 'NONE',  ( -44.27221412529542022, 20.06621383160478445, 0.8981538560692690076 ) ) ;
#32384 = CARTESIAN_POINT ( 'NONE',  ( 4.119305931990680847, 118.0988315448752530, 0.8046943418515852819 ) ) ;
#32385 = APPLICATION_PROTOCOL_DEFINITION ( 'draft international standard', 'automotive_design', 1998, #30877 ) ;
#32386 = CARTESIAN_POINT ( 'NONE',  ( -16.52109770691750867, 146.2355833862463328, 0.9494891650916720272 ) ) ;
#32387 = CARTESIAN_POINT ( 'NONE',  ( 3.969679720280225421, -13.58737529183706627, 3.751183842293267290 ) ) ;
#32388 = CARTESIAN_POINT ( 'NONE',  ( 17.67908073340989716, 148.3509993576462307, -1.576626744559513460 ) ) ;
#32389 = CARTESIAN_POINT ( 'NONE',  ( -0.4459748878573762676, 118.5593716040226724, -0.6139719676240718016 ) ) ;
#32390 = CARTESIAN_POINT ( 'NONE',  ( -9.960492004070044203, 64.81807050032566053, 1.524000000000003352 ) ) ;
#32391 = CARTESIAN_POINT ( 'NONE',  ( 2.102813808753936087, -15.18136450426021256, 5.202461169095355942 ) ) ;
#32392 = CARTESIAN_POINT ( 'NONE',  ( -1.842030023794387406, 35.66238107416427994, 0.6533647080653418593 ) ) ;
#32393 = CARTESIAN_POINT ( 'NONE',  ( 15.85793921209435098, 146.6055793175013093, -0.1365194753024329688 ) ) ;
#32394 = ADVANCED_FACE ( 'NONE', ( #28501 ), #29974, .T. ) ;
#32395 = ORIENTED_EDGE ( 'NONE', *, *, #32611, .F. ) ;
#32396 = CARTESIAN_POINT ( 'NONE',  ( -6.616924617768071466E-14, 97.37546620154573418, 7.965525879364083286E-30 ) ) ;
#32397 =( BOUNDED_SURFACE ( )  B_SPLINE_SURFACE ( 3, 2, ( 
 ( #10871, #7065, #23859 ),
 ( #33472, #20029, #23642 ),
 ( #3878, #13862, #39864 ),
 ( #29843, #36664, #681 ),
 ( #13653, #7485, #26643 ),
 ( #4302, #14477, #37700 ),
 ( #37483, #11492, #8522 ),
 ( #18296, #8308, #24478 ),
 ( #33889, #40698, #34099 ),
 ( #24908, #27690, #31295 ) ),
 .UNSPECIFIED., .F., .F., .T. ) 
 B_SPLINE_SURFACE_WITH_KNOTS ( ( 4, 2, 2, 2, 4 ),
 ( 3, 3 ),
 ( -8.881784197001252323E-16, 0.3926990816987235844, 0.7853981633974480570, 1.178097245096172418, 1.570796326794897002 ),
 ( 0.000000000000000000, 1.000000000000000000 ),
 .UNSPECIFIED. ) 
 GEOMETRIC_REPRESENTATION_ITEM ( )  RATIONAL_B_SPLINE_SURFACE ( (
 ( 1.000000000000000000, 0.7572803591334833495, 1.000000000000000000),
 ( 1.000000000000000000, 0.7572851909592280828, 1.000000000000000000),
 ( 1.000000000000000000, 0.7560206254140621196, 1.000000000000000000),
 ( 1.000000000000000000, 0.7511365686956649190, 1.000000000000000000),
 ( 1.000000000000000000, 0.7475127447245452084, 1.000000000000000000),
 ( 1.000000000000000000, 0.7383589052087454752, 1.000000000000000000),
 ( 1.000000000000000000, 0.7328301610706697833, 1.000000000000000000),
 ( 1.000000000000000000, 0.7206031636699079534, 1.000000000000000000),
 ( 1.000000000000000000, 0.7139102541741279007, 1.000000000000000000),
 ( 1.000000000000000000, 0.7071067811865475727, 1.000000000000000000) ) ) 
 REPRESENTATION_ITEM ( '' )  SURFACE ( )  );
#32398 = DIRECTION ( 'NONE',  ( 0.9816537812491089587, 0.1906721105965065444, 4.769617732184475162E-16 ) ) ;
#32399 = CIRCLE ( 'NONE', #18794, 0.6350000000000001199 ) ;
#32400 = CARTESIAN_POINT ( 'NONE',  ( -58.68272167409660511, -0.3140646606565877796, 0.3072153925275410424 ) ) ;
#32401 = VECTOR ( 'NONE', #16465, 1000.000000000000000 ) ;
#32402 = DIRECTION ( 'NONE',  ( -0.8745520943968241312, 0.4849315768086548406, -5.691349986800536046E-16 ) ) ;
#32403 = CARTESIAN_POINT ( 'NONE',  ( 15.89375338022607664, 121.0219768425927214, 0.2124277663179633124 ) ) ;
#32404 = AXIS2_PLACEMENT_3D ( 'NONE', #40291, #27487, #34513 ) ;
#32405 = ADVANCED_FACE ( 'NONE', ( #18060 ), #8495, .T. ) ;
#32406 = CARTESIAN_POINT ( 'NONE',  ( -7.694663930960380149, 124.9344662015457317, -0.1537576976229972081 ) ) ;
#32407 = EDGE_CURVE ( 'NONE', #16319, #1811, #12280, .T. ) ;
#32408 = DIRECTION ( 'NONE',  ( -4.017660918040594346E-17, 1.000000000000000000, 2.376309959284834438E-19 ) ) ;
#32409 = CARTESIAN_POINT ( 'NONE',  ( 4.636249899789679496, -11.37698174978397958, -0.2454043791197063895 ) ) ;
#32410 = CARTESIAN_POINT ( 'NONE',  ( -3.786193870232612557, 33.00004608313867038, 1.177060218906804012 ) ) ;
#32411 = CARTESIAN_POINT ( 'NONE',  ( 13.88956208308353801, 122.0315337860429423, 1.683705570428295495 ) ) ;
#32412 = CARTESIAN_POINT ( 'NONE',  ( 0.3943543298815788134, 25.17882533764851871, -4.623353113333005915 ) ) ;
#32413 = CARTESIAN_POINT ( 'NONE',  ( 5.686328549477039473, -14.11678386645415628, -6.209864621142330954 ) ) ;
#32414 = CARTESIAN_POINT ( 'NONE',  ( 5.514681883891941361, 117.1567625688420691, -0.5563447151070903818 ) ) ;
#32415 = CARTESIAN_POINT ( 'NONE',  ( -1.969999177844983684, 122.1523088006674840, -0.2733757396980688870 ) ) ;
#32416 = DIRECTION ( 'NONE',  ( 5.188838149069472160E-16, -1.699382548006136559E-16, -1.000000000000000000 ) ) ;
#32417 = CARTESIAN_POINT ( 'NONE',  ( 0.3678577911475685025, 105.9884271946378789, -5.283348413363662566 ) ) ;
#32418 = CARTESIAN_POINT ( 'NONE',  ( 2.760961650891263552, 105.1243252582604129, 4.565018514838535602 ) ) ;
#32419 = CARTESIAN_POINT ( 'NONE',  ( -0.1328416520900886078, 24.48205809745167372, 4.627450821846854190 ) ) ;
#32420 = FACE_OUTER_BOUND ( 'NONE', #14774, .T. ) ;
#32421 = CARTESIAN_POINT ( 'NONE',  ( -1.969863483948048444, 117.3993837347434237, -1.449772854203450034 ) ) ;
#32422 = CARTESIAN_POINT ( 'NONE',  ( 3.047801963512828394, -14.61332798263154054, 3.862229702996769376 ) ) ;
#32423 = CARTESIAN_POINT ( 'NONE',  ( 2.437154581274076914, 119.8248006784163380, -0.4733635836876308178 ) ) ;
#32424 = CARTESIAN_POINT ( 'NONE',  ( -11.41934419072027573, 118.9229013597968247, 0.3849275771520425105 ) ) ;
#32425 = ORIENTED_EDGE ( 'NONE', *, *, #26363, .T. ) ;
#32426 = CARTESIAN_POINT ( 'NONE',  ( -23.62918761621517660, 82.45577215708875940, -1.524000000000006017 ) ) ;
#32427 = ORIENTED_EDGE ( 'NONE', *, *, #38572, .T. ) ;
#32428 = DIRECTION ( 'NONE',  ( -0.8745520943968005945, 0.4849315768086974732, -6.829619984160627478E-16 ) ) ;
#32429 = CARTESIAN_POINT ( 'NONE',  ( 6.125566448072323311, -14.60357603047697594, -0.1915981853098273624 ) ) ;
#32430 = CARTESIAN_POINT ( 'NONE',  ( -7.829350110466720025, 119.0983413489662297, 1.000240898550800894 ) ) ;
#32431 = CARTESIAN_POINT ( 'NONE',  ( 3.000642688540850145, 117.3922842568077698, -0.5420849065376539544 ) ) ;
#32432 = CARTESIAN_POINT ( 'NONE',  ( -2.395914033174281865, 1.367755174955888275, -3.957843245732672877 ) ) ;
#32433 = CARTESIAN_POINT ( 'NONE',  ( -58.46831931685589723, 0.04886852696691689618, -0.7470671021170768311 ) ) ;
#32434 = ORIENTED_EDGE ( 'NONE', *, *, #21007, .F. ) ;
#32435 = CARTESIAN_POINT ( 'NONE',  ( -58.58343337229877079, -0.6799398409036180313, -0.1767901212656000642 ) ) ;
#32436 = CIRCLE ( 'NONE', #5908, 5.334000000000001407 ) ;
#32437 = DIRECTION ( 'NONE',  ( -0.000000000000000000, -0.000000000000000000, -1.000000000000000000 ) ) ;
#32438 = CARTESIAN_POINT ( 'NONE',  ( -4.704233533693831681, 117.8349189730105309, 0.8529071958809373299 ) ) ;
#32439 = CARTESIAN_POINT ( 'NONE',  ( -17.39219791206841137, 147.8988302317391117, 1.461875531624039493 ) ) ;
#32440 = CARTESIAN_POINT ( 'NONE',  ( -10.75478607932181241, 82.07015292912137738, 1.524000000000000243 ) ) ;
#32441 = CARTESIAN_POINT ( 'NONE',  ( 13.69950719238972603, 125.8243951943327517, -1.418320022125399316 ) ) ;
#32442 = CARTESIAN_POINT ( 'NONE',  ( -15.86975487622011016, 125.3951846505478329, -1.921535798876653711 ) ) ;
#32443 = CARTESIAN_POINT ( 'NONE',  ( -57.66338803320029882, 2.692357263605615891, -1.869785753600856637 ) ) ;
#32444 = ORIENTED_EDGE ( 'NONE', *, *, #37802, .T. ) ;
#32445 = CARTESIAN_POINT ( 'NONE',  ( 4.536962900200297355, 118.1142359939903486, -0.5195621094609307322 ) ) ;
#32446 = CARTESIAN_POINT ( 'NONE',  ( 9.705341575047208735, 124.1466939447965814, -0.4180229424618548406 ) ) ;
#32447 = VERTEX_POINT ( 'NONE', #16335 ) ;
#32448 = CARTESIAN_POINT ( 'NONE',  ( -10.01853622893607643, 122.3915136462027817, -1.471741716425344570 ) ) ;
#32449 = CARTESIAN_POINT ( 'NONE',  ( 2.845230715667840027, -15.32736664957809403, 4.381646938852296280 ) ) ;
#32450 = CARTESIAN_POINT ( 'NONE',  ( 4.918680324695957395, 105.1215131357075450, -2.093362006766627648 ) ) ;
#32451 = AXIS2_PLACEMENT_3D ( 'NONE', #21947, #25374, #31337 ) ;
#32452 = TOROIDAL_SURFACE ( 'NONE', #5954, 0.3810000000000014486, 0.2540000000000000036 ) ;
#32453 = CARTESIAN_POINT ( 'NONE',  ( -47.93564525088164885, 15.36257551998183857, -8.154853246613427015E-15 ) ) ;
#32454 = CARTESIAN_POINT ( 'NONE',  ( -4.833313786903620013, 117.6748972090164784, 0.9053765355249284719 ) ) ;
#32455 = CARTESIAN_POINT ( 'NONE',  ( 16.32868586224174479, 149.3997711511537148, 2.122341471705227356 ) ) ;
#32456 = CARTESIAN_POINT ( 'NONE',  ( -0.01822531903872333034, 118.1564764849152738, 0.9120692297075591037 ) ) ;
#32457 = CIRCLE ( 'NONE', #8654, 3.683000000000001162 ) ;
#32458 = EDGE_CURVE ( 'NONE', #21262, #702, #29264, .T. ) ;
#32459 = CARTESIAN_POINT ( 'NONE',  ( -0.8080508600641240768, 24.25718022715097888, 4.550674767031389401 ) ) ;
#32460 = CARTESIAN_POINT ( 'NONE',  ( 15.24801397198100972, 143.4548391324710224, 0.5370776308064710847 ) ) ;
#32461 = DIRECTION ( 'NONE',  ( -0.8745520943968249084, 0.4849315768086533418, -5.271987356194193006E-16 ) ) ;
#32462 = VECTOR ( 'NONE', #9672, 1000.000000000000114 ) ;
#32463 = CARTESIAN_POINT ( 'NONE',  ( -46.36222913602039597, 19.75614878210438263, -3.583538483381434325 ) ) ;
#32464 = CARTESIAN_POINT ( 'NONE',  ( -3.222356721042568317, 117.3993833695669906, 1.271110537006335139 ) ) ;
#32465 = CARTESIAN_POINT ( 'NONE',  ( -46.96327221648714101, 24.95754849389490815, 2.007562630684373239 ) ) ;
#32466 = CARTESIAN_POINT ( 'NONE',  ( -28.74159376897886276, 60.61225341505600284, -1.270000000000005125 ) ) ;
#32467 = CARTESIAN_POINT ( 'NONE',  ( -8.795781703810718000, 117.6859433316420223, -0.2728653492683267845 ) ) ;
#32468 = CARTESIAN_POINT ( 'NONE',  ( -58.37116772670351850, -0.2940390518722524327, -2.603646672650065119E-13 ) ) ;
#32469 = CARTESIAN_POINT ( 'NONE',  ( 7.461249999999945537, 85.80437499999999318, 0.000000000000000000 ) ) ;
#32470 = CARTESIAN_POINT ( 'NONE',  ( -56.90265763162630464, 5.074588416753345044, 1.064700026618647266 ) ) ;
#32471 = CARTESIAN_POINT ( 'NONE',  ( -56.80697847991661575, 4.636179106009441497, 2.484889565616565488 ) ) ;
#32472 = CARTESIAN_POINT ( 'NONE',  ( -22.95349865178522819, 150.1476136049543868, -0.1290964995630296541 ) ) ;
#32473 = ORIENTED_EDGE ( 'NONE', *, *, #35802, .F. ) ;
#32474 = CARTESIAN_POINT ( 'NONE',  ( -51.75204694603132083, 19.49597778360960021, -0.7628839639000161155 ) ) ;
#32475 = CARTESIAN_POINT ( 'NONE',  ( -7.787039648717389184, 122.6067446965587067, -0.2565226439608999098 ) ) ;
#32476 = ORIENTED_EDGE ( 'NONE', *, *, #41215, .T. ) ;
#32477 = FACE_OUTER_BOUND ( 'NONE', #23896, .T. ) ;
#32478 = CARTESIAN_POINT ( 'NONE',  ( -15.24801397198113762, 143.4548391324710224, -0.5370776308064708626 ) ) ;
#32479 = CARTESIAN_POINT ( 'NONE',  ( 4.956269154958684808, -14.57630274377035029, 4.209183869072664841 ) ) ;
#32480 = CARTESIAN_POINT ( 'NONE',  ( -12.10120965742751409, 156.5645100661158153, 1.400626166162074915 ) ) ;
#32481 = DIRECTION ( 'NONE',  ( -5.188838149069471174E-16, 1.699382548006136313E-16, 1.000000000000000000 ) ) ;
#32482 = CARTESIAN_POINT ( 'NONE',  ( 21.86057864824936559, 151.4416708234707301, 0.7622892283599554952 ) ) ;
#32483 = COLOUR_RGB ( '', 0.72549020, 0.75294118, 0.79215686) ;
#32484 = CARTESIAN_POINT ( 'NONE',  ( 14.12992900693046217, 138.8284504506842723, 0.4149782266466619518 ) ) ;
#32485 = CARTESIAN_POINT ( 'NONE',  ( -19.64403260974359355, 72.50569198072959409, 1.269999999999996909 ) ) ;
#32486 = CARTESIAN_POINT ( 'NONE',  ( 0.6184700321857297123, 7.203955656377674543, 0.7581051976356608657 ) ) ;
#32487 = CARTESIAN_POINT ( 'NONE',  ( -15.88955207386071677, 121.0219768425927214, -0.4226783167178084222 ) ) ;
#32488 = CARTESIAN_POINT ( 'NONE',  ( -3.630816577625874595E-14, 57.14999999999999147, 0.000000000000000000 ) ) ;
#32489 = DIRECTION ( 'NONE',  ( 0.8745520943968235761, -0.4849315768086558398, 8.537024980200821818E-16 ) ) ;
#32490 = EDGE_LOOP ( 'NONE', ( #1497, #39129, #41859, #9652 ) ) ;
#32491 = CARTESIAN_POINT ( 'NONE',  ( 5.563236611437734069, 117.4964933332594939, 0.9016082036358555873 ) ) ;
#32492 = ORIENTED_EDGE ( 'NONE', *, *, #24307, .F. ) ;
#32493 = CARTESIAN_POINT ( 'NONE',  ( -58.30426395036794673, -0.1531247907950611109, -0.3258712918401721059 ) ) ;
#32494 = CARTESIAN_POINT ( 'NONE',  ( 1.092003032498458426, 117.6437429425539420, 0.5722403007656918783 ) ) ;
#32495 = CARTESIAN_POINT ( 'NONE',  ( 0.01133701039331200082, 118.4098733054621277, -0.5673503590873753000 ) ) ;
#32496 = CARTESIAN_POINT ( 'NONE',  ( -0.8194340683325834762, 6.824753112428224355, -0.5254904297167376503 ) ) ;
#32497 = CARTESIAN_POINT ( 'NONE',  ( -6.293633234193186432, 17.08131519529194975, -5.670988759835773330 ) ) ;
#32498 = CARTESIAN_POINT ( 'NONE',  ( -21.42793111275547346, 141.8478887571778273, -2.143904907781017943 ) ) ;
#32499 = CARTESIAN_POINT ( 'NONE',  ( 4.744530630439001584, 117.8975126698502294, -0.7673925427075298789 ) ) ;
#32500 = CARTESIAN_POINT ( 'NONE',  ( 5.244916502329305175, 116.2229785614576798, 1.177106425564501402 ) ) ;
#32501 = CARTESIAN_POINT ( 'NONE',  ( 0.02156534543286487207, 156.6359106937186709, -1.079218069903262300 ) ) ;
#32502 = CIRCLE ( 'NONE', #3931, 7.461249999999999716 ) ;
#32503 = CARTESIAN_POINT ( 'NONE',  ( -15.52759540040498543, 147.5317938866932366, -0.2591190040802685002 ) ) ;
#32504 = ORIENTED_EDGE ( 'NONE', *, *, #11519, .T. ) ;
#32505 = CARTESIAN_POINT ( 'NONE',  ( -18.29412156995184446, 148.6295804641074483, -2.431306780064794282 ) ) ;
#32506 = CARTESIAN_POINT ( 'NONE',  ( 4.894061823620152296, -15.42295773938226411, 3.608731902971048733 ) ) ;
#32507 = PLANE ( 'NONE',  #3657 ) ;
#32508 = CARTESIAN_POINT ( 'NONE',  ( -47.04837031381860157, 23.61299024743492581, -3.054033755318078303 ) ) ;
#32509 = ORIENTED_EDGE ( 'NONE', *, *, #7929, .T. ) ;
#32510 = CARTESIAN_POINT ( 'NONE',  ( 9.373281424700387277, 121.4347015428822374, 1.498606428831741111 ) ) ;
#32511 = CARTESIAN_POINT ( 'NONE',  ( -33.20758249455312239, 49.81222039523557044, 1.269999999999993578 ) ) ;
#32512 = CARTESIAN_POINT ( 'NONE',  ( -9.638062024671791406, 56.51499999999998636, 3.341163682266966022E-16 ) ) ;
#32513 =( GEOMETRIC_REPRESENTATION_CONTEXT ( 3 ) GLOBAL_UNCERTAINTY_ASSIGNED_CONTEXT ( ( #10359 ) ) GLOBAL_UNIT_ASSIGNED_CONTEXT ( ( #40102, #17699, #24305 ) ) REPRESENTATION_CONTEXT ( 'NONE', 'WORKASPACE' ) );
#32514 = CARTESIAN_POINT ( 'NONE',  ( -2.298002300860151781, 118.5759350612125900, 0.7369678581462183464 ) ) ;
#32515 = CARTESIAN_POINT ( 'NONE',  ( 3.492884981554987611, 28.57741388400067706, -7.667201904029750992 ) ) ;
#32516 = CARTESIAN_POINT ( 'NONE',  ( 14.53200193279634433, 139.1552669279217298, 1.026914593849031165 ) ) ;
#32517 = CARTESIAN_POINT ( 'NONE',  ( 14.83366055447111975, 120.8492938200443092, -0.4607208393402016933 ) ) ;
#32518 = DIRECTION ( 'NONE',  ( 1.011795553208986377E-16, 1.000000000000000000, -0.000000000000000000 ) ) ;
#32519 = DIRECTION ( 'NONE',  ( -0.9998004120163608288, 0.000000000000000000, -0.01997839162482749342 ) ) ;
#32520 = CARTESIAN_POINT ( 'NONE',  ( -5.775410652799862987, 116.9337168780244696, -0.1011920919882984826 ) ) ;
#32521 = ORIENTED_EDGE ( 'NONE', *, *, #28132, .F. ) ;
#32522 = CARTESIAN_POINT ( 'NONE',  ( -6.414862124821939737, 120.2136652291687113, -1.181229002280302254 ) ) ;
#32523 = CARTESIAN_POINT ( 'NONE',  ( -18.35410564743290607, 77.35382415001784295, -1.904999999999999583 ) ) ;
#32524 = CARTESIAN_POINT ( 'NONE',  ( -9.165636745952109976, 123.6526633469202920, -0.6866826908162829701 ) ) ;
#32525 = CARTESIAN_POINT ( 'NONE',  ( 4.292324012607982908, -12.68181061970326340, 2.304565294163185118 ) ) ;
#32526 = DIRECTION ( 'NONE',  ( 0.9998004120163608288, 0.000000000000000000, 0.01997839162482749342 ) ) ;
#32527 = CARTESIAN_POINT ( 'NONE',  ( 13.69515342115106904, 119.6466660129326272, 0.2899717296217781404 ) ) ;
#32528 = VERTEX_POINT ( 'NONE', #25718 ) ;
#32529 = CARTESIAN_POINT ( 'NONE',  ( -2.923568588381722844, 13.88697512809157786, 3.594856661414283394 ) ) ;
#32530 = CARTESIAN_POINT ( 'NONE',  ( 5.182655383320532216, 105.1222097428776152, 1.273793769351906802 ) ) ;
#32531 = CARTESIAN_POINT ( 'NONE',  ( -17.14500000000466784, 71.11999999999886768, -1.524000000000000909 ) ) ;
#32532 = PLANE ( 'NONE',  #1357 ) ;
#32533 = CARTESIAN_POINT ( 'NONE',  ( 7.841223576139474183, 122.2967352183207339, 0.7262958897790078305 ) ) ;
#32534 = CARTESIAN_POINT ( 'NONE',  ( -4.609865753310859127, 8.349128549105346409, -0.5081561704775721111 ) ) ;
#32535 = CARTESIAN_POINT ( 'NONE',  ( 7.599585376671099901, 158.5456267226934131, 1.164890904197547261 ) ) ;
#32536 = DIRECTION ( 'NONE',  ( 5.188838149069472160E-16, -1.699382548006136559E-16, -1.000000000000000000 ) ) ;
#32538 = CARTESIAN_POINT ( 'NONE',  ( 21.06902287100046678, 145.7918284779248665, -1.526944944257475623 ) ) ;
#32537 = CARTESIAN_POINT ( 'NONE',  ( 5.449227423685711891, 56.51499999999995794, 5.145694933557973805 ) ) ;
#32539 = CARTESIAN_POINT ( 'NONE',  ( 4.585212383536918956, 13.09695617864405470, 0.6580430208065696229 ) ) ;
#32540 = CARTESIAN_POINT ( 'NONE',  ( -22.37507221999729623, 149.9331680011685251, -1.622875787667645620 ) ) ;
#32541 = EDGE_LOOP ( 'NONE', ( #6131, #23849, #25229, #11635, #18245 ) ) ;
#32542 = CARTESIAN_POINT ( 'NONE',  ( -4.346810452489807020, 155.8404949922767742, 0.3425513195823395307 ) ) ;
#32543 = CARTESIAN_POINT ( 'NONE',  ( 5.566531978545880222, -14.14111126781847361, 3.212028819027522797 ) ) ;
#32544 = CARTESIAN_POINT ( 'NONE',  ( -5.008842170714641107, 117.3975374489157133, 0.7756408261732131715 ) ) ;
#32545 = ORIENTED_EDGE ( 'NONE', *, *, #13864, .F. ) ;
#32546 = CARTESIAN_POINT ( 'NONE',  ( 0.4560022058367742548, 118.7114656741295988, 0.6168833707790647436 ) ) ;
#32547 = CARTESIAN_POINT ( 'NONE',  ( 3.009276887026298031, 39.20946620154573736, -1.210121013456480599 ) ) ;
#32548 = CARTESIAN_POINT ( 'NONE',  ( -6.550797450135577910E-14, 84.67546620154573134, 2.164564701558966795E-29 ) ) ;
#32549 = VECTOR ( 'NONE', #9215, 1000.000000000000000 ) ;
#32550 = CARTESIAN_POINT ( 'NONE',  ( -22.54293160324732526, 149.6594668941642681, 0.7271591872719226357 ) ) ;
#32551 = ADVANCED_FACE ( 'NONE', ( #29340 ), #6838, .T. ) ;
#32552 = EDGE_CURVE ( 'NONE', #27974, #40883, #38396, .T. ) ;
#32553 = CARTESIAN_POINT ( 'NONE',  ( 23.16157447928863178, 142.6111785389246336, -0.1383437888640691449 ) ) ;
#32554 = CARTESIAN_POINT ( 'NONE',  ( -4.918266948219002899, 56.51499999999997215, -4.748921713023556812 ) ) ;
#32555 = CARTESIAN_POINT ( 'NONE',  ( -47.84356795211458291, 19.38525671449504983, 5.197506975155153697 ) ) ;
#32556 = CARTESIAN_POINT ( 'NONE',  ( 5.299459906814694143, 78.93540349268872092, 5.255323016343538711 ) ) ;
#32557 = DIRECTION ( 'NONE',  ( -0.8745520943968249084, 0.4849315768086533418, -5.271987356194193006E-16 ) ) ;
#32558 = CARTESIAN_POINT ( 'NONE',  ( -46.81005371095109524, 25.73327194510133253, 1.583310528698471664 ) ) ;
#32559 = CARTESIAN_POINT ( 'NONE',  ( -6.059261036834476144, 56.51499999999998636, 4.381499999999999950 ) ) ;
#32560 = CARTESIAN_POINT ( 'NONE',  ( -4.541827306795418018, 118.0696916868041626, 0.6339922499592595129 ) ) ;
#32561 = CARTESIAN_POINT ( 'NONE',  ( 3.682264917456193221, 72.48346620154573827, 0.07358041635424013294 ) ) ;
#32562 = ORIENTED_EDGE ( 'NONE', *, *, #31345, .T. ) ;
#32563 = ORIENTED_EDGE ( 'NONE', *, *, #27784, .T. ) ;
#32564 = CARTESIAN_POINT ( 'NONE',  ( -4.401450347368204064, 115.6909491485452719, -1.538494961457526955 ) ) ;
#32565 = AXIS2_PLACEMENT_3D ( 'NONE', #2878, #41860, #733 ) ;
#32566 = CARTESIAN_POINT ( 'NONE',  ( 8.425593340951261112, 119.6232722969281355, -1.082523533391888115 ) ) ;
#32567 = CARTESIAN_POINT ( 'NONE',  ( -5.263686092533428784, 116.7134249176580028, -1.019678336081760506 ) ) ;
#32568 = CARTESIAN_POINT ( 'NONE',  ( 4.674394623628864487, 117.8377812495729273, 1.036795958576792076 ) ) ;
#32569 = TOROIDAL_SURFACE ( 'NONE', #42115, 0.3809999999999990616, 0.2540000000000000036 ) ;
#32570 = CARTESIAN_POINT ( 'NONE',  ( -47.48049929620759002, 23.18975938597035125, -2.730405167055939497 ) ) ;
#32571 = CARTESIAN_POINT ( 'NONE',  ( -5.862724111891735923, 121.1554468101848130, -0.6631653705238500507 ) ) ;
#32572 = CARTESIAN_POINT ( 'NONE',  ( -3.385571042293893385, 115.7029692422994174, -1.641253599935611041 ) ) ;
#32573 = DIRECTION ( 'NONE',  ( 9.627370216492862708E-17, 1.000000000000000000, -0.000000000000000000 ) ) ;
#32574 = DIRECTION ( 'NONE',  ( 0.1906721105965055174, -0.9816537812491091808, 0.000000000000000000 ) ) ;
#32575 = CARTESIAN_POINT ( 'NONE',  ( 3.089687104934370598, 107.8271213589905386, -4.353618003723240371 ) ) ;
#32576 = CARTESIAN_POINT ( 'NONE',  ( -1.432854634133492899, 120.0849730816093910, -0.5085234606245936373 ) ) ;
#32577 = DIRECTION ( 'NONE',  ( -4.017660918040594346E-17, 1.000000000000000000, 2.376309959284834438E-19 ) ) ;
#32578 = DIRECTION ( 'NONE',  ( -0.9998004120163608288, -5.205824365704082573E-17, -0.01997839162482760098 ) ) ;
#32579 = DIRECTION ( 'NONE',  ( -9.627370216492862708E-17, -1.000000000000000000, 0.000000000000000000 ) ) ;
#32580 = CARTESIAN_POINT ( 'NONE',  ( -9.049360525155641710, 124.1535258118840517, -0.09135200362803799767 ) ) ;
#32581 = CARTESIAN_POINT ( 'NONE',  ( -2.395914033174281865, 1.367755174955888275, -3.957843245732672877 ) ) ;
#32583 = VERTEX_POINT ( 'NONE', #39146 ) ;
#32582 = CARTESIAN_POINT ( 'NONE',  ( -0.004913308686096432183, 116.7872217978203224, 0.2458820580207659867 ) ) ;
#32584 = LINE ( 'NONE', #19784, #9055 ) ;
#32585 = CARTESIAN_POINT ( 'NONE',  ( 3.745939827176673731, -15.15858284179406823, -0.4807645327530354340 ) ) ;
#32586 = CARTESIAN_POINT ( 'NONE',  ( -1.305241956589776819, 119.0230276286704054, 0.6306560096549496119 ) ) ;
#32587 = CARTESIAN_POINT ( 'NONE',  ( -0.8250140797137134330, 8.550980984719981137, 0.5181985368706800710 ) ) ;
#32588 = CARTESIAN_POINT ( 'NONE',  ( -20.48075987368149598, 152.5656283612522657, -1.113479615819600310 ) ) ;
#32589 = CARTESIAN_POINT ( 'NONE',  ( 0.1867991717342751268, 10.66319190514178139, -0.9583599856553294272 ) ) ;
#32590 = EDGE_CURVE ( 'NONE', #10724, #37473, #17707, .T. ) ;
#32591 = ORIENTED_EDGE ( 'NONE', *, *, #37363, .F. ) ;
#32592 = VERTEX_POINT ( 'NONE', #29122 ) ;
#32593 = CARTESIAN_POINT ( 'NONE',  ( -46.49274047292066570, 18.53875678104565594, 2.063467562158682433 ) ) ;
#32594 = CARTESIAN_POINT ( 'NONE',  ( 0.5964146925940678745, 106.0274289318137306, 5.278528196272315398 ) ) ;
#32595 = SHAPE_REPRESENTATION_RELATIONSHIP ( 'NONE' , 'NONE' ,  #11484, #21408 ) ;
#32596 = CARTESIAN_POINT ( 'NONE',  ( -2.706440023329564681, 120.6505882111413683, 0.2907491850344329221 ) ) ;
#32597 = CARTESIAN_POINT ( 'NONE',  ( 3.910559219094527528, -13.09373064504072737, 2.776858670901594994 ) ) ;
#32598 = CARTESIAN_POINT ( 'NONE',  ( 17.79400844405170190, 146.5573550606970628, -1.533700293046251772 ) ) ;
#32599 = CARTESIAN_POINT ( 'NONE',  ( -0.4560022058369030962, 118.7114656741295988, -0.6168833707790646326 ) ) ;
#32600 = DIRECTION ( 'NONE',  ( 5.188838149069472160E-16, -1.699382548006136559E-16, -1.000000000000000000 ) ) ;
#32601 = B_SPLINE_CURVE_WITH_KNOTS ( 'NONE', 3,
 ( #19431, #19850, #32648, #3910, #504, #6458 ),
 .UNSPECIFIED., .F., .F.,
 ( 4, 2, 4 ),
 ( 0.000000000000000000, 0.5000000000000000000, 1.000000000000000000 ),
 .UNSPECIFIED. ) ;
#32602 = CARTESIAN_POINT ( 'NONE',  ( 2.827333099181600584, -13.37427733298611443, 0.6166582517569209054 ) ) ;
#32603 = CARTESIAN_POINT ( 'NONE',  ( -0.1059412245877799363, 38.28537051638084421, -0.7326154344855524414 ) ) ;
#32604 = CARTESIAN_POINT ( 'NONE',  ( 9.310784039460415329, 124.2035065715909496, -0.04725383350292533535 ) ) ;
#32605 = ORIENTED_EDGE ( 'NONE', *, *, #5289, .F. ) ;
#32606 = DIRECTION ( 'NONE',  ( -0.000000000000000000, -0.000000000000000000, -1.000000000000000000 ) ) ;
#32607 = CARTESIAN_POINT ( 'NONE',  ( 0.4669423002395221012, 105.9272292791236794, 5.319618862452587749 ) ) ;
#32608 = VECTOR ( 'NONE', #8959, 1000.000000000000227 ) ;
#32609 = AXIS2_PLACEMENT_3D ( 'NONE', #19360, #2788, #12972 ) ;
#32610 = LINE ( 'NONE', #4500, #12967 ) ;
#32611 = EDGE_CURVE ( 'NONE', #37685, #27491, #32974, .T. ) ;
#32612 = CARTESIAN_POINT ( 'NONE',  ( -13.51785991797444098, 17.08228783296376108, 5.016499999999999737 ) ) ;
#32613 = DIRECTION ( 'NONE',  ( 0.9454731675810308378, -0.3256999990547930213, -6.328166980064887941E-15 ) ) ;
#32614 = CARTESIAN_POINT ( 'NONE',  ( 3.728135546147748336, 116.6403000632267464, -0.003128093132697572741 ) ) ;
#32615 = CARTESIAN_POINT ( 'NONE',  ( -7.140971181236958287, 122.4194348751405101, -0.03314210641492758291 ) ) ;
#32616 = CARTESIAN_POINT ( 'NONE',  ( -2.857476489931835673, 115.6909491485452577, 1.572699180235668903 ) ) ;
#32617 = LINE ( 'NONE', #32203, #1975 ) ;
#32618 = CARTESIAN_POINT ( 'NONE',  ( 0.5226899456406054467, 39.20946620154573026, -1.259808938293395908 ) ) ;
#32619 = EDGE_CURVE ( 'NONE', #12162, #34968, #21087, .T. ) ;
#32620 = CARTESIAN_POINT ( 'NONE',  ( 9.041969115052715722, 119.3941581119689204, 1.378656440977003461 ) ) ;
#32621 = CARTESIAN_POINT ( 'NONE',  ( -2.131885088311801901, 26.04095958170969638, -4.099730575217565232 ) ) ;
#32622 = CARTESIAN_POINT ( 'NONE',  ( 4.580344459542567748, 28.35322510196829171, -7.077419036913218164 ) ) ;
#32623 = CARTESIAN_POINT ( 'NONE',  ( -5.477710374292670714, 117.3472291391384061, -0.8783748813296128333 ) ) ;
#32624 = CARTESIAN_POINT ( 'NONE',  ( -1.846946891755202769, 121.3688471916803451, -0.3635544463458705300 ) ) ;
#32625 = CARTESIAN_POINT ( 'NONE',  ( -10.84307050033138786, 78.30450799593342026, 1.270000000000000240 ) ) ;
#32626 = DIRECTION ( 'NONE',  ( -0.8745520943968249084, 0.4849315768086533418, -5.271987356194193006E-16 ) ) ;
#32627 = CARTESIAN_POINT ( 'NONE',  ( -2.044950736525416701, 104.6144662015456674, 4.372199481676336319 ) ) ;
#32628 = CARTESIAN_POINT ( 'NONE',  ( 2.488009491785908800, 18.85968022696138391, -3.895047602898422223 ) ) ;
#32629 = CARTESIAN_POINT ( 'NONE',  ( -28.76494711669534610, 76.52965637509277030, 1.269999999999990470 ) ) ;
#32630 = CARTESIAN_POINT ( 'NONE',  ( -22.76738278397264281, 137.3906169244638136, -0.4549464913834382340 ) ) ;
#32631 = CARTESIAN_POINT ( 'NONE',  ( 3.219973314159829680, -14.13069947154231620, 2.606357176882864390 ) ) ;
#32632 = CARTESIAN_POINT ( 'NONE',  ( 1.918777129854390084, 121.7602717223048501, -0.2400857948923554031 ) ) ;
#32633 = CARTESIAN_POINT ( 'NONE',  ( -16.59152294496572111, 155.2525159475892167, 0.4418349252515508807 ) ) ;
#32634 = TOROIDAL_SURFACE ( 'NONE', #37404, 15.36699999999999555, 0.6350000000000000089 ) ;
#32635 = EDGE_LOOP ( 'NONE', ( #5370, #29822, #22249, #30748, #15358, #41459, #23232 ) ) ;
#32636 = CARTESIAN_POINT ( 'NONE',  ( -24.50334120614357047, 81.61487340491997600, -1.524000000000006461 ) ) ;
#32637 = AXIS2_PLACEMENT_3D ( 'NONE', #20360, #7610, #36581 ) ;
#32638 = ORIENTED_EDGE ( 'NONE', *, *, #34765, .F. ) ;
#32639 = FACE_OUTER_BOUND ( 'NONE', #35980, .T. ) ;
#32640 = CARTESIAN_POINT ( 'NONE',  ( 5.890162669548780094, -14.87046963210582362, 1.285284309844398898 ) ) ;
#32641 = CARTESIAN_POINT ( 'NONE',  ( -3.207104841129888584, 118.4902560533893592, 0.7629184910595989688 ) ) ;
#32642 = CARTESIAN_POINT ( 'NONE',  ( 20.51279501983843545, 150.9797539340098069, -1.282250019969887855 ) ) ;
#32643 = CARTESIAN_POINT ( 'NONE',  ( 4.440015753948663324, -2.305524871907271400, 1.325333094644747245 ) ) ;
#32644 = CARTESIAN_POINT ( 'NONE',  ( -58.57514867739262598, -0.1811137290223177321, -0.5238340084838408739 ) ) ;
#32645 = ORIENTED_EDGE ( 'NONE', *, *, #21628, .F. ) ;
#32646 = CARTESIAN_POINT ( 'NONE',  ( -58.34765594471348749, -0.2451624547642194951, -0.1853313705893772922 ) ) ;
#32647 = CARTESIAN_POINT ( 'NONE',  ( 0.1292312685652868276, 109.4728569552520554, 3.923176234211466440 ) ) ;
#32648 = CARTESIAN_POINT ( 'NONE',  ( 4.934253595602364761, 117.4065730964002228, 1.087905710704323736 ) ) ;
#32649 = CARTESIAN_POINT ( 'NONE',  ( -3.531217591821389501, 156.5024071230465097, 1.273243333543746303 ) ) ;
#32650 = CARTESIAN_POINT ( 'NONE',  ( 5.152406760161801991, 116.8381519984425125, 0.1413306424610384082 ) ) ;
#32651 = ADVANCED_FACE ( 'NONE', ( #28913 ), #42141, .T. ) ;
#32652 =( BOUNDED_SURFACE ( )  B_SPLINE_SURFACE ( 3, 2, ( 
 ( #24072, #7901, #40077 ),
 ( #14267, #14684, #27691 ),
 ( #40699, #27278, #20236 ),
 ( #23426, #37084, #4720 ) ),
 .UNSPECIFIED., .F., .F., .F. ) 
 B_SPLINE_SURFACE_WITH_KNOTS ( ( 4, 4 ),
 ( 3, 3 ),
 ( -1.125575372986152065E-06, 0.0001887214708706781534 ),
 ( 0.000000000000000000, 0.2790336440021598530 ),
 .UNSPECIFIED. ) 
 GEOMETRIC_REPRESENTATION_ITEM ( )  RATIONAL_B_SPLINE_SURFACE ( (
 ( 1.000000000000000000, 0.9331452035001246426, 0.9035998819730153286),
 ( 1.000000000000000000, 0.9331452033132299206, 0.9035998817035257868),
 ( 1.000000000000000000, 0.9331453013021652199, 0.9036000229969769482),
 ( 1.000000000000000000, 0.9331453801652662694, 0.9036001367122621364) ) ) 
 REPRESENTATION_ITEM ( '' )  SURFACE ( )  );
#32653 = CARTESIAN_POINT ( 'NONE',  ( 11.63135762381485883, 122.7176759045101022, -1.263630383496116005 ) ) ;
#32654 = CARTESIAN_POINT ( 'NONE',  ( -12.77966252534845992, 121.3369795956499928, -1.646308105693409685 ) ) ;
#32655 = CARTESIAN_POINT ( 'NONE',  ( -57.95878807693440393, 1.295030275130740094, -1.504629864475988787 ) ) ;
#32656 = ADVANCED_FACE ( 'NONE', ( #25926 ), #39490, .T. ) ;
#32657 = ORIENTED_EDGE ( 'NONE', *, *, #18885, .F. ) ;
#32658 = CARTESIAN_POINT ( 'NONE',  ( 4.601481835261479247, 118.0766341700411601, -0.5257344758955123654 ) ) ;
#32659 = CARTESIAN_POINT ( 'NONE',  ( 10.29759560803357488, 124.8461398015159745, -0.5204633524205694028 ) ) ;
#32660 = ORIENTED_EDGE ( 'NONE', *, *, #21163, .F. ) ;
#32661 = CARTESIAN_POINT ( 'NONE',  ( -17.73735868213794475, 147.0764175921665640, -2.241444305069557164 ) ) ;
#32662 = CARTESIAN_POINT ( 'NONE',  ( 3.116032494879745762, -15.28226460877120374, 3.911124699519683556 ) ) ;
#32663 = CARTESIAN_POINT ( 'NONE',  ( -4.243821914726944478, 105.1218540727933686, -3.250214477582284989 ) ) ;
#32664 = CARTESIAN_POINT ( 'NONE',  ( -17.14499999999999957, 71.11999999999999034, -5.016499999999999737 ) ) ;
#32665 = AXIS2_PLACEMENT_3D ( 'NONE', #18082, #15094, #25113 ) ;
#32666 = EDGE_CURVE ( 'NONE', #6241, #40015, #8971, .T. ) ;
#32667 = CARTESIAN_POINT ( 'NONE',  ( -4.881639387764474591, 117.7524908745723593, 0.7530060852826706563 ) ) ;
#32668 = CARTESIAN_POINT ( 'NONE',  ( 16.41634355132952194, 139.9843038322558186, 2.146987391100668940 ) ) ;
#32669 = CARTESIAN_POINT ( 'NONE',  ( -3.113414239748028223, 30.98679946927233431, 0.04088859964249486750 ) ) ;
#32670 = CARTESIAN_POINT ( 'NONE',  ( -0.3239230800893593276, 29.42979164457532804, -4.628216972995994993 ) ) ;
#32671 = CARTESIAN_POINT ( 'NONE',  ( 15.78659908162999947, 146.5797798787131399, 0.5456203974801299150 ) ) ;
#32672 = CARTESIAN_POINT ( 'NONE',  ( -53.68435271313694557, 11.12367579685427721, -3.945100831076026715 ) ) ;
#32674 = ORIENTED_EDGE ( 'NONE', *, *, #31562, .F. ) ;
#32673 = CARTESIAN_POINT ( 'NONE',  ( -45.30933510662926977, 19.89173180141312614, -2.333898071402948027 ) ) ;
#32675 = CARTESIAN_POINT ( 'NONE',  ( -5.557118726059879776, 116.7202209307960459, -0.2768648844130547904 ) ) ;
#32676 = CARTESIAN_POINT ( 'NONE',  ( -5.586884702347495235, 72.99146620154573384, -0.1116392523995361763 ) ) ;
#32677 = DIRECTION ( 'NONE',  ( 0.9336303900108852138, 0.3582377630123916301, 4.235673982319075372E-16 ) ) ;
#32678 = PLANE ( 'NONE',  #5039 ) ;
#32679 = CARTESIAN_POINT ( 'NONE',  ( -11.65115770210962687, 16.51000000000000156, 4.908176479697702099 ) ) ;
#32680 = DIRECTION ( 'NONE',  ( -4.017660918040594346E-17, 1.000000000000000000, 2.376309959284834438E-19 ) ) ;
#32681 = CARTESIAN_POINT ( 'NONE',  ( -8.480639930781094904, 68.51064353654967931, -1.523999999999995802 ) ) ;
#32682 = CARTESIAN_POINT ( 'NONE',  ( -9.094996104468901166, 78.64197151092922411, -5.392902600000144986 ) ) ;
#32683 = CARTESIAN_POINT ( 'NONE',  ( -54.50298212578950796, 9.515077312548310573, 3.630897911711898018 ) ) ;
#32684 = CARTESIAN_POINT ( 'NONE',  ( -57.95878807693440393, 1.295030275130740094, 1.504629864475967915 ) ) ;
#32685 = CARTESIAN_POINT ( 'NONE',  ( -2.803048170062614641, 116.6385632091030544, 0.1397181956995451058 ) ) ;
#32686 = EDGE_CURVE ( 'NONE', #18659, #329, #29359, .T. ) ;
#32687 = ORIENTED_EDGE ( 'NONE', *, *, #38382, .F. ) ;
#32688 = CARTESIAN_POINT ( 'NONE',  ( -54.55302389503632554, 12.80492160976152327, -0.5954867740798109876 ) ) ;
#32689 = CARTESIAN_POINT ( 'NONE',  ( 6.978044078171404152, 121.9510782527418371, 0.05806353974079936364 ) ) ;
#32690 = VERTEX_POINT ( 'NONE', #9849 ) ;
#32691 = CARTESIAN_POINT ( 'NONE',  ( 3.960807457435879364, 115.7035851291592934, -1.436426024118471867 ) ) ;
#32693 = CARTESIAN_POINT ( 'NONE',  ( -5.939593986634166711, 121.5467800236367424, -0.1471147542197154823 ) ) ;
#32692 = CIRCLE ( 'NONE', #17712, 3.683000000000001162 ) ;
#32694 = CARTESIAN_POINT ( 'NONE',  ( 5.943076596790061394, -13.74187730036333122, 2.284392803971454278 ) ) ;
#32695 = CARTESIAN_POINT ( 'NONE',  ( -18.85079593648351803, 152.0234722879370111, 1.474728064877437239 ) ) ;
#32696 = CARTESIAN_POINT ( 'NONE',  ( -17.32429653712378936, 61.56493206124108042, 1.524000000000000243 ) ) ;
#32697 = CARTESIAN_POINT ( 'NONE',  ( 5.710605682675650385, 159.1232349745254453, 0.3332304182141802573 ) ) ;
#32698 = CARTESIAN_POINT ( 'NONE',  ( 2.062287441005058675, -15.63671396113243439, 5.843295106519123649 ) ) ;
#32699 = CARTESIAN_POINT ( 'NONE',  ( 5.252108655715503005, 115.6909491485453145, -0.9240985664890069007 ) ) ;
#32700 = CARTESIAN_POINT ( 'NONE',  ( -0.4650136207426652235, -7.476398416381191403, -0.8572754866018892361 ) ) ;
#32701 = CARTESIAN_POINT ( 'NONE',  ( -22.69169950426951132, 137.3157656003441787, -0.5971823736698285146 ) ) ;
#32702 = CARTESIAN_POINT ( 'NONE',  ( -48.55954782883388532, 18.47106080339405310, -5.181360474636990787 ) ) ;
#32703 = FACE_OUTER_BOUND ( 'NONE', #27592, .T. ) ;
#32704 = VERTEX_POINT ( 'NONE', #26033 ) ;
#32705 = CARTESIAN_POINT ( 'NONE',  ( -5.560072573240018912, 117.2208093686857922, 0.5507231274924011544 ) ) ;
#32706 = VERTEX_POINT ( 'NONE', #287 ) ;
#32707 = CARTESIAN_POINT ( 'NONE',  ( -17.87798177106725817, 144.5560955566678558, 1.636306359874434291 ) ) ;
#32708 = DIRECTION ( 'NONE',  ( -0.8745520943968235761, 0.4849315768086558398, -4.268512490100410909E-16 ) ) ;
#32709 = CARTESIAN_POINT ( 'NONE',  ( 18.99721151120893126, 152.1029585079319020, 2.158688780372492566 ) ) ;
#32710 = CARTESIAN_POINT ( 'NONE',  ( 19.78762832257843129, 149.1964539096042870, -1.700649111281397508 ) ) ;
#32711 = CARTESIAN_POINT ( 'NONE',  ( 0.2491751845298053603, 0.8914985761586250446, 0.9476022430964140542 ) ) ;
#32712 = CARTESIAN_POINT ( 'NONE',  ( -19.40029886644223467, 131.9512773411433670, -1.949052778313793866 ) ) ;
#32713 = CARTESIAN_POINT ( 'NONE',  ( 4.865035472571053177, 117.7603446447191260, -0.7858820013116090131 ) ) ;
#32714 = ADVANCED_FACE ( 'NONE', ( #23241 ), #7510, .T. ) ;
#32715 = CIRCLE ( 'NONE', #25886, 0.3810000000000015041 ) ;
#32716 = CARTESIAN_POINT ( 'NONE',  ( 5.771537640388776147, 118.4310156723767307, 0.6642225483502961492 ) ) ;
#32717 = EDGE_CURVE ( 'NONE', #7084, #36618, #29448, .T. ) ;
#32718 = CARTESIAN_POINT ( 'NONE',  ( 0.5800011805206757298, 120.2131932824006526, -0.3882866552237519420 ) ) ;
#32719 = CARTESIAN_POINT ( 'NONE',  ( -10.21313493804737682, 125.9885856776569426, -0.1666469060040937644 ) ) ;
#32720 = ORIENTED_EDGE ( 'NONE', *, *, #39685, .T. ) ;
#32721 = CARTESIAN_POINT ( 'NONE',  ( -0.9182646862280283706, 157.4778559999684830, -1.599919928990592988 ) ) ;
#32722 = CARTESIAN_POINT ( 'NONE',  ( 4.515093156845158440, -15.50826969562475810, 4.181389551362865831 ) ) ;
#32723 = CARTESIAN_POINT ( 'NONE',  ( -25.56614996202194590, 73.65611136973726047, 1.523999999999993804 ) ) ;
#32724 = TOROIDAL_SURFACE ( 'NONE', #12956, 8.794749999999996959, 0.2540000000000000036 ) ;
#32725 = CARTESIAN_POINT ( 'NONE',  ( -48.53848336910535011, 19.22582880449973075, -5.323527254358048744 ) ) ;
#32726 = ORIENTED_EDGE ( 'NONE', *, *, #4291, .F. ) ;
#32727 = PRODUCT_DEFINITION_SHAPE ( 'NONE', 'NONE',  #42166 ) ;
#32728 = CARTESIAN_POINT ( 'NONE',  ( 17.13831219182123888, 149.7102054596878702, 2.353104315458284468 ) ) ;
#32729 = CARTESIAN_POINT ( 'NONE',  ( -6.585902005698190595E-14, 91.53346620154573543, 1.207165459464729879E-19 ) ) ;
#32730 = AXIS2_PLACEMENT_3D ( 'NONE', #31085, #1924, #38329 ) ;
#32731 = CARTESIAN_POINT ( 'NONE',  ( 0.8838529761740171464, 116.4325158421065680, 0.01766148591713753366 ) ) ;
#32732 = CARTESIAN_POINT ( 'NONE',  ( -3.306315723242934990, 118.9685052735122355, 0.5531158949559313864 ) ) ;
#32733 = CARTESIAN_POINT ( 'NONE',  ( -8.431077252155047219, 22.10977948022283357, 0.3997009428958171462 ) ) ;
#32734 = CARTESIAN_POINT ( 'NONE',  ( 5.218277051435741498, 121.1607713875043117, 0.4468594773273021903 ) ) ;
#32735 = CARTESIAN_POINT ( 'NONE',  ( 14.99285373232496532, 120.9606250904355704, -0.4613734978017340338 ) ) ;
#32736 = DIRECTION ( 'NONE',  ( -5.188838149069471174E-16, 1.699382548006136313E-16, 1.000000000000000000 ) ) ;
#32737 = DIRECTION ( 'NONE',  ( -4.017660918040594346E-17, 1.000000000000000000, 2.376309959284834438E-19 ) ) ;
#32738 = CARTESIAN_POINT ( 'NONE',  ( -1.421877081889727945, 159.6054662015457666, -0.01472409299311845318 ) ) ;
#32739 = ORIENTED_EDGE ( 'NONE', *, *, #1932, .F. ) ;
#32740 = CARTESIAN_POINT ( 'NONE',  ( 5.171081541123786707, 120.2810485551120223, -0.6437068486157979663 ) ) ;
#32741 = CARTESIAN_POINT ( 'NONE',  ( 2.467290606313818913, -15.47138089097717106, 5.855268220497546139 ) ) ;
#32742 = CARTESIAN_POINT ( 'NONE',  ( -11.59282501421117750, 128.2970750771678752, -0.8590849294959498339 ) ) ;
#32743 = CARTESIAN_POINT ( 'NONE',  ( 1.975269416564901404, -15.10067923695700109, 5.832845082603779652 ) ) ;
#32744 = DIRECTION ( 'NONE',  ( 5.188838149069472160E-16, -1.699382548006136559E-16, -1.000000000000000000 ) ) ;
#32745 = VECTOR ( 'NONE', #2391, 1000.000000000000000 ) ;
#32746 = CARTESIAN_POINT ( 'NONE',  ( 21.64466742782788700, 132.7051459832101443, 0.4972030839502444288 ) ) ;
#32747 = ORIENTED_EDGE ( 'NONE', *, *, #6581, .F. ) ;
#32748 = CARTESIAN_POINT ( 'NONE',  ( -3.812863311134618183, 2.017465188139291765, -2.614655560905410958 ) ) ;
#32749 = CARTESIAN_POINT ( 'NONE',  ( -13.70496720262328161, 119.6480011847128253, -0.2738578607176475055 ) ) ;
#32750 = CARTESIAN_POINT ( 'NONE',  ( -6.606344270946872901E-14, 95.34346620154573770, 1.014423412895214384E-29 ) ) ;
#32751 = CARTESIAN_POINT ( 'NONE',  ( 5.030795403078426098, 113.7219408396588562, 1.867219066840775987 ) ) ;
#32752 = CARTESIAN_POINT ( 'NONE',  ( 6.087437787857826521, 121.3262240766859890, 0.5122669965167206962 ) ) ;
#32753 = CARTESIAN_POINT ( 'NONE',  ( 0.7003524534433175353, 11.14785949628657669, 4.567531960304466843 ) ) ;
#32754 = CARTESIAN_POINT ( 'NONE',  ( 22.43644356963070763, 149.3130771379323392, 1.752678757896036776 ) ) ;
#32755 = CARTESIAN_POINT ( 'NONE',  ( 15.52687642492882070, 147.5330934759543879, 0.3102639428822866474 ) ) ;
#32757 = CARTESIAN_POINT ( 'NONE',  ( 16.68922378205029489, 153.6190162071354735, -1.533137601955099294 ) ) ;
#32756 = DIRECTION ( 'NONE',  ( 5.188838149069472160E-16, -1.699382548006136559E-16, -1.000000000000000000 ) ) ;
#32758 = CIRCLE ( 'NONE', #23891, 0.5080000000000002292 ) ;
#32759 = CARTESIAN_POINT ( 'NONE',  ( 1.368391094521330897, 11.37271669962338372, 4.434453701053673313 ) ) ;
#32760 = CARTESIAN_POINT ( 'NONE',  ( -14.69808362324415363, 120.8948172685174001, -1.121060376578428386 ) ) ;
#32761 = VERTEX_POINT ( 'NONE', #26882 ) ;
#32762 = CARTESIAN_POINT ( 'NONE',  ( -14.35733687469677200, 139.0340687859245463, 0.1707862337897579352 ) ) ;
#32763 = CARTESIAN_POINT ( 'NONE',  ( 3.397480601066255712, -15.04020002808364964, 5.521695076403254632 ) ) ;
#32764 = CIRCLE ( 'NONE', #2859, 0.5080000000000002292 ) ;
#32765 = CARTESIAN_POINT ( 'NONE',  ( -6.654617103318593247E-14, 104.6144662015457243, 1.534725424433578570E-31 ) ) ;
#32766 = CARTESIAN_POINT ( 'NONE',  ( 4.999324130125957666, 117.3993846056547738, 0.8255830379890115589 ) ) ;
#32767 = VERTEX_POINT ( 'NONE', #16226 ) ;
#32768 = CARTESIAN_POINT ( 'NONE',  ( 15.19444909298863777, 153.0676604005411434, 2.356382943223728876 ) ) ;
#32769 = DIRECTION ( 'NONE',  ( -4.017660918040594346E-17, 1.000000000000000000, 2.376309959284834438E-19 ) ) ;
#32770 = DIRECTION ( 'NONE',  ( -0.9998004120163610509, -4.016384292689131511E-17, -0.01997839162482749689 ) ) ;
#32771 = CIRCLE ( 'NONE', #25940, 6.350000000000004974 ) ;
#32772 = TOROIDAL_SURFACE ( 'NONE', #39590, 3.111499999999999488, 0.2540000000000000036 ) ;
#32773 = CARTESIAN_POINT ( 'NONE',  ( -21.45272375726306180, 151.3201912522522719, 0.6338752469853824456 ) ) ;
#32774 = CARTESIAN_POINT ( 'NONE',  ( 3.006797519324799772, 15.24566924451032435, -7.865828698519952589 ) ) ;
#32775 = AXIS2_PLACEMENT_3D ( 'NONE', #3693, #10483, #7300 ) ;
#32776 = CARTESIAN_POINT ( 'NONE',  ( 0.3220477894874517188, 116.6413645472259617, -0.1880332438949531837 ) ) ;
#32777 = CARTESIAN_POINT ( 'NONE',  ( -11.53797084252497562, 82.58007221317646440, 1.523999999999999577 ) ) ;
#32778 = CARTESIAN_POINT ( 'NONE',  ( -5.036351857865265735, 117.3993844875897139, 0.5494637324817667201 ) ) ;
#32779 = CARTESIAN_POINT ( 'NONE',  ( -50.22242345129090779, 22.76272812237061771, -9.508731853559545367E-15 ) ) ;
#32780 = CARTESIAN_POINT ( 'NONE',  ( -4.937359598886440715, 117.4097706984612302, -1.081953738475849747 ) ) ;
#32781 = CARTESIAN_POINT ( 'NONE',  ( -52.06546789126484498, 13.38259882428268632, 4.575081192416372566 ) ) ;
#32782 = CARTESIAN_POINT ( 'NONE',  ( -58.72811565343341300, -0.3134725424711655162, 0.2575438388786236987 ) ) ;
#32783 = CARTESIAN_POINT ( 'NONE',  ( -4.463408765292727232, 118.1258133513832860, 0.5547340330597864133 ) ) ;
#32784 = DIRECTION ( 'NONE',  ( 0.8572391118119472297, 0.5149185422762166953, 0.000000000000000000 ) ) ;
#32785 = ORIENTED_EDGE ( 'NONE', *, *, #12223, .T. ) ;
#32786 = VERTEX_POINT ( 'NONE', #29233 ) ;
#32787 = PLANE ( 'NONE',  #2952 ) ;
#32788 = CARTESIAN_POINT ( 'NONE',  ( -6.069717446804125949, 119.4746383518879043, -1.260100842361058016 ) ) ;
#32789 = CARTESIAN_POINT ( 'NONE',  ( -5.192700560041021873, 116.2637919873444190, -1.171650394069924772 ) ) ;
#32790 = CARTESIAN_POINT ( 'NONE',  ( 4.556952415498273901, 118.0383946930539878, 0.8497061536611607568 ) ) ;
#32791 = CARTESIAN_POINT ( 'NONE',  ( -46.81330379368907302, 25.73549360603863434, -1.450859712031395521 ) ) ;
#32792 = CARTESIAN_POINT ( 'NONE',  ( -16.47979853205677969, 146.5532241433796230, -1.607449420861547740 ) ) ;
#32793 = CARTESIAN_POINT ( 'NONE',  ( -4.532044145959075010, 115.7029491485453718, -1.515528964257317757 ) ) ;
#32794 = CYLINDRICAL_SURFACE ( 'NONE', #7440, 12.69999999999999751 ) ;
#32795 = CARTESIAN_POINT ( 'NONE',  ( 4.812383263389150123, 112.7966860322829206, -2.369499567760593450 ) ) ;
#32796 = CARTESIAN_POINT ( 'NONE',  ( -14.71707226966683812, 150.5114039713088516, -1.846696807168831000 ) ) ;
#32797 =( NAMED_UNIT ( * ) PLANE_ANGLE_UNIT ( ) SI_UNIT ( $, .RADIAN. ) );
#32798 = CARTESIAN_POINT ( 'NONE',  ( -6.431420355030265265E-14, 156.3034662015457172, 9.897580308537652682E-17 ) ) ;
#32799 = CARTESIAN_POINT ( 'NONE',  ( 7.810699835753124098, 122.5400548747105915, -0.1271298699639721308 ) ) ;
#32800 = CARTESIAN_POINT ( 'NONE',  ( -10.10118861072700192, 125.9371159002616309, -0.1041072054866566399 ) ) ;
#32801 = CARTESIAN_POINT ( 'NONE',  ( -4.476207883417873568, -7.053342675672244155, -1.178223045331058705 ) ) ;
#32802 = CARTESIAN_POINT ( 'NONE',  ( 19.79238143276385031, 128.7876384977266468, 1.131474956103616814 ) ) ;
#32803 = CARTESIAN_POINT ( 'NONE',  ( -4.377002418771855474, 72.24507371176854065, -1.523999999999994248 ) ) ;
#32804 = CARTESIAN_POINT ( 'NONE',  ( 3.866492242221801767, -15.24987600803320831, 0.6064936129020901401 ) ) ;
#32805 = CARTESIAN_POINT ( 'NONE',  ( -10.43940122747819466, 155.6679353847891321, 1.745147575944303364 ) ) ;
#32806 = CARTESIAN_POINT ( 'NONE',  ( -0.8880852245287531588, 7.049514723814470862, -0.3999422104893632923 ) ) ;
#32807 = CARTESIAN_POINT ( 'NONE',  ( -22.89058624538214204, 149.8162411397050278, -1.183733681586530917 ) ) ;
#32808 = AXIS2_PLACEMENT_3D ( 'NONE', #8955, #21922, #8745 ) ;
#32809 = CARTESIAN_POINT ( 'NONE',  ( 0.7511875256325919459, -11.68598654017788974, 0.6195722450943603743 ) ) ;
#32810 = ORIENTED_EDGE ( 'NONE', *, *, #4075, .T. ) ;
#32811 = VERTEX_POINT ( 'NONE', #39042 ) ;
#32812 = CARTESIAN_POINT ( 'NONE',  ( -44.40685758373553682, 19.43703734468912714, 0.2085933842879050815 ) ) ;
#32813 = CARTESIAN_POINT ( 'NONE',  ( 0.1274156416094324173, 105.9117620634264370, 5.326488824310051662 ) ) ;
#32814 = PRODUCT_CONTEXT ( 'NONE', #30877, 'mechanical' ) ;
#32815 = CARTESIAN_POINT ( 'NONE',  ( -1.739825554503067861, 156.3676537730497387, 0.7044751146431476041 ) ) ;
#32816 = CARTESIAN_POINT ( 'NONE',  ( 4.249299001760414640, -12.92553893317818847, 2.698699680779739207 ) ) ;
#32817 = CARTESIAN_POINT ( 'NONE',  ( 15.43236126668700159, 134.8939017613128328, -1.443262610673740953 ) ) ;
#32818 = CARTESIAN_POINT ( 'NONE',  ( -8.740007204533959850, 120.0394951565550343, -1.484413609726634942 ) ) ;
#32819 = DIRECTION ( 'NONE',  ( -0.8745520943968235761, 0.4849315768086558953, -5.361993529360570985E-16 ) ) ;
#32820 = CARTESIAN_POINT ( 'NONE',  ( 3.026662605148213725, -13.87242449132548217, 1.205013440933411228 ) ) ;
#32821 = CARTESIAN_POINT ( 'NONE',  ( -4.432242455686237648, 32.76553509196318004, 1.287969469385143784 ) ) ;
#32822 = CARTESIAN_POINT ( 'NONE',  ( 0.6587526420362558310, 156.3106852680424765, -0.1744449402554845152 ) ) ;
#32823 = AXIS2_PLACEMENT_3D ( 'NONE', #1818, #30766, #34396 ) ;
#32824 = EDGE_LOOP ( 'NONE', ( #9631, #17587 ) ) ;
#32825 = CARTESIAN_POINT ( 'NONE',  ( -4.163217485963554232, 111.0900967538983650, 3.043985244824447101 ) ) ;
#32826 = CARTESIAN_POINT ( 'NONE',  ( 17.14499999999999957, 71.11999999999999034, 5.016499999999999737 ) ) ;
#32827 = CARTESIAN_POINT ( 'NONE',  ( -28.65049350906917880, 77.81814547195517662, 1.269999999999991136 ) ) ;
#32828 = DIRECTION ( 'NONE',  ( -0.8745520943968243532, 0.4849315768086547296, -5.361993529360573944E-16 ) ) ;
#32829 = CARTESIAN_POINT ( 'NONE',  ( 20.42271720105680188, 129.0384130229076334, 0.2828206407990420113 ) ) ;
#32830 = CARTESIAN_POINT ( 'NONE',  ( -6.920469006312010229, 121.8192184429722005, 0.01800753507563507619 ) ) ;
#32831 = AXIS2_PLACEMENT_3D ( 'NONE', #30369, #10777, #7387 ) ;
#32832 = CARTESIAN_POINT ( 'NONE',  ( -1.648859552577025323, 115.6909491485452577, 1.667642768541721887 ) ) ;
#32833 = DIRECTION ( 'NONE',  ( -1.000000000000000000, 0.000000000000000000, 0.000000000000000000 ) ) ;
#32834 = CARTESIAN_POINT ( 'NONE',  ( 2.511959498749158470, 39.20946620154573026, -1.220058598423863661 ) ) ;
#32835 = CARTESIAN_POINT ( 'NONE',  ( 18.59893286765435505, 151.9584835496716266, 2.273025404440325303 ) ) ;
#32836 = CARTESIAN_POINT ( 'NONE',  ( 3.087053954869741101, 14.59627045569285286, -3.440871586639639990 ) ) ;
#32837 = CARTESIAN_POINT ( 'NONE',  ( 0.01634572621781915994, 29.22912819268679030, -8.429653881604959764 ) ) ;
#32838 = CARTESIAN_POINT ( 'NONE',  ( 2.187205382360373651, 116.7606846954971331, -0.4172344709117405959 ) ) ;
#32839 = CARTESIAN_POINT ( 'NONE',  ( -3.156357112953910082, 123.6198120039584154, -0.1457842492014823077 ) ) ;
#32840 = DIRECTION ( 'NONE',  ( -0.8745520943968235761, 0.4849315768086558398, -4.268512490100410909E-16 ) ) ;
#32841 = DIRECTION ( 'NONE',  ( -5.188838149069471174E-16, 1.699382548006136313E-16, 1.000000000000000000 ) ) ;
#32842 = CARTESIAN_POINT ( 'NONE',  ( 3.196719817593447033, 104.6144662015522329, 4.273492549843798116 ) ) ;
#32843 = CARTESIAN_POINT ( 'NONE',  ( -1.756104463947763206, 14.33678105357426702, 4.288642365192034234 ) ) ;
#32844 = DIRECTION ( 'NONE',  ( -4.017660918040594346E-17, 1.000000000000000000, 2.376309959284832031E-19 ) ) ;
#32845 = CARTESIAN_POINT ( 'NONE',  ( 13.85159022459153988, 12.96416000000000146, -5.016499999999999737 ) ) ;
#32846 = CARTESIAN_POINT ( 'NONE',  ( 2.715444768400132158, -14.72438443971033095, 4.720152092698882029 ) ) ;
#32847 = CARTESIAN_POINT ( 'NONE',  ( 1.135428393696602312, 110.6314368487224300, -3.415474402745806159 ) ) ;
#32848 = CARTESIAN_POINT ( 'NONE',  ( -22.82237111512532124, 142.4248215231809240, 0.5244786342524968559 ) ) ;
#32849 = AXIS2_PLACEMENT_3D ( 'NONE', #40232, #11027, #24008 ) ;
#32850 = CARTESIAN_POINT ( 'NONE',  ( -12.21488373879589240, 71.11999999999999034, -5.016499999999999737 ) ) ;
#32851 = VERTEX_POINT ( 'NONE', #23031 ) ;
#32852 = CARTESIAN_POINT ( 'NONE',  ( 5.035933200060415338, 117.3993844219003648, -0.5513780243448201945 ) ) ;
#32853 = ORIENTED_EDGE ( 'NONE', *, *, #33432, .F. ) ;
#32854 = CARTESIAN_POINT ( 'NONE',  ( -15.42835734045148577, 79.74558783746837776, 1.523999999999998023 ) ) ;
#32855 = CARTESIAN_POINT ( 'NONE',  ( 5.215289103204772125, -15.32183344268082870, 2.967178555186370303 ) ) ;
#32856 = CARTESIAN_POINT ( 'NONE',  ( -6.760483308329498620, 119.1290971219625021, 1.000752511853993054 ) ) ;
#32857 = CARTESIAN_POINT ( 'NONE',  ( 13.46300103848306406, 120.9245410081625209, -0.9131080906212012405 ) ) ;
#32858 = CARTESIAN_POINT ( 'NONE',  ( -2.424025297795170619, -5.104216246930970868, 3.935102955759355758 ) ) ;
#32859 = EDGE_CURVE ( 'NONE', #8461, #8441, #35854, .T. ) ;
#32860 = CARTESIAN_POINT ( 'NONE',  ( -58.79373602274613830, -0.2918016666370280565, -0.1550872664390397226 ) ) ;
#32861 = VERTEX_POINT ( 'NONE', #6668 ) ;
#32862 = DIRECTION ( 'NONE',  ( 5.188838149069472160E-16, -1.699382548006136559E-16, -1.000000000000000000 ) ) ;
#32863 = CARTESIAN_POINT ( 'NONE',  ( 0.7402556297410838315, 119.5055576915191580, 0.7321893670752779304 ) ) ;
#32864 = CARTESIAN_POINT ( 'NONE',  ( -4.737627528408766331, 117.7521883752312419, 0.9000133201668191196 ) ) ;
#32865 = CARTESIAN_POINT ( 'NONE',  ( -0.5698427240851328124, 120.0661220204379305, 0.4260729765348977294 ) ) ;
#32866 = CARTESIAN_POINT ( 'NONE',  ( -4.757346424997288103, 117.3993836135861386, -1.207075064218979810 ) ) ;
#32867 = CARTESIAN_POINT ( 'NONE',  ( 16.81178602683893075, 135.2943057719725459, -1.678525023343173439 ) ) ;
#32868 = CARTESIAN_POINT ( 'NONE',  ( -16.61465421735670844, 153.6190162071354735, -2.198628343207905900 ) ) ;
#32869 = CARTESIAN_POINT ( 'NONE',  ( -58.23017998949752183, 0.6774554162835566551, -1.209604144815722426 ) ) ;
#32870 = AXIS2_PLACEMENT_3D ( 'NONE', #36214, #20206, #6605 ) ;
#32871 = ORIENTED_EDGE ( 'NONE', *, *, #41808, .F. ) ;
#32872 = CARTESIAN_POINT ( 'NONE',  ( 4.361691748181014461, 118.1815233605024957, -0.4501171095398698863 ) ) ;
#32873 = EDGE_CURVE ( 'NONE', #5804, #28106, #30724, .T. ) ;
#32874 = CARTESIAN_POINT ( 'NONE',  ( 9.326662024493369785, 153.8845013697122965, -0.4488502173044092158 ) ) ;
#32875 = ORIENTED_EDGE ( 'NONE', *, *, #35448, .T. ) ;
#32876 = CARTESIAN_POINT ( 'NONE',  ( -15.64494829320037894, 134.9797526104055123, -2.135645317121837472 ) ) ;
#32877 = CARTESIAN_POINT ( 'NONE',  ( 2.816406720412386822, -15.24816796146632925, 4.372395393210481984 ) ) ;
#32878 = CARTESIAN_POINT ( 'NONE',  ( -5.326136116496724249, 105.1224662015457341, -0.4468285755459980302 ) ) ;
#32879 = VECTOR ( 'NONE', #26328, 1000.000000000000114 ) ;
#32880 = CARTESIAN_POINT ( 'NONE',  ( 0.02983097946976470335, 117.3993836135854707, -1.492864285907033572 ) ) ;
#32881 = CARTESIAN_POINT ( 'NONE',  ( -4.255528399684056495, 7.899375212487111497, -1.818898740287305138 ) ) ;
#32882 = CARTESIAN_POINT ( 'NONE',  ( 13.40752216115192752, 152.3772590505219569, 2.011877943007317704 ) ) ;
#32883 = CARTESIAN_POINT ( 'NONE',  ( -2.651076796310585237, 29.59993426230072089, 0.1800044463941182782 ) ) ;
#32884 = CARTESIAN_POINT ( 'NONE',  ( 3.121479725567877228, 16.06095178295013071, 3.416230322513892137 ) ) ;
#32885 = CARTESIAN_POINT ( 'NONE',  ( 7.046279781204515480, 122.0586610246435129, 0.2738582164285300879 ) ) ;
#32886 = ADVANCED_FACE ( 'NONE', ( #29661 ), #3442, .T. ) ;
#32887 = EDGE_CURVE ( 'NONE', #37020, #20172, #28606, .T. ) ;
#32888 = CARTESIAN_POINT ( 'NONE',  ( -52.94148447887670272, 9.133269539094115430, -0.6394659809470596423 ) ) ;
#32889 = CARTESIAN_POINT ( 'NONE',  ( 2.182332163935870817, 116.1897970688993809, 0.04360819029724687795 ) ) ;
#32890 = CARTESIAN_POINT ( 'NONE',  ( -5.591489108514605455, 77.73497692594764885, -1.523999999999996025 ) ) ;
#32891 = CYLINDRICAL_SURFACE ( 'NONE', #20650, 0.2539999999999998925 ) ;
#32892 = CARTESIAN_POINT ( 'NONE',  ( -30.15519950990045572, 69.97033940222175374, 1.269999999999990692 ) ) ;
#32893 = DIRECTION ( 'NONE',  ( 0.9998004120163608288, 0.000000000000000000, 0.01997839162482736852 ) ) ;
#32894 = EDGE_CURVE ( 'NONE', #18166, #4212, #3482, .T. ) ;
#32895 = CARTESIAN_POINT ( 'NONE',  ( -5.177913976931289852, 65.30181249999996851, 5.372100000000007647 ) ) ;
#32896 = CARTESIAN_POINT ( 'NONE',  ( -4.074955089416341991, 118.2429491485453354, 0.1454234154749719787 ) ) ;
#32897 = DIRECTION ( 'NONE',  ( -0.1565721916418034432, -0.9876665170007953298, 8.659954811667511346E-17 ) ) ;
#32898 = CARTESIAN_POINT ( 'NONE',  ( -57.70501761738805158, 2.967533670478833763, 0.5494564739991059099 ) ) ;
#32899 = CARTESIAN_POINT ( 'NONE',  ( -57.67794393518098417, 1.927849678527493449, 1.763631237166035648 ) ) ;
#32900 = CARTESIAN_POINT ( 'NONE',  ( -11.66036501707591810, 118.7334002725740874, -0.02296568806519961800 ) ) ;
#32901 = AXIS2_PLACEMENT_3D ( 'NONE', #38057, #40427, #1864 ) ;
#32902 = ORIENTED_EDGE ( 'NONE', *, *, #2504, .F. ) ;
#32903 = CARTESIAN_POINT ( 'NONE',  ( -51.68405183998543606, 20.46365084016696301, -1.077913170022978826E-14 ) ) ;
#32904 = CARTESIAN_POINT ( 'NONE',  ( -7.787433790559666669, 122.6039481253381922, -0.2654969604323166865 ) ) ;
#32905 = ORIENTED_EDGE ( 'NONE', *, *, #18826, .F. ) ;
#32906 = FACE_OUTER_BOUND ( 'NONE', #286, .T. ) ;
#32907 = CARTESIAN_POINT ( 'NONE',  ( -10.21163942101063249, 125.9885856776569426, -0.2414886939513457842 ) ) ;
#32908 = CARTESIAN_POINT ( 'NONE',  ( 5.879588643049518559, -13.10657381646278274, 1.873965859954596969 ) ) ;
#32909 = CARTESIAN_POINT ( 'NONE',  ( -6.823161219633312236, 118.5360090424673274, 0.8871979454111539320 ) ) ;
#32910 = CARTESIAN_POINT ( 'NONE',  ( 1.893578447776079754, 19.08455809737888487, -4.224370802633358402 ) ) ;
#32911 = CIRCLE ( 'NONE', #1625, 0.2539999999999986158 ) ;
#32912 = CARTESIAN_POINT ( 'NONE',  ( 0.9351853929027724721, 116.6346273530297850, 0.2267945756083742659 ) ) ;
#32913 = CARTESIAN_POINT ( 'NONE',  ( 10.05542837570307668, 125.9185204131281210, 0.3475070621306587948 ) ) ;
#32914 = DIRECTION ( 'NONE',  ( -6.353134868986659519E-16, 1.000000000000000000, -0.000000000000000000 ) ) ;
#32915 = CARTESIAN_POINT ( 'NONE',  ( -0.4068859638909740339, 2.017459551269393359, -0.8868740919469698669 ) ) ;
#32916 = CARTESIAN_POINT ( 'NONE',  ( -2.764936593379252017, 116.5678055239024644, -0.1631480333911171920 ) ) ;
#32917 = CARTESIAN_POINT ( 'NONE',  ( -48.32642138504052554, 18.79167496732631548, -5.205639462496891134 ) ) ;
#32918 = CARTESIAN_POINT ( 'NONE',  ( 1.248107678658480997E-15, 12.96416000000000146, 0.000000000000000000 ) ) ;
#32919 = EDGE_LOOP ( 'NONE', ( #26917, #15485, #16833, #17117 ) ) ;
#32920 = CARTESIAN_POINT ( 'NONE',  ( 5.552057423463700125, 116.7478124476613743, 0.3280336575071842176 ) ) ;
#32921 = ORIENTED_EDGE ( 'NONE', *, *, #34488, .T. ) ;
#32922 = CARTESIAN_POINT ( 'NONE',  ( -8.280704432558593453, 121.1361926620737393, 1.000371422393417697 ) ) ;
#32923 = CARTESIAN_POINT ( 'NONE',  ( -57.77469323499624920, 0.9920357466726326123, -1.126265832864315808 ) ) ;
#32924 = CARTESIAN_POINT ( 'NONE',  ( 14.04349332752973467, 121.9525460547650226, 1.645664411013196604 ) ) ;
#32925 = CARTESIAN_POINT ( 'NONE',  ( 0.4802819474807752398, 118.7114656741295988, -0.5981741851633314289 ) ) ;
#32926 = AXIS2_PLACEMENT_3D ( 'NONE', #17105, #7328, #36093 ) ;
#32927 = CARTESIAN_POINT ( 'NONE',  ( 0.05045227420522335748, 0.5774631391966889016, 0.9751023907654918776 ) ) ;
#32928 = CARTESIAN_POINT ( 'NONE',  ( -7.956670401304606344, 118.4344479264803169, -1.111586840565143675 ) ) ;
#32929 = CARTESIAN_POINT ( 'NONE',  ( 4.665372465336868224, 118.0265698473236711, -0.5749007169697829545 ) ) ;
#32930 = CARTESIAN_POINT ( 'NONE',  ( 5.190622930436333604, 104.6144662015347535, 1.277265713775895151 ) ) ;
#32931 = CARTESIAN_POINT ( 'NONE',  ( 11.98504388954655120, 126.0992317015783328, -1.027991910846089985 ) ) ;
#32932 = CARTESIAN_POINT ( 'NONE',  ( -8.487687333566288572, 123.3253871723413368, -0.1696041924978711202 ) ) ;
#32933 = VERTEX_POINT ( 'NONE', #6876 ) ;
#32934 = CARTESIAN_POINT ( 'NONE',  ( -8.000928410381925815, 156.3870133935118076, -2.044342179695390893 ) ) ;
#32935 = CARTESIAN_POINT ( 'NONE',  ( 4.689621780486535663, -15.62538141832135707, 3.172200491054990579 ) ) ;
#32936 = AXIS2_PLACEMENT_3D ( 'NONE', #33376, #23554, #13976 ) ;
#32937 = CARTESIAN_POINT ( 'NONE',  ( -58.85382722430585289, -0.1409386484715794419, -5.573042720897973618E-15 ) ) ;
#32938 = CARTESIAN_POINT ( 'NONE',  ( -4.503792796599852544, 118.0666417019298109, -0.8213613892662697813 ) ) ;
#32939 = CARTESIAN_POINT ( 'NONE',  ( -47.19936399096371105, 20.24790404726484283, -5.251082349106865443 ) ) ;
#32940 = EDGE_CURVE ( 'NONE', #3642, #21134, #6845, .T. ) ;
#32941 = CARTESIAN_POINT ( 'NONE',  ( 4.147465018942456894, 118.2392518931096532, 0.3974363740737554274 ) ) ;
#32942 = CARTESIAN_POINT ( 'NONE',  ( 11.77984014550159841, 123.3160021321619695, 1.727726820665321350 ) ) ;
#32943 = FACE_OUTER_BOUND ( 'NONE', #2308, .T. ) ;
#32944 = EDGE_CURVE ( 'NONE', #4212, #26041, #12378, .T. ) ;
#32945 = CARTESIAN_POINT ( 'NONE',  ( 13.43845804798103316, 156.9141898299356512, 0.2685323735513602261 ) ) ;
#32946 = AXIS2_PLACEMENT_3D ( 'NONE', #26855, #10869, #30048 ) ;
#32947 = CARTESIAN_POINT ( 'NONE',  ( -3.689824518792605978, 110.1236525333376619, 3.433021159709686909 ) ) ;
#32948 = CARTESIAN_POINT ( 'NONE',  ( -4.443900581410109574, 30.07671411637534931, -7.177485988639727310 ) ) ;
#32949 = CARTESIAN_POINT ( 'NONE',  ( 10.03827118703578059, 124.8772485319846055, 0.7459150106818386305 ) ) ;
#32950 = CARTESIAN_POINT ( 'NONE',  ( 1.363555988950266862, 159.4956652290339605, -0.6451735917158236688 ) ) ;
#32951 = ADVANCED_FACE ( 'NONE', ( #1122 ), #17495, .T. ) ;
#32952 = DIRECTION ( 'NONE',  ( 0.8138664877804109299, -0.5810519254489895369, 0.000000000000000000 ) ) ;
#32953 = AXIS2_PLACEMENT_3D ( 'NONE', #190, #13163, #9961 ) ;
#32954 = DIRECTION ( 'NONE',  ( 0.8745520943968230210, -0.4849315768086570611, 6.829619984160674809E-16 ) ) ;
#32955 = ADVANCED_FACE ( 'NONE', ( #4532 ), #30492, .F. ) ;
#32956 = CARTESIAN_POINT ( 'NONE',  ( -23.21412382727114121, 149.6303025714371131, -0.4381719528662391117 ) ) ;
#32957 = ORIENTED_EDGE ( 'NONE', *, *, #34303, .T. ) ;
#32958 = CARTESIAN_POINT ( 'NONE',  ( 5.238238559199842825, 120.3605920493329222, -0.6250241856820153430 ) ) ;
#32959 = CARTESIAN_POINT ( 'NONE',  ( -17.14500000000466784, 71.11999999999886768, 1.523999999999998689 ) ) ;
#32960 = AXIS2_PLACEMENT_3D ( 'NONE', #19480, #13098, #32489 ) ;
#32961 = CARTESIAN_POINT ( 'NONE',  ( 0.006534791579796636780, 156.3267223255430167, -0.3270276925529294054 ) ) ;
#32962 = CARTESIAN_POINT ( 'NONE',  ( 4.270589230953349968, -11.85684205577233818, 0.9542379244983925091 ) ) ;
#32963 = ADVANCED_FACE ( 'NONE', ( #4951 ), #1334, .T. ) ;
#32964 = CARTESIAN_POINT ( 'NONE',  ( -14.55736095115768514, 121.4416029531759591, 0.8377414905974124304 ) ) ;
#32965 = CARTESIAN_POINT ( 'NONE',  ( -10.39928917620371784, 153.1223395828141918, -0.2078025466733117443 ) ) ;
#32966 = CARTESIAN_POINT ( 'NONE',  ( 23.35646125964490949, 148.8716009884483071, 0.5438655406665986458 ) ) ;
#32967 = ORIENTED_EDGE ( 'NONE', *, *, #20898, .T. ) ;
#32968 = CARTESIAN_POINT ( 'NONE',  ( 4.440015753948663324, -2.305524871907271400, 1.325333094644747245 ) ) ;
#32969 = CARTESIAN_POINT ( 'NONE',  ( -5.772319165918015749, 116.9338547871927858, -0.1153446742911716505 ) ) ;
#32970 = CARTESIAN_POINT ( 'NONE',  ( -46.60530155212503445, 26.17382724835477958, 1.269999999999988916 ) ) ;
#32971 = CARTESIAN_POINT ( 'NONE',  ( -8.228564651236517591, 120.5845947550810422, 1.087621554438485738 ) ) ;
#32972 = CARTESIAN_POINT ( 'NONE',  ( 4.615940417482057967, 3.801270455692812966, -0.2501868467277520436 ) ) ;
#32973 = CARTESIAN_POINT ( 'NONE',  ( 14.30926610799415144, 121.2650221238243944, 1.406141635412307300 ) ) ;
#32974 = LINE ( 'NONE', #9950, #32009 ) ;
#32976 = CARTESIAN_POINT ( 'NONE',  ( 13.79335258734181124, 122.1113760975138263, -1.168436778447113689 ) ) ;
#32975 = DIRECTION ( 'NONE',  ( 5.188838149069472160E-16, -1.699382548006136559E-16, -1.000000000000000000 ) ) ;
#32977 = CARTESIAN_POINT ( 'NONE',  ( 3.019445949670579665, 11.99742794009110014, 3.522755186455234000 ) ) ;
#32978 = CARTESIAN_POINT ( 'NONE',  ( -16.30933243092150420, 122.7783120765077030, -1.207982166786797151 ) ) ;
#32979 = EDGE_LOOP ( 'NONE', ( #2040, #5371, #41753, #20558 ) ) ;
#32980 = LINE ( 'NONE', #13370, #40237 ) ;
#32981 = ORIENTED_EDGE ( 'NONE', *, *, #2971, .T. ) ;
#32982 = CARTESIAN_POINT ( 'NONE',  ( -9.203139800278419713, 153.8854248570426080, 0.2095608753156675830 ) ) ;
#32983 = CARTESIAN_POINT ( 'NONE',  ( 4.517131889307780312, -14.80175198191645336, 4.712020298053779754 ) ) ;
#32984 = DIRECTION ( 'NONE',  ( -0.9998004120163608288, 0.000000000000000000, -0.01997839162482747608 ) ) ;
#32985 = CARTESIAN_POINT ( 'NONE',  ( 2.829627719599027369, -13.65247383265987757, 0.5238048331051645690 ) ) ;
#32986 = VERTEX_POINT ( 'NONE', #24099 ) ;
#32987 = CARTESIAN_POINT ( 'NONE',  ( 19.49537437117577454, 147.7952244890416296, 2.518105945687704406 ) ) ;
#32988 = DIRECTION ( 'NONE',  ( -4.017660918040594346E-17, 1.000000000000000000, 2.376309959284834438E-19 ) ) ;
#32989 = CARTESIAN_POINT ( 'NONE',  ( -20.83467972660109169, 65.95194780259438971, -5.016499999999999737 ) ) ;
#32990 = CARTESIAN_POINT ( 'NONE',  ( -22.21083362159536634, 150.4821223471089411, 0.6270836034604139186 ) ) ;
#32991 = CARTESIAN_POINT ( 'NONE',  ( 4.770677904581660300, 21.51973835935561041, 6.970347630165958819 ) ) ;
#32992 = CARTESIAN_POINT ( 'NONE',  ( 7.125042791937182152, 121.7184703992695773, 0.7630849752878294812 ) ) ;
#32993 = CARTESIAN_POINT ( 'NONE',  ( 0.3287531253414590626, 116.7093555017326452, -0.2203909396130737663 ) ) ;
#32994 = DIRECTION ( 'NONE',  ( -0.9998004120163609398, 0.000000000000000000, -0.01997839162482749689 ) ) ;
#32995 = CARTESIAN_POINT ( 'NONE',  ( -46.68567580513006732, 26.01863749727769104, 1.329804637746865081 ) ) ;
#32996 = CARTESIAN_POINT ( 'NONE',  ( -47.97936104919185851, 23.38005451144316993, 1.568716696360799912 ) ) ;
#32998 = EDGE_CURVE ( 'NONE', #18074, #3139, #4671, .T. ) ;
#32997 = CARTESIAN_POINT ( 'NONE',  ( -17.14500000000466784, 71.11999999999886768, 1.269999999999998241 ) ) ;
#32999 = CARTESIAN_POINT ( 'NONE',  ( -54.98111839650035648, 8.542840639972862249, 3.427624633821322320 ) ) ;
#33000 = CARTESIAN_POINT ( 'NONE',  ( -17.14500000000466784, 71.11999999999886768, -1.524000000000000909 ) ) ;
#33001 = CARTESIAN_POINT ( 'NONE',  ( -4.404930073839969928, 118.1622843756694010, 0.4910954181917899786 ) ) ;
#33002 = CARTESIAN_POINT ( 'NONE',  ( -5.237865101059587580, 78.94033958618261693, -5.314315937239334708 ) ) ;
#33003 = ORIENTED_EDGE ( 'NONE', *, *, #15761, .F. ) ;
#33004 = CARTESIAN_POINT ( 'NONE',  ( -46.52557095416602806, 23.25943309041075224, 3.047882326417268750 ) ) ;
#33005 = ADVANCED_FACE ( 'NONE', ( #27302 ), #19078, .T. ) ;
#33006 = CARTESIAN_POINT ( 'NONE',  ( 8.346771193436987701, 120.0109853342942472, -1.116703882779259027 ) ) ;
#33007 = CARTESIAN_POINT ( 'NONE',  ( -5.131660560486008826, 115.4810986995850755, -1.508144361588663829 ) ) ;
#33008 = CARTESIAN_POINT ( 'NONE',  ( 4.553093912424611922, 118.0135662636855756, 0.8850293724966483699 ) ) ;
#33009 = CARTESIAN_POINT ( 'NONE',  ( -14.07483374865171477, 150.3034377993741657, -1.364178037702375779 ) ) ;
#33010 = FACE_OUTER_BOUND ( 'NONE', #18299, .T. ) ;
#33011 = CARTESIAN_POINT ( 'NONE',  ( 4.709982941061709560, 118.1651004037422865, -0.4215969789121262190 ) ) ;
#33012 = CARTESIAN_POINT ( 'NONE',  ( 0.3655860903868409229, 105.8811906981200934, -5.329044222542315801 ) ) ;
#33013 = CARTESIAN_POINT ( 'NONE',  ( -10.36176036692648594, 123.5464890276372785, -1.327270239784479333 ) ) ;
#33014 = FACE_OUTER_BOUND ( 'NONE', #24505, .T. ) ;
#33015 = CARTESIAN_POINT ( 'NONE',  ( -0.003550340867792285433, 156.3099534201614631, 0.1776735749810083032 ) ) ;
#33016 = CARTESIAN_POINT ( 'NONE',  ( 8.044334902818746968, 121.4620208242424155, -0.8712540157607662206 ) ) ;
#33017 = CARTESIAN_POINT ( 'NONE',  ( -8.915496673695567864, 123.9583917734820915, -0.08963474529912127120 ) ) ;
#33018 = CARTESIAN_POINT ( 'NONE',  ( 0.7336086519982950582, 0.2932837538699786251, -4.563195415240439701 ) ) ;
#33019 = CARTESIAN_POINT ( 'NONE',  ( 10.56633813141740497, 157.9214973357695158, 0.8874509626871487367 ) ) ;
#33020 = DIRECTION ( 'NONE',  ( 9.627370216492862708E-17, 1.000000000000000000, -0.000000000000000000 ) ) ;
#33021 = CARTESIAN_POINT ( 'NONE',  ( 2.598075364112794716, -15.28479904474297513, 4.671545106743766773 ) ) ;
#33022 = CARTESIAN_POINT ( 'NONE',  ( -18.78841748004283119, 148.4604323410545987, 1.722921296925317369 ) ) ;
#33023 = CARTESIAN_POINT ( 'NONE',  ( 0.8462494346447723137, 11.68649857616015275, 0.4938625092760188795 ) ) ;
#33024 = CARTESIAN_POINT ( 'NONE',  ( -5.654702199549804575, 159.1134716836843381, -0.5125381600378308145 ) ) ;
#33025 = CARTESIAN_POINT ( 'NONE',  ( -0.8770832347484921465, 27.56386522087566249, 0.4220112102557041500 ) ) ;
#33026 = VERTEX_POINT ( 'NONE', #40317 ) ;
#33027 = CARTESIAN_POINT ( 'NONE',  ( -42.88395384449221126, 21.55219572468337219, 1.583305067638063779 ) ) ;
#33028 = CARTESIAN_POINT ( 'NONE',  ( 5.567295163420428850, 119.7830797108918688, 0.4963393297495872769 ) ) ;
#33029 = APPLICATION_PROTOCOL_DEFINITION ( 'draft international standard', 'automotive_design', 1998, #25946 ) ;
#33030 = AXIS2_PLACEMENT_3D ( 'NONE', #12097, #38092, #8907 ) ;
#33031 = CARTESIAN_POINT ( 'NONE',  ( -8.149220328376188149, 154.6259123219959690, 0.6607633090041664659 ) ) ;
#33032 = CARTESIAN_POINT ( 'NONE',  ( 4.057314763829551474, -13.83595378911055285, 4.182047561617943110 ) ) ;
#33033 = CARTESIAN_POINT ( 'NONE',  ( 5.120154531940189102, 120.2090573957402455, -0.7231840875875844565 ) ) ;
#33034 = CARTESIAN_POINT ( 'NONE',  ( 0.03256023585714045571, 157.9544661776888290, -1.629447346748784220 ) ) ;
#33035 = CARTESIAN_POINT ( 'NONE',  ( 4.761265771961571858, 104.6144662015457527, 0.8484901396519970440 ) ) ;
#33036 = CARTESIAN_POINT ( 'NONE',  ( 3.162461164278121739, -14.57801340048104777, 3.369881103115548893 ) ) ;
#33037 = CARTESIAN_POINT ( 'NONE',  ( -1.820350978615107751, 35.44831059284695129, 0.3018992756893350005 ) ) ;
#33038 = CARTESIAN_POINT ( 'NONE',  ( 15.54908666625160940, 147.5346097818530211, 0.08167737433607563657 ) ) ;
#33039 = ORIENTED_EDGE ( 'NONE', *, *, #1457, .F. ) ;
#33040 = CARTESIAN_POINT ( 'NONE',  ( -2.469273130011678141, 107.0255785817588645, 4.723498045142633828 ) ) ;
#33041 = CARTESIAN_POINT ( 'NONE',  ( -16.60960244842765832, 1.680552189788819435E-15, 0.000000000000000000 ) ) ;
#33042 = CARTESIAN_POINT ( 'NONE',  ( 4.801338745261147345, 117.3993836135855275, -1.016148444996444189 ) ) ;
#33043 = CARTESIAN_POINT ( 'NONE',  ( -17.14499999999999957, 71.11999999999999034, 5.016499999999999737 ) ) ;
#33044 = CARTESIAN_POINT ( 'NONE',  ( 2.769246990704956612, 116.5678055239024644, -0.05256187475617109944 ) ) ;
#33045 = CARTESIAN_POINT ( 'NONE',  ( -6.719914377344099243, 121.2247800624193133, 0.07397671124164069412 ) ) ;
#33046 = CARTESIAN_POINT ( 'NONE',  ( -2.812155987513873079, 118.7629491485454167, 1.088229539211323038 ) ) ;
#33047 = PLANE ( 'NONE',  #29156 ) ;
#33048 = CARTESIAN_POINT ( 'NONE',  ( -0.4217933310832886473, 35.81132274965050044, -0.2641305449634421820 ) ) ;
#33049 = CARTESIAN_POINT ( 'NONE',  ( 11.58753624721085984, 156.3395478113760362, 2.047021040405475389 ) ) ;
#33050 = CIRCLE ( 'NONE', #18070, 0.2539999999999960067 ) ;
#33051 = CARTESIAN_POINT ( 'NONE',  ( 3.724956840101937505, 21.94285949141939440, 2.734508905299370518 ) ) ;
#33052 = CARTESIAN_POINT ( 'NONE',  ( -7.980626778564171353, 22.53057930515566554, 2.691543149341120156 ) ) ;
#33053 = CARTESIAN_POINT ( 'NONE',  ( -8.615205574347543305, 118.4878503906377460, -1.080356039600459894 ) ) ;
#33054 = CARTESIAN_POINT ( 'NONE',  ( -1.788686868886097292, 120.9773948236336878, -0.4149341611056206469 ) ) ;
#33055 = CARTESIAN_POINT ( 'NONE',  ( -5.892673590944178308, 78.88814725119665638, 5.017439957471214740 ) ) ;
#33056 = FACE_BOUND ( 'NONE', #27176, .T. ) ;
#33057 = CARTESIAN_POINT ( 'NONE',  ( -3.166910920246462258, 104.6144662015195621, 4.306197946819769307 ) ) ;
#33058 = CARTESIAN_POINT ( 'NONE',  ( -4.636761822055341042, 12.60011390031314349, 0.2095705037016724059 ) ) ;
#33059 = DIRECTION ( 'NONE',  ( -5.188838149069471174E-16, 1.699382548006136313E-16, 1.000000000000000000 ) ) ;
#33060 = CYLINDRICAL_SURFACE ( 'NONE', #17822, 0.5080000000000000071 ) ;
#33061 = CARTESIAN_POINT ( 'NONE',  ( 2.681353593581013328, -14.83682625404381028, 4.634604895792218571 ) ) ;
#33062 = CARTESIAN_POINT ( 'NONE',  ( 1.397093717039300964, 113.6455945353133643, -2.337579097500038117 ) ) ;
#33063 = CARTESIAN_POINT ( 'NONE',  ( -0.005915287708768494392, 116.9295063353193882, 0.2960251855814710065 ) ) ;
#33064 = CARTESIAN_POINT ( 'NONE',  ( 4.901578213037685927, 117.4095775641370523, -0.9679565193343001583 ) ) ;
#33065 = EDGE_LOOP ( 'NONE', ( #4491, #5752, #38856, #30380 ) ) ;
#33066 = DIRECTION ( 'NONE',  ( -0.9454731675810326141, 0.3256999990547876367, -5.459396135145336213E-16 ) ) ;
#33067 = APPLICATION_CONTEXT ( 'automotive_design' ) ;
#33068 = ORIENTED_EDGE ( 'NONE', *, *, #31099, .F. ) ;
#33069 = DIRECTION ( 'NONE',  ( 0.9876665170007974393, -0.1565721916417901483, 8.537024980200831679E-16 ) ) ;
#33070 = CARTESIAN_POINT ( 'NONE',  ( 3.437591410214265064, -15.71306207096091789, 4.322042152151218453 ) ) ;
#33071 = CARTESIAN_POINT ( 'NONE',  ( -16.05265579080208482, 153.3736753708079732, 1.680156470693515036 ) ) ;
#33072 = CARTESIAN_POINT ( 'NONE',  ( 13.91986491619282873, 121.5005676099359846, -1.010465608187345321 ) ) ;
#33073 = CARTESIAN_POINT ( 'NONE',  ( -0.2409191691226134635, 30.52881386638012629, -0.9476172785465332149 ) ) ;
#33074 = CARTESIAN_POINT ( 'NONE',  ( -58.82991074935231524, -0.2577531494038359794, -1.058401375502683064E-14 ) ) ;
#33075 = ORIENTED_EDGE ( 'NONE', *, *, #33091, .F. ) ;
#33076 = DIRECTION ( 'NONE',  ( -9.627370216492862708E-17, -1.000000000000000000, 0.000000000000000000 ) ) ;
#33077 = CARTESIAN_POINT ( 'NONE',  ( -0.1065646865916382441, 105.8844662015457203, 5.332932678536313809 ) ) ;
#33078 = DIRECTION ( 'NONE',  ( -0.9998501190848636533, -0.01731298258487879230, 2.441448296158441227E-15 ) ) ;
#33079 = PRODUCT_DEFINITION_SHAPE ( 'NONE', 'NONE',  #26370 ) ;
#33080 = CARTESIAN_POINT ( 'NONE',  ( -12.96210878518750498, 128.4900567078429390, 1.108396809849303777 ) ) ;
#33081 = DIRECTION ( 'NONE',  ( -0.8745520943968245753, 0.4849315768086539524, -5.691349986800526185E-16 ) ) ;
#33082 = CARTESIAN_POINT ( 'NONE',  ( 17.94049195465762736, 148.7876888829155746, -1.661648619591604481 ) ) ;
#33083 = CARTESIAN_POINT ( 'NONE',  ( -4.065609891792139940, 118.4217611105734846, -0.9713962693593599651 ) ) ;
#33084 = CARTESIAN_POINT ( 'NONE',  ( -5.424023212060650856, 78.92586886208859198, 5.134886908577998454 ) ) ;
#33085 = ORIENTED_EDGE ( 'NONE', *, *, #30869, .F. ) ;
#33086 = CARTESIAN_POINT ( 'NONE',  ( 4.555104234677612496, 118.1072174076028034, -0.4957042797719007909 ) ) ;
#33087 = CARTESIAN_POINT ( 'NONE',  ( 15.56233417011314124, 148.0963874134046705, -0.5341686659567148610 ) ) ;
#33088 = AXIS2_PLACEMENT_3D ( 'NONE', #15837, #6274, #22013 ) ;
#33089 = ORIENTED_EDGE ( 'NONE', *, *, #17483, .F. ) ;
#33090 = CARTESIAN_POINT ( 'NONE',  ( 1.863517626568274910, -15.41251410767331720, 5.374852164437769808 ) ) ;
#33091 = EDGE_CURVE ( 'NONE', #37691, #8945, #11110, .T. ) ;
#33092 = DIRECTION ( 'NONE',  ( -0.8745520943968243532, 0.4849315768086547296, -5.361993529360573944E-16 ) ) ;
#33093 = CARTESIAN_POINT ( 'NONE',  ( -58.36720124622708994, -0.2861505079046616773, 0.06388190288942181827 ) ) ;
#33094 = CARTESIAN_POINT ( 'NONE',  ( 0.3254831797250597458, 1.427361272777448509, 4.610396533461925905 ) ) ;
#33095 = CARTESIAN_POINT ( 'NONE',  ( 17.50701641564904776, 146.6691408387931688, 2.165841098895501027 ) ) ;
#33096 = CARTESIAN_POINT ( 'NONE',  ( 2.842584213824973283, 37.57586378862247045, -0.09837489246507950813 ) ) ;
#33097 = EDGE_CURVE ( 'NONE', #30817, #7672, #13645, .T. ) ;
#33098 = CARTESIAN_POINT ( 'NONE',  ( 3.548611814566905664, 16.26088872207684943, 2.983771105379771971 ) ) ;
#33099 = CARTESIAN_POINT ( 'NONE',  ( 8.097005894254447611, 122.8525693413601800, 0.3074703907764579358 ) ) ;
#33100 = LINE ( 'NONE', #36709, #19498 ) ;
#33101 = CARTESIAN_POINT ( 'NONE',  ( -50.43530108972998960, 14.71354995532366594, -3.653486772774936053 ) ) ;
#33102 = CARTESIAN_POINT ( 'NONE',  ( -2.162143947430365643, 116.2986588195852420, -0.2515325357244250215 ) ) ;
#33103 = FACE_OUTER_BOUND ( 'NONE', #28833, .T. ) ;
#33104 = CARTESIAN_POINT ( 'NONE',  ( -46.93285886088614234, 25.18477106413915934, -1.854137101283168887 ) ) ;
#33105 = CARTESIAN_POINT ( 'NONE',  ( -5.525052883313952279, 65.71034362490503611, 1.270000000000004459 ) ) ;
#33106 = CARTESIAN_POINT ( 'NONE',  ( -29.43804252118301079, 67.00854438735578356, -1.269999999999767981 ) ) ;
#33107 = CARTESIAN_POINT ( 'NONE',  ( 2.958531772299235918, 50.42904571186020490, 1.329372033065076453 ) ) ;
#33108 = FACE_OUTER_BOUND ( 'NONE', #29744, .T. ) ;
#33109 = FACE_OUTER_BOUND ( 'NONE', #32026, .T. ) ;
#33110 = CARTESIAN_POINT ( 'NONE',  ( -58.40930376703802551, 1.028767233150276628, 0.4283228411258263035 ) ) ;
#33111 = TOROIDAL_SURFACE ( 'NONE', #26960, 0.3810000000000002829, 0.2540000000000000036 ) ;
#33112 = CARTESIAN_POINT ( 'NONE',  ( -55.73247374733729487, 5.492406230130003841, 2.854677165782097514 ) ) ;
#33113 = CARTESIAN_POINT ( 'NONE',  ( -22.60023854264601439, 150.6256779753201158, -0.001684207673826830986 ) ) ;
#33114 = AXIS2_PLACEMENT_3D ( 'NONE', #39336, #22482, #32519 ) ;
#33115 = ORIENTED_EDGE ( 'NONE', *, *, #14406, .T. ) ;
#33116 = CARTESIAN_POINT ( 'NONE',  ( -58.07447437077728125, 1.735896131820596766, -1.499107834811110873 ) ) ;
#33117 = CARTESIAN_POINT ( 'NONE',  ( -6.961417914879455715, 121.9448106840860504, -0.2443103574289700597 ) ) ;
#33118 = VERTEX_POINT ( 'NONE', #40931 ) ;
#33119 = CARTESIAN_POINT ( 'NONE',  ( 1.734723475976807094E-15, 17.14499999999999957, 0.000000000000000000 ) ) ;
#33120 = CARTESIAN_POINT ( 'NONE',  ( -8.053145991180288732, 122.8529229587361442, -0.1924930237977967862 ) ) ;
#33121 = CARTESIAN_POINT ( 'NONE',  ( 4.021138818454151220, -15.00176662281678475, 5.141887924562631440 ) ) ;
#33122 = CARTESIAN_POINT ( 'NONE',  ( -20.90199038452910685, 141.6159226613069109, 1.473829418026497251 ) ) ;
#33123 = CARTESIAN_POINT ( 'NONE',  ( 3.211436584971100849, 28.15539441671475274, -3.345526564039049688 ) ) ;
#33124 = CARTESIAN_POINT ( 'NONE',  ( 5.807154922825556120, 117.0096406922080376, 0.3504623104576318204 ) ) ;
#33125 = CARTESIAN_POINT ( 'NONE',  ( 11.71381910070873644, 130.2301003178167775, 0.4045216064884521456 ) ) ;
#33126 = CARTESIAN_POINT ( 'NONE',  ( 4.622858883031034871, 26.85595184169372374, 0.2084198311932836112 ) ) ;
#33127 = CARTESIAN_POINT ( 'NONE',  ( -0.1494942157332288524, 1.595350521021342782, -0.9636992805340545143 ) ) ;
#33128 = CARTESIAN_POINT ( 'NONE',  ( -9.776364138556823846, 118.0142902678875885, -0.3953848830946984361 ) ) ;
#33129 = LINE ( 'NONE', #10738, #31781 ) ;
#33130 = CARTESIAN_POINT ( 'NONE',  ( -11.56352105402813280, 78.55269139521317356, 1.270000000000000018 ) ) ;
#33131 = ORIENTED_EDGE ( 'NONE', *, *, #20419, .F. ) ;
#33132 = CARTESIAN_POINT ( 'NONE',  ( 5.530216759611570332, 117.0052764743229261, 0.6302382510017663364 ) ) ;
#33133 = CARTESIAN_POINT ( 'NONE',  ( -17.80491421350304648, 148.0643276405518804, 1.576192721057973145 ) ) ;
#33134 = CARTESIAN_POINT ( 'NONE',  ( -58.20606554041528824, 0.05853145357879600830, -0.5431157087058823274 ) ) ;
#33135 = CARTESIAN_POINT ( 'NONE',  ( 13.68454576465603800, 121.6032371815301900, 1.618700059879337294 ) ) ;
#33136 = CARTESIAN_POINT ( 'NONE',  ( 8.613587046216144572, 156.7723266660784986, -1.729508645372233033 ) ) ;
#33137 = CARTESIAN_POINT ( 'NONE',  ( -0.6334066649623988354, -12.81304641701132851, -0.7396855475671405555 ) ) ;
#33138 = CARTESIAN_POINT ( 'NONE',  ( -20.70408045738755831, 151.0745573368290593, -1.983427051661964535 ) ) ;
#33139 = VECTOR ( 'NONE', #27723, 1000.000000000000114 ) ;
#33140 = CARTESIAN_POINT ( 'NONE',  ( 4.664901767118291076, 118.0183831904404741, -0.6239428623521563466 ) ) ;
#33141 = CARTESIAN_POINT ( 'NONE',  ( 4.696425917957757434, 104.6144662015457243, 1.156094417919997674 ) ) ;
#33142 = ADVANCED_FACE ( 'NONE', ( #20893 ), #18119, .F. ) ;
#33143 = B_SPLINE_CURVE_WITH_KNOTS ( 'NONE', 1,
 ( #41898, #12697 ),
 .UNSPECIFIED., .F., .F.,
 ( 2, 2 ),
 ( 0.000000000000000000, 1.000000000000000000 ),
 .UNSPECIFIED. ) ;
#33144 = CARTESIAN_POINT ( 'NONE',  ( 9.968563030426308202, 123.7598584631124794, -0.7002966798862195752 ) ) ;
#33145 = CARTESIAN_POINT ( 'NONE',  ( -5.945776936743828678, 121.5465042053001667, -0.1188107733588233406 ) ) ;
#33146 = ORIENTED_EDGE ( 'NONE', *, *, #19781, .T. ) ;
#33147 = CARTESIAN_POINT ( 'NONE',  ( -11.57159210561028928, 122.7176759045101022, -1.727280539041415874 ) ) ;
#33148 = CARTESIAN_POINT ( 'NONE',  ( 3.970714270704740922, -15.74271870963887743, 3.976543152134710990 ) ) ;
#33149 = AXIS2_PLACEMENT_3D ( 'NONE', #16131, #32769, #29134 ) ;
#33150 = CARTESIAN_POINT ( 'NONE',  ( -11.41714695485569919, 57.14999999999997726, 5.016500000000000625 ) ) ;
#33151 = CARTESIAN_POINT ( 'NONE',  ( -4.642530418943314530, 118.0244946899635323, -0.7554534729805311155 ) ) ;
#33152 = CARTESIAN_POINT ( 'NONE',  ( -52.97391985390434144, 12.30611266682019789, -4.247241762254921227 ) ) ;
#33153 = VECTOR ( 'NONE', #26492, 1000.000000000000000 ) ;
#33154 = CARTESIAN_POINT ( 'NONE',  ( 4.065926199369043204, 118.2429491485453354, 0.3080910687088499467 ) ) ;
#33155 = CARTESIAN_POINT ( 'NONE',  ( 2.153957835384796127, 157.2504501563031738, 1.632675037709188537 ) ) ;
#33156 = CARTESIAN_POINT ( 'NONE',  ( -17.32429653712378936, 61.56493206124108042, -1.523999999999999355 ) ) ;
#33157 = CARTESIAN_POINT ( 'NONE',  ( 21.68875320759051917, 132.7412702629105468, 0.4333929054516008073 ) ) ;
#33158 = CARTESIAN_POINT ( 'NONE',  ( 7.077328715112659374, 6.763356510963684620, 4.580356461215433939 ) ) ;
#33159 = CARTESIAN_POINT ( 'NONE',  ( 9.577010982343992396, 124.1734284925964573, 0.7139017932201211503 ) ) ;
#33160 = CARTESIAN_POINT ( 'NONE',  ( 15.10519797802274056, 121.1899582252741112, -0.5359826722732081716 ) ) ;
#33161 = CARTESIAN_POINT ( 'NONE',  ( 5.322333424082418496, 105.1224784086732171, -0.3647577769771441769 ) ) ;
#33162 = VERTEX_POINT ( 'NONE', #14092 ) ;
#33163 = CARTESIAN_POINT ( 'NONE',  ( 0.9590485603908195378, 118.7629491485454025, 1.264668241433272833 ) ) ;
#33164 = TOROIDAL_SURFACE ( 'NONE', #37894, 2.286000000000000032, 0.2540000000000000036 ) ;
#33165 = ADVANCED_FACE ( 'NONE', ( #37513 ), #1547, .F. ) ;
#33166 = CARTESIAN_POINT ( 'NONE',  ( -21.60220573293495860, 132.6646020023713959, -0.2978857061057720856 ) ) ;
#33167 = ORIENTED_EDGE ( 'NONE', *, *, #10027, .T. ) ;
#33168 = CARTESIAN_POINT ( 'NONE',  ( -6.826600680103125818, 121.4509929031113131, -0.7999390687483252105 ) ) ;
#33169 = CYLINDRICAL_SURFACE ( 'NONE', #25786, 9.048749999999998295 ) ;
#33170 = CARTESIAN_POINT ( 'NONE',  ( -9.239529650026234719, 153.8817031120973411, -0.7017441744976310458 ) ) ;
#33171 = CARTESIAN_POINT ( 'NONE',  ( 3.936650548058306054, -12.34391569202568384, 1.586490187297609156 ) ) ;
#33172 = CARTESIAN_POINT ( 'NONE',  ( -22.09732278473127565, 146.2042277794223537, 1.157738048209833170 ) ) ;
#33173 = CARTESIAN_POINT ( 'NONE',  ( -41.06677624517575964, 23.07857903943748212, 1.269999999996107354 ) ) ;
#33174 = CARTESIAN_POINT ( 'NONE',  ( 1.421330246821746801, 159.6054662015457666, 0.04208995589191837083 ) ) ;
#33175 = VERTEX_POINT ( 'NONE', #34336 ) ;
#33176 = CARTESIAN_POINT ( 'NONE',  ( -3.594857975007920814, -7.703025367003809798, -2.923569511714296798 ) ) ;
#33177 = CARTESIAN_POINT ( 'NONE',  ( 0.5136544389551274126, 105.1227275070236686, 5.319539499184048559 ) ) ;
#33178 = DIRECTION ( 'NONE',  ( -0.9998501190848640974, -0.01731298258485272981, -8.537024980200786319E-16 ) ) ;
#33179 = CARTESIAN_POINT ( 'NONE',  ( 6.057513928997569685, 57.78500000000000369, 1.904999999999996030 ) ) ;
#33180 = CIRCLE ( 'NONE', #5296, 0.6350000000000014522 ) ;
#33181 = CARTESIAN_POINT ( 'NONE',  ( -4.496095910029399789, 118.6657657825083305, 0.8773962309065390652 ) ) ;
#33182 = EDGE_CURVE ( 'NONE', #33565, #25673, #1684, .T. ) ;
#33183 = CARTESIAN_POINT ( 'NONE',  ( -3.339653329301207840, -2.245917679271888900, -3.199182135983138053 ) ) ;
#33184 = CARTESIAN_POINT ( 'NONE',  ( 13.81631647976127120, 120.6843904051541898, 1.269697867868520014 ) ) ;
#33185 = CARTESIAN_POINT ( 'NONE',  ( -58.68272167409650564, -0.3140646606568653354, -0.3072153925272262387 ) ) ;
#33187 = CARTESIAN_POINT ( 'NONE',  ( 20.86711222142698929, 145.7124547906547889, -1.576573076165909360 ) ) ;
#33186 = DIRECTION ( 'NONE',  ( 0.9998004120163608288, 0.000000000000000000, 0.01997839162482736852 ) ) ;
#33188 = CARTESIAN_POINT ( 'NONE',  ( 0.3254831797250597458, 1.427361272777448509, 4.610396533461925905 ) ) ;
#33189 = CARTESIAN_POINT ( 'NONE',  ( -15.07172804838065261, 121.1899582252741112, -1.138989471373297535 ) ) ;
#33190 = ORIENTED_EDGE ( 'NONE', *, *, #17108, .F. ) ;
#33191 = CARTESIAN_POINT ( 'NONE',  ( -13.12764272666535526, 133.9996589410087324, 0.1750096343312400049 ) ) ;
#33192 = ADVANCED_FACE ( 'NONE', ( #40524 ), #31123, .F. ) ;
#33193 = CARTESIAN_POINT ( 'NONE',  ( 5.718287093813156474, -14.23487671053640113, 2.942044405997081391 ) ) ;
#33194 = DIRECTION ( 'NONE',  ( 0.9998004120163609398, 0.000000000000000000, 0.01997839162482749689 ) ) ;
#33195 = TOROIDAL_SURFACE ( 'NONE', #20910, 5.080000000000005400, 0.5080000000000000071 ) ;
#33196 = EDGE_CURVE ( 'NONE', #20421, #26517, #37309, .T. ) ;
#33197 = CARTESIAN_POINT ( 'NONE',  ( -5.184089659939317585, 115.9100003722667083, -1.325920433419026434 ) ) ;
#33198 = ORIENTED_EDGE ( 'NONE', *, *, #24135, .F. ) ;
#33199 = CARTESIAN_POINT ( 'NONE',  ( 17.10357040864152367, 151.3967157021085654, 2.430234537686704055 ) ) ;
#33200 = CARTESIAN_POINT ( 'NONE',  ( -8.265412277504241345, 72.86149316418863009, -1.523999999999996469 ) ) ;
#33201 = CARTESIAN_POINT ( 'NONE',  ( -31.81551635377703136, 53.03133741989296368, -1.270000000000005347 ) ) ;
#33202 = CARTESIAN_POINT ( 'NONE',  ( -5.427513099616406045, 158.9671755112622122, 0.8485680044740095962 ) ) ;
#33203 = CARTESIAN_POINT ( 'NONE',  ( 3.560122487986403517, 2.076091768892780909, 7.630420683349803390 ) ) ;
#33204 = CARTESIAN_POINT ( 'NONE',  ( 16.46997841215771530, 146.2355833862463328, 1.608729380348347782 ) ) ;
#33205 = ADVANCED_FACE ( 'NONE', ( #8125 ), #16055, .T. ) ;
#33206 = CARTESIAN_POINT ( 'NONE',  ( 0.004913308685965686075, 116.7872217978203224, -0.2458820580207658757 ) ) ;
#33207 = CARTESIAN_POINT ( 'NONE',  ( 9.132817075745611705E-16, 9.026346327358515609, 0.000000000000000000 ) ) ;
#33208 = CARTESIAN_POINT ( 'NONE',  ( -57.66147120254575498, 1.236620361205436502, 1.243523781513556914 ) ) ;
#33209 = CARTESIAN_POINT ( 'NONE',  ( -47.36536141536632982, 24.59964078100214380, 1.062456689557159439 ) ) ;
#33210 = CARTESIAN_POINT ( 'NONE',  ( -4.713276526765134200, 118.1588900175951977, 0.4357070110130277785 ) ) ;
#33211 = CARTESIAN_POINT ( 'NONE',  ( -54.97180548219925100, 8.422794459035404913, 3.467293221275778325 ) ) ;
#33212 = CARTESIAN_POINT ( 'NONE',  ( -56.97070633664897343, 3.259530599714575150, 2.205540024717516090 ) ) ;
#33213 = CARTESIAN_POINT ( 'NONE',  ( -4.555299138033702455, 118.1072373763005032, 0.4955848589101189972 ) ) ;
#33214 = DIRECTION ( 'NONE',  ( 5.188838149069472160E-16, -1.699382548006136559E-16, -1.000000000000000000 ) ) ;
#33215 = EDGE_LOOP ( 'NONE', ( #31630, #30118, #34388, #892 ) ) ;
#33216 = CARTESIAN_POINT ( 'NONE',  ( -45.91718695868514288, 25.22619731686664224, 1.578102078770057037 ) ) ;
#33217 = CARTESIAN_POINT ( 'NONE',  ( 6.090059827715747609, 119.4132085878391223, -1.021381826822683303 ) ) ;
#33218 = CARTESIAN_POINT ( 'NONE',  ( -3.430439322123234991, 108.6576027043044377, -4.130303871225995849 ) ) ;
#33219 = CARTESIAN_POINT ( 'NONE',  ( 4.531728878287003326, 118.1072486390968379, 0.6773096721064315595 ) ) ;
#33220 = CARTESIAN_POINT ( 'NONE',  ( -12.31319552751079449, 152.0262389575480881, -1.296791798139146801 ) ) ;
#33221 = COLOUR_RGB ( '', 0.66274510, 0.83137255, 0.94901961) ;
#33222 = CARTESIAN_POINT ( 'NONE',  ( 0.000000000000000000, 0.000000000000000000, 0.000000000000000000 ) ) ;
#33223 = CARTESIAN_POINT ( 'NONE',  ( 2.802571055147052626, 117.9496044482589951, -1.216643114892233868 ) ) ;
#33224 = CARTESIAN_POINT ( 'NONE',  ( 3.100166793870271498, 107.8178375082508609, -4.356447870432107905 ) ) ;
#33225 = EDGE_CURVE ( 'NONE', #21005, #22572, #8338, .T. ) ;
#33226 = CARTESIAN_POINT ( 'NONE',  ( 0.008308630153154609663, 120.0570981805881559, -0.4157978282972238371 ) ) ;
#33227 = CARTESIAN_POINT ( 'NONE',  ( -5.329475387727676150, 116.0444662015457311, -0.2797177882896795809 ) ) ;
#33228 = DIRECTION ( 'NONE',  ( 1.224646799147353207E-16, 7.780346281855952181E-32, 1.000000000000000000 ) ) ;
#33229 = CARTESIAN_POINT ( 'NONE',  ( 8.561575482294122352, 118.9452303826420092, -0.9294693558782792797 ) ) ;
#33230 = CARTESIAN_POINT ( 'NONE',  ( -10.39299036940601439, 153.1602481698635643, -0.02716054506326659457 ) ) ;
#33231 = CARTESIAN_POINT ( 'NONE',  ( 4.928175349042589026, 117.6470996705704124, 0.8667669811659319823 ) ) ;
#33232 = CARTESIAN_POINT ( 'NONE',  ( 11.39485104697103779, 118.9229013597968247, 0.8408094927682292496 ) ) ;
#33233 = FACE_OUTER_BOUND ( 'NONE', #28349, .T. ) ;
#33234 = CARTESIAN_POINT ( 'NONE',  ( 1.853042888461218007, -15.33088210119805339, 5.380378780177352382 ) ) ;
#33235 = CARTESIAN_POINT ( 'NONE',  ( -2.387896358646931283, 119.0637060312156024, 0.6953999086667947971 ) ) ;
#33236 = CARTESIAN_POINT ( 'NONE',  ( 0.9553521702984651975, -6.993735180969975929, 0.1873809170862112405 ) ) ;
#33237 = CARTESIAN_POINT ( 'NONE',  ( -18.29650779608106603, 125.1624627582897915, -0.9465853942869045801 ) ) ;
#33238 = CARTESIAN_POINT ( 'NONE',  ( 0.7743132463278736832, -9.628960163071635492, -0.5975928149734356376 ) ) ;
#33239 = EDGE_LOOP ( 'NONE', ( #10597, #10727, #19645, #37197 ) ) ;
#33240 = CARTESIAN_POINT ( 'NONE',  ( -41.90039389258884484, 22.27519970079744382, 1.481527307957004602 ) ) ;
#33241 = CARTESIAN_POINT ( 'NONE',  ( 3.889650775106587854, 109.8300753404742096, 3.673692233826463482 ) ) ;
#33242 = CARTESIAN_POINT ( 'NONE',  ( -16.17919469456376902, 146.7365623387580342, 0.6462428564100395345 ) ) ;
#33243 = CARTESIAN_POINT ( 'NONE',  ( 4.475827780916731946, -13.19141740729908108, 3.156716699630707890 ) ) ;
#33244 = CARTESIAN_POINT ( 'NONE',  ( 9.186197600956422349, 155.0058477609193801, -1.458900829815475975 ) ) ;
#33245 = CARTESIAN_POINT ( 'NONE',  ( -5.836180790127460050, 119.4106843418347950, -1.193569107438471333 ) ) ;
#33246 = CARTESIAN_POINT ( 'NONE',  ( -3.966471220580447987, 104.6144662015457811, 2.768186473522256108 ) ) ;
#33247 = EDGE_CURVE ( 'NONE', #28135, #7084, #18327, .T. ) ;
#33248 = CARTESIAN_POINT ( 'NONE',  ( 3.047801963512828394, -14.61332798263154054, 3.862229702996769376 ) ) ;
#33249 = CARTESIAN_POINT ( 'NONE',  ( -4.773210155766332008, 117.5405312103193438, -1.172205701249354304 ) ) ;
#33250 = CARTESIAN_POINT ( 'NONE',  ( 10.43234786055276686, 153.0845720789597522, 0.001036074960337154093 ) ) ;
#33251 = EDGE_LOOP ( 'NONE', ( #33003, #31730, #10578, #27600 ) ) ;
#33252 = CARTESIAN_POINT ( 'NONE',  ( 12.21488373879589240, 17.14499999999999957, -4.381499999999999950 ) ) ;
#33253 = CARTESIAN_POINT ( 'NONE',  ( -6.589702033682734540E-14, 87.97746620154572383, -4.338478393988997516E-18 ) ) ;
#33254 = CARTESIAN_POINT ( 'NONE',  ( -6.654617103318593247E-14, 104.6144662015457243, 1.534725424433578570E-31 ) ) ;
#33255 = CARTESIAN_POINT ( 'NONE',  ( -17.09258512000246100, 84.17916046765628835, -1.524000000000002908 ) ) ;
#33256 = CARTESIAN_POINT ( 'NONE',  ( 18.63219679753382962, 154.1293031355326946, 0.2996243416495531497 ) ) ;
#33257 = CIRCLE ( 'NONE', #37324, 0.5080000000000000071 ) ;
#33258 = CARTESIAN_POINT ( 'NONE',  ( -3.100166793870399840, 107.8178375082508609, 4.356447870432107905 ) ) ;
#33259 = AXIS2_PLACEMENT_3D ( 'NONE', #15234, #18638, #34421 ) ;
#33260 = CARTESIAN_POINT ( 'NONE',  ( 2.060254573934078515, -15.43196230555739312, 5.989929398572627406 ) ) ;
#33261 = CARTESIAN_POINT ( 'NONE',  ( -3.148524768479886937, 30.89467502894793327, -0.4672404312464801812 ) ) ;
#33262 = CARTESIAN_POINT ( 'NONE',  ( -3.346823384277141766, 31.23146344785865480, -0.04602645998765462348 ) ) ;
#33263 = CARTESIAN_POINT ( 'NONE',  ( 20.40332572169740288, 149.1468970683199586, 2.432323357318189050 ) ) ;
#33264 = ORIENTED_EDGE ( 'NONE', *, *, #38528, .T. ) ;
#33265 = CARTESIAN_POINT ( 'NONE',  ( 4.103208822911150300, 18.85939590645278585, -7.354229849909827088 ) ) ;
#33266 = CARTESIAN_POINT ( 'NONE',  ( -5.478737692705611728, 117.5010888497598103, -0.9448662039476222185 ) ) ;
#33267 = CARTESIAN_POINT ( 'NONE',  ( -1.644890720626135172, 119.8612358676174949, -0.5912986496483324528 ) ) ;
#33268 = CARTESIAN_POINT ( 'NONE',  ( 6.349999999999963229, 57.78500000000000369, 0.000000000000000000 ) ) ;
#33269 = CYLINDRICAL_SURFACE ( 'NONE', #22891, 9.048749999999998295 ) ;
#33270 = CARTESIAN_POINT ( 'NONE',  ( -8.744179778605065678, 67.99101067706818924, 1.270000000000003348 ) ) ;
#33271 = CARTESIAN_POINT ( 'NONE',  ( 3.746277899330032302, -0.8937244826341392834, -2.755274729908455900 ) ) ;
#33272 = DIRECTION ( 'NONE',  ( 0.8745520943968243532, -0.4849315768086547296, 6.829619984160642269E-16 ) ) ;
#33273 = CARTESIAN_POINT ( 'NONE',  ( -4.855449335888874174, 115.6909491485453003, 1.281272725539408297 ) ) ;
#33274 = CARTESIAN_POINT ( 'NONE',  ( 2.976679874252225577, -13.20894259333504905, 0.9412263588231246647 ) ) ;
#33275 = CARTESIAN_POINT ( 'NONE',  ( 3.568793996893895315, 120.2162445758188056, -0.3416935720284703937 ) ) ;
#33276 = CARTESIAN_POINT ( 'NONE',  ( -0.01133159106151501033, 159.5297144918048673, 0.5670791535570577357 ) ) ;
#33277 = DIRECTION ( 'NONE',  ( 0.3256999990547836399, 0.9454731675810339464, 0.000000000000000000 ) ) ;
#33278 = CARTESIAN_POINT ( 'NONE',  ( -8.428339483816529309, 74.57444062528223583, -1.269999999999996909 ) ) ;
#33279 =( BOUNDED_SURFACE ( )  B_SPLINE_SURFACE ( 3, 2, ( 
 ( #30907, #1117, #18111 ),
 ( #37102, #17904, #14705 ),
 ( #8330, #4525, #17489 ),
 ( #40095, #21300, #4323 ),
 ( #7920, #17691, #20886 ),
 ( #27508, #7716, #14286 ),
 ( #34117, #8119, #33910 ),
 ( #17286, #4944, #11309 ),
 ( #1746, #20679, #10682 ),
 ( #30276, #4738, #31116 ),
 ( #30690, #27710, #30485 ),
 ( #1328, #40719, #5157 ),
 ( #11514, #34328, #24091 ),
 ( #1540, #36683, #40517 ),
 ( #27295, #33704, #40310 ),
 ( #1953, #26877, #7505 ),
 ( #11103, #37302, #20464 ),
 ( #12370, #25561, #15755 ),
 ( #15124, #41137, #37932 ),
 ( #24934, #28344, #12574 ),
 ( #41562, #5572, #19164 ),
 ( #28760, #18739, #24718 ),
 ( #15339, #2165, #34538 ),
 ( #38565, #38362, #6195 ),
 ( #25147, #28554, #2592 ),
 ( #2379, #8964, #22134 ),
 ( #21932, #41353, #5364 ),
 ( #25358, #31749, #5990 ),
 ( #40923, #18319, #31321 ),
 ( #15552, #28127, #21505 ),
 ( #18953, #32168, #18530 ),
 ( #34741, #9177, #35163 ),
 ( #34961, #11943, #31959 ),
 ( #8755, #9378, #37722 ),
 ( #12155, #2798, #14913 ),
 ( #41773, #21717, #38151 ),
 ( #11729, #31535, #22342 ),
 ( #35365, #5784, #27917 ),
 ( #8546, #22760, #12983 ),
 ( #654, #9792, #29607 ),
 ( #7247, #35793, #29815 ),
 ( #12776, #16166, #3417 ) ),
 .UNSPECIFIED., .F., .F., .T. ) 
 B_SPLINE_SURFACE_WITH_KNOTS ( ( 4, 2, 2, 2, 2, 2, 2, 2, 2, 2, 2, 2, 2, 2, 2, 2, 2, 2, 2, 2, 4 ),
 ( 3, 3 ),
 ( 0.000000000000000000, 0.0009429120494251018838, 0.001414368074137652880, 0.001885824098850203768, 0.002828736148275305760, 0.003771648197700407535, 0.004714560247125509744, 0.005186016271838060632, 0.005657472296550611519, 0.006600384345975713295, 0.007543296395400815070, 0.008486208444825917713, 0.009429120494251019488, 0.009900576518963571243, 0.01037203254367612126, 0.01131494459310122304, 0.01225785664252632481, 0.01272931266723887483, 0.01320076869195142659, 0.01414368074137652836, 0.01508659279080163014 ),
 ( 0.000000000000000000, 1.000000000000000000 ),
 .UNSPECIFIED. ) 
 GEOMETRIC_REPRESENTATION_ITEM ( )  RATIONAL_B_SPLINE_SURFACE ( (
 ( 1.000000000000000000, 0.7071103834195795468, 1.000000000000000000),
 ( 1.000000000000000000, 0.7071124051442869707, 1.000000000000000000),
 ( 1.000000000000000000, 0.7070849312894228467, 1.000000000000000000),
 ( 1.000000000000000000, 0.7071123019286037481, 1.000000000000000000),
 ( 1.000000000000000000, 0.7071614862087763909, 1.000000000000000000),
 ( 1.000000000000000000, 0.7073010037706329856, 1.000000000000000000),
 ( 1.000000000000000000, 0.7073901506915791781, 1.000000000000000000),
 ( 1.000000000000000000, 0.7076394263844208998, 1.000000000000000000),
 ( 1.000000000000000000, 0.7077756853797776415, 1.000000000000000000),
 ( 1.000000000000000000, 0.7077567304198957299, 1.000000000000000000),
 ( 1.000000000000000000, 0.7075957674067504533, 1.000000000000000000),
 ( 1.000000000000000000, 0.7070041386104982672, 1.000000000000000000),
 ( 1.000000000000000000, 0.7065667128226251759, 1.000000000000000000),
 ( 1.000000000000000000, 0.7061037264541912828, 1.000000000000000000),
 ( 1.000000000000000000, 0.7059795971604051479, 1.000000000000000000),
 ( 1.000000000000000000, 0.7058187053605305961, 1.000000000000000000),
 ( 1.000000000000000000, 0.7057806473396187608, 1.000000000000000000),
 ( 1.000000000000000000, 0.7057897566527251421, 1.000000000000000000),
 ( 1.000000000000000000, 0.7059679295365862695, 1.000000000000000000),
 ( 1.000000000000000000, 0.7064617003595946576, 1.000000000000000000),
 ( 1.000000000000000000, 0.7067673356939784268, 1.000000000000000000),
 ( 1.000000000000000000, 0.7071356715510913604, 1.000000000000000000),
 ( 1.000000000000000000, 0.7071413527495709062, 1.000000000000000000),
 ( 1.000000000000000000, 0.7067748178510451229, 1.000000000000000000),
 ( 1.000000000000000000, 0.7064655642066967056, 1.000000000000000000),
 ( 1.000000000000000000, 0.7060874411990923916, 1.000000000000000000),
 ( 1.000000000000000000, 0.7059745403824593257, 1.000000000000000000),
 ( 1.000000000000000000, 0.7058136453788583786, 1.000000000000000000),
 ( 1.000000000000000000, 0.7057652904070991218, 1.000000000000000000),
 ( 1.000000000000000000, 0.7057433926758498455, 1.000000000000000000),
 ( 1.000000000000000000, 0.7059038550872894779, 1.000000000000000000),
 ( 1.000000000000000000, 0.7065143984468699179, 1.000000000000000000),
 ( 1.000000000000000000, 0.7069574456150055086, 1.000000000000000000),
 ( 1.000000000000000000, 0.7074174870072401644, 1.000000000000000000),
 ( 1.000000000000000000, 0.7075394654349829171, 1.000000000000000000),
 ( 1.000000000000000000, 0.7077084337036048112, 1.000000000000000000),
 ( 1.000000000000000000, 0.7077551412959035559, 1.000000000000000000),
 ( 1.000000000000000000, 0.7077863613254063990, 1.000000000000000000),
 ( 1.000000000000000000, 0.7076589125939298786, 1.000000000000000000),
 ( 1.000000000000000000, 0.7073336049174636653, 1.000000000000000000),
 ( 1.000000000000000000, 0.7071402517120219944, 1.000000000000000000),
 ( 1.000000000000000000, 0.7071072175333811272, 1.000000000000000000) ) ) 
 REPRESENTATION_ITEM ( '' )  SURFACE ( )  );
#33280 = VERTEX_POINT ( 'NONE', #22141 ) ;
#33281 = CARTESIAN_POINT ( 'NONE',  ( -1.606566256928685599, 32.19982401495065716, 1.077694121983207021 ) ) ;
#33282 = CARTESIAN_POINT ( 'NONE',  ( 5.240434970354078459, -15.39321860721029545, 1.015353449650246764 ) ) ;
#33283 = CARTESIAN_POINT ( 'NONE',  ( -19.78169998575278044, 149.7343351798865285, 1.666391814173802999 ) ) ;
#33284 = CARTESIAN_POINT ( 'NONE',  ( -2.983771112188844832, -5.329111280313512999, 3.548611825089460048 ) ) ;
#33285 = CARTESIAN_POINT ( 'NONE',  ( -58.62772660637192956, -0.2868617839840607586, -0.3825110252948605849 ) ) ;
#33286 = ORIENTED_EDGE ( 'NONE', *, *, #39881, .T. ) ;
#33287 = CARTESIAN_POINT ( 'NONE',  ( -11.56352105402813280, 78.55269139521317356, -1.523999999999999133 ) ) ;
#33288 = CARTESIAN_POINT ( 'NONE',  ( 1.009032787325873537, 123.9312678891798640, 0.1103529103309999343 ) ) ;
#33289 = SURFACE_SIDE_STYLE ('',( #10485 ) ) ;
#33290 = CARTESIAN_POINT ( 'NONE',  ( -5.875224328284241793, 120.7327493588883840, 0.6546335550538251447 ) ) ;
#33291 = CARTESIAN_POINT ( 'NONE',  ( 3.841735362705627210, 118.0214076499569700, 0.9713319504342076138 ) ) ;
#33292 = VECTOR ( 'NONE', #20713, 1000.000000000000114 ) ;
#33293 = CARTESIAN_POINT ( 'NONE',  ( 18.09865239071504206, 149.0664087073519681, -1.700023788287825299 ) ) ;
#33294 = CLOSED_SHELL ( 'NONE', ( #35232, #9267, #23652, #8998, #4644, #12567, #12595, #4214, #920, #23538, #3678, #26093, #5885, #36559, #2767, #306, #12100, #16975, #29731, #12360, #36744, #25533, #12412, #21950, #27841, #5168, #33672, #32148, #37116, #28524, #34175, #10285, #8168, #25608, #14441, #27628, #28689, #10287, #24367, #6545, #14803, #29197, #41210, #3379, #21687, #934, #23732, #17771, #16466, #38714, #22743, #36229, #19568, #29533, #8225, #12331, #31040, #13648, #17592, #39749, #1910, #38112, #29796, #17824, #16041, #3806, #14512, #24494, #19593, #9910, #8901, #5939, #12695, #22913, #21643, #18773, #14215, #20166, #23238, #11734, #35031, #1727, #18651, #15668, #884, #14166, #17830, #8261, #16468, #42011, #21967, #12066, #38905, #14678, #24762, #22999, #23691, #39348, #14311, #1132, #17555, #36361, #31620, #28133, #9811, #41422, #14680, #28186, #14090, #15695, #23530, #3225, #4300, #34697, #19074 ) ) ;
#33295 = CARTESIAN_POINT ( 'NONE',  ( -12.86454329319610856, 121.9120276846612256, -1.753115191834736963 ) ) ;
#33296 = FACE_OUTER_BOUND ( 'NONE', #16691, .T. ) ;
#33297 = ORIENTED_EDGE ( 'NONE', *, *, #36608, .F. ) ;
#33298 = CARTESIAN_POINT ( 'NONE',  ( 4.239670762977913121, 118.2238228529691213, -0.3214580067528489682 ) ) ;
#33299 = CARTESIAN_POINT ( 'NONE',  ( 8.072651008563752839, 154.6119571123129788, -0.5584669891872421355 ) ) ;
#33300 = ORIENTED_EDGE ( 'NONE', *, *, #2888, .T. ) ;
#33301 = CARTESIAN_POINT ( 'NONE',  ( 3.009962208777686499, -14.98531826913061771, 3.912431539232285704 ) ) ;
#33302 = CARTESIAN_POINT ( 'NONE',  ( 4.023522443498899648, 105.1224988529233144, -3.517836912119111314 ) ) ;
#33303 = CARTESIAN_POINT ( 'NONE',  ( -0.3558933743640902425, 1.202427940091101100, 4.626034787239965418 ) ) ;
#33304 = CARTESIAN_POINT ( 'NONE',  ( 9.709460118793433736, 122.6450757329969434, 1.337221984871323821 ) ) ;
#33305 = CARTESIAN_POINT ( 'NONE',  ( 2.944445591501515747, 38.71711244820894393, 0.2891746879855487395 ) ) ;
#33306 = CARTESIAN_POINT ( 'NONE',  ( 4.573446973487649281, 17.56025517495590904, -0.6989348988664985107 ) ) ;
#33307 = CARTESIAN_POINT ( 'NONE',  ( 15.39298062464833450, 147.8297367799732456, 0.5361660792469027381 ) ) ;
#33308 = CARTESIAN_POINT ( 'NONE',  ( -2.872265077263356226, 44.28946620154572855, -5.646510212151727437 ) ) ;
#33309 = AXIS2_PLACEMENT_3D ( 'NONE', #22466, #35497, #19290 ) ;
#33310 = CARTESIAN_POINT ( 'NONE',  ( -50.29507671575589001, 15.72791930032348873, -4.796563717952116335 ) ) ;
#33311 = CARTESIAN_POINT ( 'NONE',  ( 8.797613110180989793, 117.6982703817063367, 0.05471292246626040245 ) ) ;
#33312 = CARTESIAN_POINT ( 'NONE',  ( 1.421603664355671315, 159.6054662015457666, 0.02840702444251847966 ) ) ;
#33313 = CARTESIAN_POINT ( 'NONE',  ( -17.14499999999999957, 71.11999999999999034, 5.714999999999998082 ) ) ;
#33314 = CARTESIAN_POINT ( 'NONE',  ( -6.451606698686837575E-14, 65.62546620154573418, 4.217636114931141265E-29 ) ) ;
#33315 = CARTESIAN_POINT ( 'NONE',  ( -30.55042969354924765, 56.28656473928203496, -1.524000000000195421 ) ) ;
#33316 = CARTESIAN_POINT ( 'NONE',  ( -5.475330206976867231, 53.58606250000000415, 5.107412922131463695 ) ) ;
#33317 = CARTESIAN_POINT ( 'NONE',  ( -46.78334400223545231, 25.31617564245998508, 1.751383154100511597 ) ) ;
#33318 = FACE_OUTER_BOUND ( 'NONE', #38680, .T. ) ;
#33319 = CARTESIAN_POINT ( 'NONE',  ( -58.05614784158871799, 2.052449344323428626, 0.2046694337772680672 ) ) ;
#33320 = CARTESIAN_POINT ( 'NONE',  ( 0.01180776361637191768, 120.3637084677655764, -0.5909087754570011564 ) ) ;
#33321 = CARTESIAN_POINT ( 'NONE',  ( -5.699072711719833428, 159.1209727096294273, 0.1881040421785058481 ) ) ;
#33322 = ORIENTED_EDGE ( 'NONE', *, *, #20858, .T. ) ;
#33323 = CARTESIAN_POINT ( 'NONE',  ( -57.92473815682701144, 2.127617342915319565, -1.480748064241608430 ) ) ;
#33324 = CARTESIAN_POINT ( 'NONE',  ( 7.792635189458867906, 122.6008994260911891, 0.03648374067325547282 ) ) ;
#33325 = ORIENTED_EDGE ( 'NONE', *, *, #6096, .T. ) ;
#33326 = CARTESIAN_POINT ( 'NONE',  ( -8.798071503382049130, 117.6842349159514640, -0.1758064068840608507 ) ) ;
#33327 = CARTESIAN_POINT ( 'NONE',  ( 0.001367086239699496575, 156.3041635968983485, -0.06841458569046195148 ) ) ;
#33328 = CARTESIAN_POINT ( 'NONE',  ( 2.293780832555937010, -15.47183500671027367, 5.912194120686782739 ) ) ;
#33329 = CARTESIAN_POINT ( 'NONE',  ( -21.18042260023744205, 148.1333099715771766, 1.515480231459294336 ) ) ;
#33330 = CARTESIAN_POINT ( 'NONE',  ( 1.580769961479467911, 28.79261460129497863, -4.363931058323818668 ) ) ;
#33331 = CARTESIAN_POINT ( 'NONE',  ( 4.764559463231916148, 116.8420656028321218, 0.3170442335454677907 ) ) ;
#33332 = CARTESIAN_POINT ( 'NONE',  ( 2.224323458635174777, -15.45660113867128338, 5.869303334135124395 ) ) ;
#33333 = CARTESIAN_POINT ( 'NONE',  ( 2.332027132427558769, 25.33165720878049498, 3.998286310156994983 ) ) ;
#33334 = CARTESIAN_POINT ( 'NONE',  ( -0.3677562164248854293, -4.027846162062824753, 0.9036657059391408620 ) ) ;
#33335 = CARTESIAN_POINT ( 'NONE',  ( -0.9228193675735004708, 116.5712332538976455, -0.1866785551396778486 ) ) ;
#33336 = CARTESIAN_POINT ( 'NONE',  ( -7.213960532367465817, 78.77618639008778700, -1.904999999999999583 ) ) ;
#33337 = CARTESIAN_POINT ( 'NONE',  ( 4.937305977349591757, 117.4065427751604460, 1.082467720437599645 ) ) ;
#33338 = ORIENTED_EDGE ( 'NONE', *, *, #12282, .F. ) ;
#33339 = CARTESIAN_POINT ( 'NONE',  ( -2.194728688019693674, 116.2160623166575277, 0.009134385426443037206 ) ) ;
#33340 = CARTESIAN_POINT ( 'NONE',  ( -16.80660261901795849, 149.5530097695598215, 1.582604632240843801 ) ) ;
#33341 = CARTESIAN_POINT ( 'NONE',  ( -57.98023336920307003, 0.5472916609800171361, -0.8843171072923534659 ) ) ;
#33342 = CARTESIAN_POINT ( 'NONE',  ( 4.922209265113101750, 118.1424809852657773, 0.9875327093606014461 ) ) ;
#33343 = CARTESIAN_POINT ( 'NONE',  ( 3.262238196373776766, 118.8118204130220903, -0.7766580032327176086 ) ) ;
#33344 = CARTESIAN_POINT ( 'NONE',  ( -0.7500621227288748472, -10.43934603300536956, 0.6214162388253807734 ) ) ;
#33345 = CARTESIAN_POINT ( 'NONE',  ( -7.877908914988320355, 118.7344292658239340, -1.218006232967851377 ) ) ;
#33346 = CARTESIAN_POINT ( 'NONE',  ( -42.34481381083929818, 23.19759442052183473, -1.554397948409621755 ) ) ;
#33347 = CARTESIAN_POINT ( 'NONE',  ( 4.970465051853945937, 104.6144662015435642, 1.943362965483819593 ) ) ;
#33348 = AXIS2_PLACEMENT_3D ( 'NONE', #28980, #36022, #41796 ) ;
#33349 = CARTESIAN_POINT ( 'NONE',  ( 16.53085885483072559, 146.5532241433796230, -0.9478179252731553373 ) ) ;
#33350 = CARTESIAN_POINT ( 'NONE',  ( -15.64207015331068185, 147.2204672151589193, -0.3125657877211906466 ) ) ;
#33351 = ORIENTED_EDGE ( 'NONE', *, *, #20338, .F. ) ;
#33352 = CARTESIAN_POINT ( 'NONE',  ( -18.59210649535975435, 147.7499600834086948, -2.443498639627971869 ) ) ;
#33353 = CARTESIAN_POINT ( 'NONE',  ( 5.113606203424133412, -15.47995924129362599, 1.801594979316981204 ) ) ;
#33354 = CARTESIAN_POINT ( 'NONE',  ( -24.24369025645184905, 82.02711331519694227, -1.270000000000006457 ) ) ;
#33355 = CARTESIAN_POINT ( 'NONE',  ( -4.659430783399328035, 117.9638225107766800, -0.9016972064179303858 ) ) ;
#33356 = CARTESIAN_POINT ( 'NONE',  ( -49.01671973967521012, 18.67808020721676954, -5.174630477995056488 ) ) ;
#33357 = DIRECTION ( 'NONE',  ( -0.8572391118119521147, -0.5149185422762083686, 1.001946476563074719E-16 ) ) ;
#33358 = CARTESIAN_POINT ( 'NONE',  ( 7.396903380747357204, 120.6159063994810055, 1.271367681336521782 ) ) ;
#33359 = CARTESIAN_POINT ( 'NONE',  ( -3.328555392133318858, 33.88165127674241717, 1.160568618710268618 ) ) ;
#33360 = CARTESIAN_POINT ( 'NONE',  ( 16.17587344042694397, 121.2571949256804089, 0.3060957306870976113 ) ) ;
#33361 = CARTESIAN_POINT ( 'NONE',  ( -4.329333532990936817, 10.85900946394830413, -7.254296797256971630 ) ) ;
#33362 = CARTESIAN_POINT ( 'NONE',  ( 8.259016884198906894, 122.7564308547279666, 0.6276379194545153029 ) ) ;
#33363 = CARTESIAN_POINT ( 'NONE',  ( 22.10675755583028490, 150.4421090420883900, -0.7299123522449002532 ) ) ;
#33364 = CARTESIAN_POINT ( 'NONE',  ( -41.35619903644352036, 22.77303286471995136, -1.271070091490047238 ) ) ;
#33365 = AXIS2_PLACEMENT_3D ( 'NONE', #12228, #25633, #38643 ) ;
#33366 = CARTESIAN_POINT ( 'NONE',  ( 3.682264917456191888, 104.6144662015457243, 0.07358041635424013294 ) ) ;
#33367 = CARTESIAN_POINT ( 'NONE',  ( -9.815320032040085962, 117.9943556427423488, -0.1502691370658184589 ) ) ;
#33368 = ORIENTED_EDGE ( 'NONE', *, *, #5064, .F. ) ;
#33369 = CARTESIAN_POINT ( 'NONE',  ( 5.671770810419905828, 120.9487722882625604, -0.4210702782392469201 ) ) ;
#33370 = FACE_OUTER_BOUND ( 'NONE', #21868, .T. ) ;
#33371 = ORIENTED_EDGE ( 'NONE', *, *, #27169, .T. ) ;
#33372 = CARTESIAN_POINT ( 'NONE',  ( -36.79765817521327165, 27.64956762128696610, 1.269999999999995577 ) ) ;
#33373 = CARTESIAN_POINT ( 'NONE',  ( -11.34253674425788994, 128.2076764602477681, -0.6137764907266787251 ) ) ;
#33374 = CARTESIAN_POINT ( 'NONE',  ( 3.029556690758328674, -14.73736909467317169, 5.484434072839230012 ) ) ;
#33375 = CARTESIAN_POINT ( 'NONE',  ( -22.40052491088804842, 148.4347612714453248, 0.9998933253014316014 ) ) ;
#33376 = CARTESIAN_POINT ( 'NONE',  ( -16.71197878298170991, 83.87086364642222236, 1.269999999999996687 ) ) ;
#33377 = CARTESIAN_POINT ( 'NONE',  ( 0.2977815589728530221, 116.4565202671238069, 0.07303518451646379139 ) ) ;
#33378 = ORIENTED_EDGE ( 'NONE', *, *, #16727, .T. ) ;
#33379 = CARTESIAN_POINT ( 'NONE',  ( -0.8472427164685307766, -8.777537934218566207, -4.544909406875613733 ) ) ;
#33380 = CARTESIAN_POINT ( 'NONE',  ( -3.706843470526901996, 116.6237204831772232, -0.08772160974583163850 ) ) ;
#33381 = DIRECTION ( 'NONE',  ( -0.7517731442105904938, 0.6594218222380290317, 3.321276712443281495E-16 ) ) ;
#33382 = CARTESIAN_POINT ( 'NONE',  ( 10.92199999999999704, 12.96416000000000146, 0.000000000000000000 ) ) ;
#33383 = B_SPLINE_CURVE_WITH_KNOTS ( 'NONE', 3,
 ( #7480, #20229, #33466, #40286, #4085, #30044, #11078, #11283 ),
 .UNSPECIFIED., .F., .F.,
 ( 4, 2, 2, 4 ),
 ( -6.000000000046590246E-08, 0.002398650364449638004, 0.003598005546674457045, 0.004797360728899276519 ),
 .UNSPECIFIED. ) ;
#33384 = ORIENTED_EDGE ( 'NONE', *, *, #3870, .F. ) ;
#33385 = CARTESIAN_POINT ( 'NONE',  ( -8.274446143174570167, 120.3630673002886056, 1.110374729364685065 ) ) ;
#33386 = CARTESIAN_POINT ( 'NONE',  ( -1.146732334619779969, -3.095543821355960734, -4.488006035213349953 ) ) ;
#33387 = CARTESIAN_POINT ( 'NONE',  ( 5.309498559578469390, 158.9031408473208273, 1.190161311236993313 ) ) ;
#33388 = CARTESIAN_POINT ( 'NONE',  ( -57.74919803515421535, 1.101601998901122537, -1.404840701337578990 ) ) ;
#33390 = CARTESIAN_POINT ( 'NONE',  ( 20.99182874412617039, 148.0559997909317644, -1.564581863923973470 ) ) ;
#33389 = DIRECTION ( 'NONE',  ( 0.8745520943968260186, -0.4849315768086515099, 8.537024980200745890E-16 ) ) ;
#33391 = CARTESIAN_POINT ( 'NONE',  ( -4.449009123739010363, -11.09185097514761331, -1.246716907482375847 ) ) ;
#33392 = CARTESIAN_POINT ( 'NONE',  ( -5.838122194618600602, 117.4684171610355747, -0.7518181979692856176 ) ) ;
#33393 = TOROIDAL_SURFACE ( 'NONE', #12303, 5.080000000000005400, 0.5080000000000000071 ) ;
#33394 = ADVANCED_FACE ( 'NONE', ( #25366 ), #25585, .T. ) ;
#33395 = ORIENTED_EDGE ( 'NONE', *, *, #23484, .F. ) ;
#33396 = CARTESIAN_POINT ( 'NONE',  ( -0.6587526420363846169, 156.3106852680424765, 0.1744449402554847373 ) ) ;
#33397 = CARTESIAN_POINT ( 'NONE',  ( 5.379112111825198106, -14.48849916137785776, 3.594839802689186570 ) ) ;
#33398 = AXIS2_PLACEMENT_3D ( 'NONE', #1514, #14471, #31501 ) ;
#33399 = DIRECTION ( 'NONE',  ( -6.353134868986659519E-16, 1.000000000000000000, 0.000000000000000000 ) ) ;
#33400 = B_SPLINE_CURVE_WITH_KNOTS ( 'NONE', 3,
 ( #11512, #39298, #13520, #10732, #8328, #753, #36732, #963, #36324, #30123, #20099, #7555, #17902, #33330, #39729, #7142, #33123, #13728, #3741, #36111, #3952, #26508, #26721, #10528, #36525, #17123, #21298, #29704, #4375, #18109, #16914, #4160, #23498, #23714, #34326, #39513, #7344, #26290, #13932, #26927, #5155, #40717, #19895, #10106, #20304, #39940, #20515, #33543, #30905, #16699, #1744, #14703, #27708, #24498, #37502, #337, #32910, #13303, #6925, #545, #10319, #23287, #18527, #25355, #9174, #18316, #5781, #34535, #37719, #34738, #22131, #6192, #5569, #35160, #9375, #2162, #5987, #25558, #28341, #31532, #12152, #40921, #15121, #38562, #11727, #28124, #2376, #28551, #35362, #15752, #12367, #41350, #31114, #8543, #41134, #11940, #41559, #41770, #31956, #21502, #31318, #24931, #22339, #21714, #1951, #21929, #2795, #8752, #27915, #38359, #18736, #18950, #28757, #34958, #24715, #37929, #15336, #25144, #5361, #38148, #31746, #14911, #8961, #2589, #15549, #12571, #13410, #12773, #3847, #22757, #20000, #25763, #3414, #35790, #38770, #32581, #26399, #9581, #16811, #6602, #33018, #16381, #19366, #9997, #14, #35999, #19782, #22550, #23177, #23394, #22969, #15960, #3000, #652, #29386, #32372, #3201, #19573, #226, #13201, #6812, #7033, #26185, #41974, #39618, #39404, #29813, #39189, #10207, #13620, #16163, #35580, #32801, #26611, #29168, #6396, #10424, #12980, #28958, #3632, #16596, #29605, #440, #25973, #36212, #36426, #19161, #32165, #38981, #9789, #1487, #30226, #17851, #4059, #20411 ),
 .UNSPECIFIED., .F., .F.,
 ( 4, 1, 1, 1, 1, 1, 1, 1, 1, 1, 1, 1, 1, 1, 1, 1, 1, 1, 1, 1, 1, 1, 1, 1, 1, 1, 1, 1, 1, 1, 1, 1, 1, 1, 1, 1, 1, 1, 1, 1, 1, 1, 1, 1, 1, 1, 1, 1, 1, 1, 1, 1, 1, 1, 1, 1, 1, 1, 1, 1, 1, 1, 1, 1, 1, 1, 1, 1, 1, 1, 1, 1, 1, 1, 1, 1, 1, 1, 1, 1, 1, 1, 1, 1, 1, 1, 1, 1, 1, 1, 1, 1, 1, 1, 1, 1, 1, 1, 1, 1, 1, 1, 1, 1, 1, 1, 1, 1, 1, 1, 1, 1, 1, 1, 1, 1, 1, 1, 1, 1, 1, 1, 1, 1, 1, 1, 1, 1, 1, 1, 1, 1, 1, 1, 1, 1, 1, 1, 1, 1, 1, 1, 1, 1, 1, 1, 1, 1, 1, 1, 1, 1, 1, 1, 1, 1, 1, 1, 1, 1, 1, 1, 1, 1, 1, 1, 1, 1, 1, 1, 1, 1, 1, 1, 1, 1, 1, 1, 1, 1, 1, 1, 1, 1, 1, 1, 1, 1, 1, 1, 1, 1, 4 ),
 ( 0.000000000000000000, 0.007812500000000423273, 0.01388888888888889506, 0.01562500000000000000, 0.02343749999999998959, 0.02777777777777778317, 0.03125000000000092981, 0.03906249999999999306, 0.04166666666666667823, 0.04687500000000000000, 0.05468749999999999306, 0.05555555555555556635, 0.06249999999999997918, 0.06944444444444446141, 0.07031250000000000000, 0.07812500000000000000, 0.08333333333333334259, 0.08593749999999998612, 0.09374999999999603095, 0.09722222222222223764, 0.1015625000000000139, 0.1093750000000000000, 0.1111111111111111188, 0.1171875000000000000, 0.1250000000000000000, 0.1328125000000000000, 0.1388888888888889228, 0.1406250000000000000, 0.1484375000000000000, 0.1527777777777778179, 0.1562500000000039690, 0.1640625000000000000, 0.1666666666666666852, 0.1718750000000000000, 0.1796875000000000000, 0.1805555555555555802, 0.1875000000000000000, 0.1944444444444444753, 0.1953125000000000000, 0.2031250000000000000, 0.2083333333333333703, 0.2109375000000000000, 0.2187499999999960310, 0.2222222222222222376, 0.2265625000000000000, 0.2343750000000000000, 0.2361111111111111327, 0.2421875000000000000, 0.2500000000000000000, 0.2578125000000000000, 0.2638888888888888951, 0.2656250000000000000, 0.2734375000000000000, 0.2777777777777777346, 0.2812500000000039968, 0.2890625000000000000, 0.2916666666666665741, 0.2968750000000000000, 0.3046875000000000000, 0.3055555555555554692, 0.3125000000000000000, 0.3194444444444443088, 0.3203125000000000000, 0.3281250000000000000, 0.3333333333333332038, 0.3359375000000000000, 0.3437499999999960587, 0.3472222222222220434, 0.3515625000000000000, 0.3593750000000000000, 0.3611111111111109384, 0.3671875000000000000, 0.3750000000000000000, 0.3828125000000000000, 0.3888888888888886175, 0.3906250000000000000, 0.3984375000000000000, 0.4027777777777775126, 0.4062500000000039968, 0.4140625000000000000, 0.4166666666666663521, 0.4218750000000000000, 0.4296875000000000000, 0.4305555555555552472, 0.4375000000000000000, 0.4444444444444440867, 0.4453125000000000000, 0.4531250000000000000, 0.4583333333333329818, 0.4609375000000000000, 0.4687499999999960587, 0.4722222222222218768, 0.4765625000000000000, 0.4843750000000000000, 0.4861111111111107719, 0.4921875000000000000, 0.5000000000000000000, 0.5078125000000000000, 0.5138888888888886175, 0.5156250000000000000, 0.5234375000000000000, 0.5277777777777775681, 0.5312500000000039968, 0.5390625000000000000, 0.5416666666666664076, 0.5468750000000000000, 0.5546875000000000000, 0.5555555555555553582, 0.5625000000000000000, 0.5694444444444443088, 0.5703125000000000000, 0.5781250000000000000, 0.5833333333333331483, 0.5859375000000000000, 0.5937499999999960032, 0.5972222222222220989, 0.6015625000000000000, 0.6093750000000000000, 0.6111111111111110494, 0.6171875000000000000, 0.6250000000000000000, 0.6328125000000000000, 0.6388888888888888395, 0.6406250000000000000, 0.6484375000000000000, 0.6527777777777777901, 0.6562500000000039968, 0.6640625000000000000, 0.6666666666666666297, 0.6718750000000000000, 0.6796875000000000000, 0.6805555555555555802, 0.6875000000000000000, 0.6944444444444445308, 0.6953125000000000000, 0.7031250000000000000, 0.7083333333333333703, 0.7109375000000000000, 0.7187499999999960032, 0.7222222222222223209, 0.7265625000000000000, 0.7343750000000000000, 0.7361111111111111605, 0.7421875000000000000, 0.7500000000000000000, 0.7578125000000000000, 0.7638888888888889506, 0.7656250000000000000, 0.7734375000000000000, 0.7777777777777779011, 0.7812500000000039968, 0.7890625000000000000, 0.7916666666666668517, 0.7968750000000000000, 0.8046875000000000000, 0.8055555555555556912, 0.8125000000000000000, 0.8194444444444446418, 0.8203125000000000000, 0.8281250000000000000, 0.8333333333333335924, 0.8359375000000000000, 0.8437499999999960032, 0.8472222222222224319, 0.8515625000000000000, 0.8593750000000000000, 0.8611111111111113825, 0.8671875000000000000, 0.8750000000000000000, 0.8828125000000000000, 0.8888888888888891726, 0.8906250000000000000, 0.8984375000000000000, 0.9027777777777781232, 0.9062500000000039968, 0.9140625000000000000, 0.9166666666666670737, 0.9218750000000000000, 0.9296875000000000000, 0.9305555555555559133, 0.9375000000000000000, 0.9444444444444447528, 0.9453125000000000000, 0.9531250000000000000, 0.9583333333333335924, 0.9609375000000000000, 0.9687499999999991118, 0.9722222222222224319, 0.9765625000000000000, 0.9843750000000000000, 0.9861111111111111605, 0.9921874999999995559, 1.000000000000000000 ),
 .UNSPECIFIED. ) ;
#33401 = CARTESIAN_POINT ( 'NONE',  ( 0.02983097946977083040, 117.3993836135855133, -1.492864285907016697 ) ) ;
#33402 = ADVANCED_FACE ( 'NONE', ( #38574 ), #28968, .T. ) ;
#33403 = ORIENTED_EDGE ( 'NONE', *, *, #14947, .T. ) ;
#33404 = CARTESIAN_POINT ( 'NONE',  ( 3.228607480374420913, 118.8118204130220903, 0.9063605472083391401 ) ) ;
#33405 = CARTESIAN_POINT ( 'NONE',  ( 4.973152232786927307, 117.3993868326352015, 0.9753084504214339923 ) ) ;
#33406 = DIRECTION ( 'NONE',  ( -0.7548010569845284845, -0.6559537821943240976, -2.801824109679630066E-16 ) ) ;
#33407 = CARTESIAN_POINT ( 'NONE',  ( -0.006942562093356200587, 117.0978366787122127, 0.3474341964894884782 ) ) ;
#33408 = CARTESIAN_POINT ( 'NONE',  ( -1.555401355773622374, 10.72473834230686762, 8.302158768936594768 ) ) ;
#33409 = CARTESIAN_POINT ( 'NONE',  ( 7.153290765949940955, 121.6016026263613838, 0.8513816870021355676 ) ) ;
#33410 = LINE ( 'NONE', #33832, #39668 ) ;
#33411 = CARTESIAN_POINT ( 'NONE',  ( 15.85309526068949104, 121.4040080620525117, -0.2080479070310632672 ) ) ;
#33412 = CARTESIAN_POINT ( 'NONE',  ( -5.885917553499152355, 77.12042444889114279, 1.524000000000003352 ) ) ;
#33413 = CARTESIAN_POINT ( 'NONE',  ( -57.83161538119274070, 0.8690275533227826976, 1.064493502049185025 ) ) ;
#33414 = CARTESIAN_POINT ( 'NONE',  ( -47.91671457320775573, 24.98613645765719582, 0.3547230740385100556 ) ) ;
#33415 = CARTESIAN_POINT ( 'NONE',  ( -2.811131974896623031, 117.3993815978873414, 1.303371054368798410 ) ) ;
#33417 = CARTESIAN_POINT ( 'NONE',  ( -53.83456308493991571, 9.379524109395250164, 3.755176697756422044 ) ) ;
#33416 = B_SPLINE_CURVE_WITH_KNOTS ( 'NONE', 3,
 ( #27863, #24878, #40665, #5310, #33855, #21245, #28070, #37875, #21660, #21042 ),
 .UNSPECIFIED., .F., .F.,
 ( 4, 2, 2, 2, 4 ),
 ( 1.502521540412022121E-05, 0.0001716267095962864064, 0.0003282282037884526001, 0.0004848296979806188210, 0.0006414311921727849876 ),
 .UNSPECIFIED. ) ;
#33418 = CARTESIAN_POINT ( 'NONE',  ( -58.45888099891715228, 0.06908990101018230856, 0.7635323682102057585 ) ) ;
#33419 = EDGE_CURVE ( 'NONE', #29613, #21134, #26691, .T. ) ;
#33420 = CARTESIAN_POINT ( 'NONE',  ( -4.378391549104950542, 118.1844058569687519, 0.4336172515691945617 ) ) ;
#33421 = CARTESIAN_POINT ( 'NONE',  ( 3.441724091444921196, 108.4907294080017692, -4.067959973020410125 ) ) ;
#33422 = PRODUCT_DEFINITION_SHAPE ( 'NONE', 'NONE',  #42167 ) ;
#33423 = ORIENTED_EDGE ( 'NONE', *, *, #22462, .F. ) ;
#33424 = CARTESIAN_POINT ( 'NONE',  ( -41.97746338594183868, 23.60773098774231826, 1.523999999999994026 ) ) ;
#33425 = EDGE_CURVE ( 'NONE', #30178, #27616, #9385, .T. ) ;
#33426 = CARTESIAN_POINT ( 'NONE',  ( -6.088634770323529288, 119.5152126290041679, -1.257500645984790166 ) ) ;
#33427 = CARTESIAN_POINT ( 'NONE',  ( -7.694725746745366912, 124.7202454748262710, -0.1536377669325635076 ) ) ;
#33429 = CARTESIAN_POINT ( 'NONE',  ( 4.541907748926803379, 118.0342732306360176, 0.8605405987047681782 ) ) ;
#33428 = AXIS2_PLACEMENT_3D ( 'NONE', #25693, #22683, #42116 ) ;
#33430 = CARTESIAN_POINT ( 'NONE',  ( -9.448695200928863613, 153.9068681542131856, -1.043141309954137341 ) ) ;
#33431 = CARTESIAN_POINT ( 'NONE',  ( -0.5787063603190276684, 115.7029630171035848, -1.760568961526914000 ) ) ;
#33432 = EDGE_CURVE ( 'NONE', #22572, #3641, #28136, .T. ) ;
#33433 = CARTESIAN_POINT ( 'NONE',  ( 0.5514881128753655881, 117.3993826274773795, -1.472903135207439762 ) ) ;
#33434 = CARTESIAN_POINT ( 'NONE',  ( 6.540839804427455384, 120.6338824379019172, -0.1347920106280765806 ) ) ;
#33435 = CARTESIAN_POINT ( 'NONE',  ( -16.27782172975869557, 148.1602266505728380, -1.760797687140677192 ) ) ;
#33436 = CARTESIAN_POINT ( 'NONE',  ( 14.39766717389552220, 60.87500489999898434, 1.904999999999990257 ) ) ;
#33437 = CARTESIAN_POINT ( 'NONE',  ( -43.33782384755379269, 21.60941887711892306, 2.445739413452193478 ) ) ;
#33438 = CARTESIAN_POINT ( 'NONE',  ( 8.625062891301235268, 118.6226016915421582, -0.7970602507506778789 ) ) ;
#33439 = CARTESIAN_POINT ( 'NONE',  ( -0.002141537396551156710, 156.3034662015459446, 0.1071712884387201609 ) ) ;
#33440 = CARTESIAN_POINT ( 'NONE',  ( -17.14500000000466784, 71.11999999999886768, -1.270000000000000684 ) ) ;
#33441 = CARTESIAN_POINT ( 'NONE',  ( 20.83375562662813962, 132.2939277659177151, 1.304325680028331824 ) ) ;
#33442 = DIRECTION ( 'NONE',  ( 5.206863593109713661E-17, -1.000000000000000000, 1.077750396879097183E-30 ) ) ;
#33443 = CARTESIAN_POINT ( 'NONE',  ( 3.373996639098103323, -14.83046237366941789, 1.396824179944331723 ) ) ;
#33444 = CARTESIAN_POINT ( 'NONE',  ( -9.549337214234009608, 121.2752502669211339, 1.156350410895870429 ) ) ;
#33445 = CARTESIAN_POINT ( 'NONE',  ( -0.7500621227288748472, -10.43934603300536956, 0.6214162388253807734 ) ) ;
#33446 = CARTESIAN_POINT ( 'NONE',  ( -22.69296959717488704, 150.3666470947781022, -1.044501570340798269 ) ) ;
#33447 = CARTESIAN_POINT ( 'NONE',  ( 0.3060232888392590556, -2.951246395405549450, 0.9280917289473271659 ) ) ;
#33448 = ORIENTED_EDGE ( 'NONE', *, *, #11494, .F. ) ;
#33449 = CARTESIAN_POINT ( 'NONE',  ( -49.96466797210978683, 13.31430344189337589, 0.7651684107024910864 ) ) ;
#33450 = CARTESIAN_POINT ( 'NONE',  ( 2.643983731439564444, 108.0685014782224442, 4.389169220726125253 ) ) ;
#33451 = CONTEXT_DEPENDENT_SHAPE_REPRESENTATION ( #1779, #35428 ) ;
#33452 = CARTESIAN_POINT ( 'NONE',  ( -3.641174103387575745, 120.8049117488720015, 0.2662595081522519669 ) ) ;
#33453 = CARTESIAN_POINT ( 'NONE',  ( 3.361239686659836856, -14.56070858809799162, 5.257229516148527182 ) ) ;
#33454 = CARTESIAN_POINT ( 'NONE',  ( 17.58003597271441620, 146.9817191466759141, -1.463309413676198156 ) ) ;
#33455 = EDGE_LOOP ( 'NONE', ( #11223, #7646, #36472, #21573, #41359, #13101, #38662, #11160 ) ) ;
#33456 = CARTESIAN_POINT ( 'NONE',  ( -2.329084838959003534, 118.9063233352275972, -0.7992829875212341673 ) ) ;
#33457 = CARTESIAN_POINT ( 'NONE',  ( 0.7256241136792617175, 104.6144662015456817, 4.780927069918088357 ) ) ;
#33458 = TOROIDAL_SURFACE ( 'NONE', #27324, 0.7620000000000000107, 0.2540000000000000036 ) ;
#33459 = CARTESIAN_POINT ( 'NONE',  ( 2.666490510518176649, -13.49855353256042889, 0.05227394649444832425 ) ) ;
#33460 = CARTESIAN_POINT ( 'NONE',  ( -4.831581646441107658, 117.6432783874694366, -1.087973816982874320 ) ) ;
#33461 = CARTESIAN_POINT ( 'NONE',  ( 5.999396524113651097, 155.3621521873626534, -0.05839828084409114106 ) ) ;
#33462 = EDGE_LOOP ( 'NONE', ( #6419, #37046, #5035, #32591, #34638, #27435 ) ) ;
#33463 = CARTESIAN_POINT ( 'NONE',  ( 3.009276887026298031, 39.20946620154573736, -1.210121013456480599 ) ) ;
#33464 = CARTESIAN_POINT ( 'NONE',  ( 2.163405660033729028, 107.1115117626483055, 4.788046284768042504 ) ) ;
#33465 = AXIS2_PLACEMENT_3D ( 'NONE', #19189, #32196, #3030 ) ;
#33466 = CARTESIAN_POINT ( 'NONE',  ( 3.168525235803220763, 117.3993833749843532, 1.398852401101993159 ) ) ;
#33467 = DIRECTION ( 'NONE',  ( -0.8745520943968240202, 0.4849315768086551737, -5.361993529360572958E-16 ) ) ;
#33468 = ADVANCED_FACE ( 'NONE', ( #31329, #22349 ), #41571, .F. ) ;
#33469 = CARTESIAN_POINT ( 'NONE',  ( 22.82234304556241256, 150.4043717142618277, 0.2269822898261401878 ) ) ;
#33470 = CARTESIAN_POINT ( 'NONE',  ( -41.05189575270519242, 23.09451173561980042, -1.270000000000005125 ) ) ;
#33471 = CARTESIAN_POINT ( 'NONE',  ( 1.941303917661279632, -15.39441291017290503, 6.018986302445838099 ) ) ;
#33472 = CARTESIAN_POINT ( 'NONE',  ( 12.21488373878702127, 55.49440886859300548, 5.016499999999999737 ) ) ;
#33473 = CARTESIAN_POINT ( 'NONE',  ( -0.1605347423948317587, 34.07300127660931111, 0.3172648596225849382 ) ) ;
#33474 = CARTESIAN_POINT ( 'NONE',  ( 18.19503446209933983, 151.8090458617612057, 2.356823057848428160 ) ) ;
#33475 = ORIENTED_EDGE ( 'NONE', *, *, #5549, .F. ) ;
#33476 = CARTESIAN_POINT ( 'NONE',  ( 1.359589829139859152, 24.67768052395325284, 8.332721669750835503 ) ) ;
#33477 = CARTESIAN_POINT ( 'NONE',  ( 2.336946977945878690, 117.1813995298343656, -0.5665797218883661390 ) ) ;
#33478 = CARTESIAN_POINT ( 'NONE',  ( -3.231430644863531931, 118.6786177306206014, -0.7432888438146499910 ) ) ;
#33479 = FACE_OUTER_BOUND ( 'NONE', #13722, .T. ) ;
#33480 = CARTESIAN_POINT ( 'NONE',  ( -4.800085724567980883, 115.7029491485352537, -1.472342921364584889 ) ) ;
#33481 = CARTESIAN_POINT ( 'NONE',  ( -0.0006472084743510491366, 124.6436471961814476, 0.03238895860161190854 ) ) ;
#33482 = CIRCLE ( 'NONE', #15088, 0.6350000000000014522 ) ;
#33483 = CARTESIAN_POINT ( 'NONE',  ( -0.2084201458593382406, 5.265951782950084592, 4.622859108429906883 ) ) ;
#33484 = EDGE_CURVE ( 'NONE', #41561, #18870, #9929, .T. ) ;
#33485 = CARTESIAN_POINT ( 'NONE',  ( -5.208855653336853742, 31.38455280743060527, -0.6720767434146609487 ) ) ;
#33486 = CARTESIAN_POINT ( 'NONE',  ( -4.765768241072703582, 118.5264896598256854, 0.8412120300991379196 ) ) ;
#33487 = CARTESIAN_POINT ( 'NONE',  ( 2.739926266261139887, -12.91893237176182296, 0.2921503600690461555 ) ) ;
#33488 = CARTESIAN_POINT ( 'NONE',  ( 0.4402454045156525830, 106.4201689084969047, -5.104646014783341457 ) ) ;
#33489 = CARTESIAN_POINT ( 'NONE',  ( -11.36388202081354137, 118.9804978796424706, 0.4533785775503093585 ) ) ;
#33490 = CARTESIAN_POINT ( 'NONE',  ( -1.149787651882492989, 32.77214111141197606, 3.982284714218304433 ) ) ;
#33491 = DIRECTION ( 'NONE',  ( -5.188838149069472160E-16, 1.699382548006136559E-16, 1.000000000000000000 ) ) ;
#33492 = ORIENTED_EDGE ( 'NONE', *, *, #3776, .F. ) ;
#33493 = CARTESIAN_POINT ( 'NONE',  ( 5.332935392244917416, 115.7029491189645825, 0.1065647408284378928 ) ) ;
#33494 = CARTESIAN_POINT ( 'NONE',  ( 3.313323393711395948, -15.78004832563367721, 4.785553473879357256 ) ) ;
#33495 = CARTESIAN_POINT ( 'NONE',  ( -14.40310572532117384, 154.4775811199918110, 1.681202589455180307 ) ) ;
#33496 = CARTESIAN_POINT ( 'NONE',  ( 1.360477052538118681, -3.804838552850991817, 4.419457122809256511 ) ) ;
#33497 = VERTEX_POINT ( 'NONE', #5998 ) ;
#33498 = CARTESIAN_POINT ( 'NONE',  ( -58.35999251409288036, -0.2710268728051273834, -0.1245515173812772602 ) ) ;
#33499 = CARTESIAN_POINT ( 'NONE',  ( 0.7466139261199012944, 119.9044272045951374, 0.6467483038796006944 ) ) ;
#33500 = CARTESIAN_POINT ( 'NONE',  ( -0.02156534543299366835, 156.6359106937186709, 1.079218069903262744 ) ) ;
#33501 = CARTESIAN_POINT ( 'NONE',  ( -6.194847070882102180, 64.72978607931611350, -1.523999999999994026 ) ) ;
#33502 = TOROIDAL_SURFACE ( 'NONE', #20544, 0.3810000000000001719, 0.2540000000000000036 ) ;
#33503 = CARTESIAN_POINT ( 'NONE',  ( 11.50356673920478201, 154.6851215890897038, -1.708948620147628716 ) ) ;
#33504 = CARTESIAN_POINT ( 'NONE',  ( -2.184917017309302878, 118.1205262787358663, -0.7523320384000312666 ) ) ;
#33505 = FACE_OUTER_BOUND ( 'NONE', #32824, .T. ) ;
#33506 = CARTESIAN_POINT ( 'NONE',  ( 4.241009399425758275, 118.2240432067376759, -0.3200593562746568144 ) ) ;
#33507 = CARTESIAN_POINT ( 'NONE',  ( 9.384706802269484172, 123.8909350679826815, -0.3250447036211729368 ) ) ;
#33508 = VERTEX_POINT ( 'NONE', #12163 ) ;
#33509 = CARTESIAN_POINT ( 'NONE',  ( 3.216867006742271329, -14.81339725456490264, 3.133484537391586944 ) ) ;
#33510 = CARTESIAN_POINT ( 'NONE',  ( 10.79307885933854294, 57.10041794475097987, -5.016500000000000625 ) ) ;
#33511 = CIRCLE ( 'NONE', #5606, 2.540000000000004032 ) ;
#33512 = CARTESIAN_POINT ( 'NONE',  ( -58.36915991843477514, -0.2902476589043412325, 0.03232548579181320630 ) ) ;
#33513 = CARTESIAN_POINT ( 'NONE',  ( -1.889208318266999198, 10.27326514537015534, 4.227218769941996968 ) ) ;
#33514 = CARTESIAN_POINT ( 'NONE',  ( 8.921947645406950400, 154.9128698100208794, 1.713759150786742458 ) ) ;
#33515 = CARTESIAN_POINT ( 'NONE',  ( 2.940994655134018032, 38.68039677755331951, -0.1346318768538148081 ) ) ;
#33516 = CARTESIAN_POINT ( 'NONE',  ( 4.617411384770501392, 7.639850289152962048, 0.2838591255797697777 ) ) ;
#33517 = CARTESIAN_POINT ( 'NONE',  ( 13.59043555108493884, 150.2357272821285221, 0.3212980696657039004 ) ) ;
#33518 = CARTESIAN_POINT ( 'NONE',  ( 5.078986093043053707, 92.04146620154574521, 0.1014902294541244060 ) ) ;
#33519 = AXIS2_PLACEMENT_3D ( 'NONE', #6424, #5604, #32402 ) ;
#33520 = ADVANCED_FACE ( 'NONE', ( #12380 ), #35373, .T. ) ;
#33521 =( BOUNDED_SURFACE ( )  B_SPLINE_SURFACE ( 3, 2, ( 
 ( #5928, #41917, #41705 ),
 ( #2938, #14385, #33173 ),
 ( #19945, #10782, #26980 ),
 ( #29755, #17172, #23976 ) ),
 .UNSPECIFIED., .F., .F., .T. ) 
 B_SPLINE_SURFACE_WITH_KNOTS ( ( 4, 4 ),
 ( 3, 3 ),
 ( 8.673617379884035472E-19, 6.346505048319266184E-05 ),
 ( 0.000000000000000000, 1.000000000000000000 ),
 .UNSPECIFIED. ) 
 GEOMETRIC_REPRESENTATION_ITEM ( )  RATIONAL_B_SPLINE_SURFACE ( (
 ( 1.000000000000000000, 0.7071067811865690000, 1.000000000000000000),
 ( 1.000000000000000000, 0.7071067753522035648, 1.000000000000000000),
 ( 1.000000000000000000, 0.7071464246557217503, 1.000000000000000000),
 ( 1.000000000000000000, 0.7072256012392765800, 1.000000000000000000) ) ) 
 REPRESENTATION_ITEM ( '' )  SURFACE ( )  );
#33522 = CARTESIAN_POINT ( 'NONE',  ( -56.39145920764457287, 3.696195836928164891, -1.449839391286715573 ) ) ;
#33523 = CARTESIAN_POINT ( 'NONE',  ( -8.789536962982657187, 117.7096669775960862, -0.3419224959890725390 ) ) ;
#33524 = CARTESIAN_POINT ( 'NONE',  ( -6.629500982736845120E-14, 97.88346620154572975, -1.984505748321436882E-18 ) ) ;
#33525 = CARTESIAN_POINT ( 'NONE',  ( -46.94649113550044461, 25.08650387525446845, -1.922972035666928203 ) ) ;
#33526 = FACE_OUTER_BOUND ( 'NONE', #34207, .T. ) ;
#33527 = CARTESIAN_POINT ( 'NONE',  ( -30.55042969390685315, 56.28656473939154381, -1.270000000000100160 ) ) ;
#33528 = CARTESIAN_POINT ( 'NONE',  ( 4.034796628256747120, -3.593727855734754950, 7.433834689985365785 ) ) ;
#33529 = EDGE_CURVE ( 'NONE', #40534, #20298, #9185, .T. ) ;
#33530 = CARTESIAN_POINT ( 'NONE',  ( -6.373576640880495633E-14, 50.63946620154572997, 5.832708929232124832E-29 ) ) ;
#33531 = DIRECTION ( 'NONE',  ( 0.01997839162482749689, 1.040247600000945640E-18, -0.9998004120163610509 ) ) ;
#33532 = CARTESIAN_POINT ( 'NONE',  ( -58.70413935429054675, 0.2332485698458008905, 0.6626129746612758886 ) ) ;
#33533 = CARTESIAN_POINT ( 'NONE',  ( 0.01111760956202519947, 120.5507043431653784, -0.5563706444133252882 ) ) ;
#33534 = CARTESIAN_POINT ( 'NONE',  ( -20.08431799972946052, 128.8637844977697569, 0.1093955315764417319 ) ) ;
#33535 = ORIENTED_EDGE ( 'NONE', *, *, #26947, .F. ) ;
#33536 = CARTESIAN_POINT ( 'NONE',  ( -57.78866059769681129, 2.451738602565561642, -1.593934435026652219 ) ) ;
#33537 = CARTESIAN_POINT ( 'NONE',  ( -7.784760752776371362, 122.6240640030675877, -0.1928348868300470975 ) ) ;
#33538 = ORIENTED_EDGE ( 'NONE', *, *, #8613, .F. ) ;
#33539 = CARTESIAN_POINT ( 'NONE',  ( -45.03191848990922352, 21.16108440571266414, -3.788620003469220343 ) ) ;
#33540 = CARTESIAN_POINT ( 'NONE',  ( -0.6448247514297434924, 156.3042436901572216, -0.08557349692115849560 ) ) ;
#33541 = CARTESIAN_POINT ( 'NONE',  ( 5.498302128480847983, -14.40662979408034694, 3.384674516772870234 ) ) ;
#33542 = CARTESIAN_POINT ( 'NONE',  ( -15.16136233027302183, 154.7927800759015042, 1.480671785937533569 ) ) ;
#33543 = CARTESIAN_POINT ( 'NONE',  ( -3.854280124997887746, 21.23357344512866973, -2.551540157904111261 ) ) ;
#33544 = CIRCLE ( 'NONE', #38279, 0.2539999999999981717 ) ;
#33545 = CARTESIAN_POINT ( 'NONE',  ( 2.795228999030319628, 116.6385632091030544, 0.2515850966972204561 ) ) ;
#33546 = CARTESIAN_POINT ( 'NONE',  ( 2.204990229119355050, -15.43588533350201430, 5.895893715474639585 ) ) ;
#33547 = B_SPLINE_CURVE_WITH_KNOTS ( 'NONE', 3,
 ( #23866, #26864, #896, #40083, #36885, #7703, #39872, #13871, #20242, #23218, #30058, #23432, #4309, #14274, #17056, #20666, #479, #7073, #33690, #10463, #16850, #33055, #10879, #29850 ),
 .UNSPECIFIED., .F., .F.,
 ( 4, 2, 2, 2, 1, 2, 2, 2, 2, 1, 2, 2, 4 ),
 ( 0.000000000000000000, 0.2499999999999849565, 0.3749999999999771849, 0.4374999999999723554, 0.4687499999999691358, 0.4843749999999673039, 0.4999999999999654721, 0.6249999999999718003, 0.6874999999999765743, 0.7187499999999787947, 0.7343749999999799050, 0.7499999999999809042, 1.000000000000000000 ),
 .UNSPECIFIED. ) ;
#33548 = CARTESIAN_POINT ( 'NONE',  ( -29.35823734812138852, 61.32503332634691873, 1.269999999999994245 ) ) ;
#33549 = CARTESIAN_POINT ( 'NONE',  ( 0.9102147817015755482, -10.07290960004636737, -0.3509275504499672627 ) ) ;
#33550 = CARTESIAN_POINT ( 'NONE',  ( -3.748677658115184386, 116.6824454826851820, -0.2320358872840702358 ) ) ;
#33551 = CARTESIAN_POINT ( 'NONE',  ( -4.823516985575233562, 117.8389059115630744, 0.7421444254238848126 ) ) ;
#33552 = CARTESIAN_POINT ( 'NONE',  ( 10.38331224698210242, 57.14999999999999858, 5.016499999999999737 ) ) ;
#33553 = CARTESIAN_POINT ( 'NONE',  ( 8.748582098294324538, 117.8797259988493096, 0.6463030221440396739 ) ) ;
#33554 = CARTESIAN_POINT ( 'NONE',  ( -9.240212912644894416, 121.6705353891887995, 1.055487293716822039 ) ) ;
#33555 = CARTESIAN_POINT ( 'NONE',  ( -58.13670558675570987, 0.2084532747741471848, -0.6632339434594649585 ) ) ;
#33556 = CARTESIAN_POINT ( 'NONE',  ( 13.87194369518284809, 121.7708260186165177, 1.632391212143506021 ) ) ;
#33557 = CARTESIAN_POINT ( 'NONE',  ( 19.34566907036573014, 149.3473233412102275, -1.724881794388704703 ) ) ;
#33558 = CARTESIAN_POINT ( 'NONE',  ( -0.6538259107469485132, -10.21753563294075384, 0.7251761174241220242 ) ) ;
#33559 = CARTESIAN_POINT ( 'NONE',  ( -5.844526503020657238, 118.0670013439590491, -1.005764768584936686 ) ) ;
#33560 = CARTESIAN_POINT ( 'NONE',  ( -46.20552558087364758, 24.41938074005533466, -2.020549794458512682 ) ) ;
#33561 = CIRCLE ( 'NONE', #15155, 0.7620000000000015650 ) ;
#33562 = CARTESIAN_POINT ( 'NONE',  ( 5.190856860529054373, 105.1222051271263780, 1.277391616506039274 ) ) ;
#33563 = CARTESIAN_POINT ( 'NONE',  ( 8.590326429123150476, 154.7538831414287870, -1.096848044820071921 ) ) ;
#33564 = CARTESIAN_POINT ( 'NONE',  ( -11.82813386268903955, 130.3161362890850512, -0.2363542639706541493 ) ) ;
#33565 = VERTEX_POINT ( 'NONE', #2805 ) ;
#33566 = CARTESIAN_POINT ( 'NONE',  ( -12.38071862475251450, 124.1810962131942517, -1.797420231217670139 ) ) ;
#33567 = CARTESIAN_POINT ( 'NONE',  ( 2.573200380748495331, -15.70867456196409151, 5.149826986703908815 ) ) ;
#33568 = DIRECTION ( 'NONE',  ( 0.9998004120163608288, 0.000000000000000000, 0.01997839162482736852 ) ) ;
#33569 = CARTESIAN_POINT ( 'NONE',  ( -4.441329932981612494, 118.1268108493847109, -0.7296998205460351050 ) ) ;
#33570 = CARTESIAN_POINT ( 'NONE',  ( -54.34142964503966056, 9.837102586603037935, -3.694930414371515148 ) ) ;
#33571 = CARTESIAN_POINT ( 'NONE',  ( -6.527452395418614125E-14, 72.48346620154573827, -8.020333044904917549E-18 ) ) ;
#33572 = CARTESIAN_POINT ( 'NONE',  ( 6.586386431196439517, 120.2999964176511014, 1.183541128842728885 ) ) ;
#33573 = DIRECTION ( 'NONE',  ( 4.017660918040594346E-17, -1.000000000000000000, -2.376309959284834438E-19 ) ) ;
#33574 = CARTESIAN_POINT ( 'NONE',  ( 16.31694223957253698, 121.4173703750124531, 0.3260513381110076714 ) ) ;
#33575 = CARTESIAN_POINT ( 'NONE',  ( 7.667154907385915763, 6.987472373264454362, 3.492918021822637442 ) ) ;
#33576 = CARTESIAN_POINT ( 'NONE',  ( 10.60367000503885748, 126.1357510980948575, 0.6849044484263044907 ) ) ;
#33577 = AXIS2_PLACEMENT_3D ( 'NONE', #25486, #5698, #35712 ) ;
#33578 = CARTESIAN_POINT ( 'NONE',  ( 17.61824099940326604, 125.1652531886817172, -0.6886689253619217022 ) ) ;
#33579 = LINE ( 'NONE', #1208, #2960 ) ;
#33580 = AXIS2_PLACEMENT_3D ( 'NONE', #6683, #19864, #38644 ) ;
#33581 = CARTESIAN_POINT ( 'NONE',  ( -58.20750686534850615, 0.04498437427168100466, 0.4973296020553291119 ) ) ;
#33582 = ADVANCED_FACE ( 'NONE', ( #15766 ), #19763, .T. ) ;
#33583 = CARTESIAN_POINT ( 'NONE',  ( -0.8998519745136789316, 116.4604358222411236, 0.05108568132534212214 ) ) ;
#33584 = EDGE_LOOP ( 'NONE', ( #33792, #20354, #28810, #35563 ) ) ;
#33585 = CARTESIAN_POINT ( 'NONE',  ( -46.67361288142431164, 26.04169289900193363, -0.9171659260646428669 ) ) ;
#33586 = CARTESIAN_POINT ( 'NONE',  ( -5.679082498912885413, 121.0114208266025599, -0.6118695118735946181 ) ) ;
#33587 = CARTESIAN_POINT ( 'NONE',  ( -17.14500000000466784, 71.11999999999886768, -1.524000000000000909 ) ) ;
#33588 = DIRECTION ( 'NONE',  ( -0.3256999990547775337, -0.9454731675810359448, 0.000000000000000000 ) ) ;
#33589 = CARTESIAN_POINT ( 'NONE',  ( -2.769557799161974199, 120.9068798055765370, -0.2367794989410799689 ) ) ;
#33590 = CARTESIAN_POINT ( 'NONE',  ( 4.077043646397369159, -14.32506836492906999, 4.807529146363894057 ) ) ;
#33591 = CARTESIAN_POINT ( 'NONE',  ( -22.28974849274172598, 149.2301036976659816, 0.9981255638314735501 ) ) ;
#33592 = DIRECTION ( 'NONE',  ( -6.353134868986659519E-16, 1.000000000000000000, 0.000000000000000000 ) ) ;
#33593 = CARTESIAN_POINT ( 'NONE',  ( 22.73177750447365497, 137.3553536570635742, 0.5243227317837022561 ) ) ;
#33594 = EDGE_LOOP ( 'NONE', ( #33325, #24053, #20848, #37898 ) ) ;
#33595 = CARTESIAN_POINT ( 'NONE',  ( 4.219463811995017188, -1.205994944679912306, -1.932895124392335573 ) ) ;
#33596 = CARTESIAN_POINT ( 'NONE',  ( -11.73662545640882904, 118.7267541726749869, -0.2503127652027325456 ) ) ;
#33597 = CARTESIAN_POINT ( 'NONE',  ( 5.078986093043053707, 81.62746620154572952, 0.1014902294541237954 ) ) ;
#33598 = PLANE ( 'NONE',  #25162 ) ;
#33599 = VERTEX_POINT ( 'NONE', #16051 ) ;
#33600 = CARTESIAN_POINT ( 'NONE',  ( -5.506994448060305025, 119.6850719548569941, 0.8864364066137871978 ) ) ;
#33601 = CARTESIAN_POINT ( 'NONE',  ( 4.168288449772385995, -6.568960759998498489, 2.029292378399509378 ) ) ;
#33602 = CARTESIAN_POINT ( 'NONE',  ( -0.008308726997799834729, 117.3658353995175503, 0.4158026747930030353 ) ) ;
#33603 = CARTESIAN_POINT ( 'NONE',  ( -57.99063839910062512, 1.082714195263373425, -1.370926835928584664 ) ) ;
#33604 = CARTESIAN_POINT ( 'NONE',  ( 4.850700283611232067, 158.3075559295907055, -1.526604748539100775 ) ) ;
#33605 = AXIS2_PLACEMENT_3D ( 'NONE', #798, #10367, #4629 ) ;
#33606 = CARTESIAN_POINT ( 'NONE',  ( 1.463615122064738427, -3.970138727222522590, -4.384008014421088895 ) ) ;
#33607 = CARTESIAN_POINT ( 'NONE',  ( 0.01443894962456205439, 159.4760848062415732, -0.7225840825867285711 ) ) ;
#33608 = VERTEX_POINT ( 'NONE', #22430 ) ;
#33610 = AXIS2_PLACEMENT_3D ( 'NONE', #16473, #32677, #35250 ) ;
#33609 = CARTESIAN_POINT ( 'NONE',  ( -8.625872078176357149, 123.3364012560002578, 0.04702935286775016682 ) ) ;
#33611 = CARTESIAN_POINT ( 'NONE',  ( 4.984919470525341012, -14.71752327621497791, 4.178560682339194976 ) ) ;
#33612 = DIRECTION ( 'NONE',  ( -1.000000000000000000, 1.011795553208986254E-16, 0.000000000000000000 ) ) ;
#33613 = TOROIDAL_SURFACE ( 'NONE', #13860, 0.7620000000000000107, 0.2540000000000000036 ) ;
#33614 = CARTESIAN_POINT ( 'NONE',  ( -4.943847941134515089, 113.9634239269208393, -2.116083417004583467 ) ) ;
#33615 = ORIENTED_EDGE ( 'NONE', *, *, #11287, .T. ) ;
#33616 = CARTESIAN_POINT ( 'NONE',  ( 12.03045567952066364, 122.8144071692085504, 1.784322758991244040 ) ) ;
#33617 = EDGE_CURVE ( 'NONE', #19469, #27131, #35049, .T. ) ;
#33618 = CIRCLE ( 'NONE', #32926, 0.6350000000000014522 ) ;
#33619 = AXIS2_PLACEMENT_3D ( 'NONE', #32765, #5953, #22304 ) ;
#33620 = PLANE ( 'NONE',  #32081 ) ;
#33621 = CARTESIAN_POINT ( 'NONE',  ( -21.83270838041260120, 150.5404744109896171, 0.8586010584139895929 ) ) ;
#33622 = CARTESIAN_POINT ( 'NONE',  ( -3.310625167495538257, 6.824969433126684137, -7.744297517547710896 ) ) ;
#33623 = CARTESIAN_POINT ( 'NONE',  ( 3.199116795994500606, 156.2293907256693331, 0.9954876105832139999 ) ) ;
#33624 = DIRECTION ( 'NONE',  ( -5.206863593109713661E-17, 1.000000000000000000, -1.077750396879097183E-30 ) ) ;
#33625 = EDGE_CURVE ( 'NONE', #27874, #14494, #23535, .T. ) ;
#33626 = CARTESIAN_POINT ( 'NONE',  ( 18.31971715989119076, 125.1624627582897915, -0.2149060778942796235 ) ) ;
#33627 = DIRECTION ( 'NONE',  ( 1.000000000000000000, -1.044409991968847179E-16, 0.000000000000000000 ) ) ;
#33628 = CIRCLE ( 'NONE', #26805, 5.588000000000006295 ) ;
#33629 = CARTESIAN_POINT ( 'NONE',  ( -56.15333643087780047, 4.440440768670265825, 2.369795045322684590 ) ) ;
#33630 = CARTESIAN_POINT ( 'NONE',  ( -48.26009918843825375, 20.16784055841990764, 4.711418872450271245 ) ) ;
#33631 = CARTESIAN_POINT ( 'NONE',  ( -57.97566020452313040, 1.918554019021911916, 1.632400077439698061 ) ) ;
#33632 = CARTESIAN_POINT ( 'NONE',  ( -58.63629444759789777, -0.3008185210916128893, 0.3590172183976028664 ) ) ;
#33633 = EDGE_CURVE ( 'NONE', #14016, #4305, #19039, .T. ) ;
#33634 = CARTESIAN_POINT ( 'NONE',  ( -4.394434931943050238, 118.1841795841535827, 0.4163878308331336875 ) ) ;
#33635 = CARTESIAN_POINT ( 'NONE',  ( 1.392235599252770184, 106.3000011757766003, -5.100451643702543336 ) ) ;
#33636 = ORIENTED_EDGE ( 'NONE', *, *, #10346, .F. ) ;
#33637 = CARTESIAN_POINT ( 'NONE',  ( -43.83556092231052048, 21.45200552150719631, 2.811646013901242025 ) ) ;
#33638 = CARTESIAN_POINT ( 'NONE',  ( -6.112386360759682447, 119.5658119500284755, -1.253701994526288832 ) ) ;
#33639 = CARTESIAN_POINT ( 'NONE',  ( -7.669310211018488310, 124.7206709383052043, -0.1531702926821040256 ) ) ;
#33640 = CARTESIAN_POINT ( 'NONE',  ( 4.459538917479417997, 118.1136197194245625, 0.7514127147595077716 ) ) ;
#33641 = CARTESIAN_POINT ( 'NONE',  ( -1.517991627498799900, 120.5919059741422217, -0.3392643659851172222 ) ) ;
#33642 = CARTESIAN_POINT ( 'NONE',  ( -0.7773321051407233728, 115.7028436671041192, -1.754947197622949817 ) ) ;
#33643 = CARTESIAN_POINT ( 'NONE',  ( 0.4423781608754945860, 117.9496046456311120, -1.391511169922456270 ) ) ;
#33644 = CARTESIAN_POINT ( 'NONE',  ( -4.349660437102230048, 31.17966527223318707, -1.615541842050199461 ) ) ;
#33645 = CARTESIAN_POINT ( 'NONE',  ( -3.288791919378307504, 156.3062290909284116, -1.149731754608032563 ) ) ;
#33646 = EDGE_CURVE ( 'NONE', #38078, #36646, #24207, .T. ) ;
#33647 = DIRECTION ( 'NONE',  ( -5.188838149069472160E-16, 1.699382548006136559E-16, 1.000000000000000000 ) ) ;
#33648 = CARTESIAN_POINT ( 'NONE',  ( -3.743815577281075058, 31.31851751214970037, -0.6207396561878217867 ) ) ;
#33649 = CARTESIAN_POINT ( 'NONE',  ( 7.878666962137408802, 122.2304107671078981, -0.4668939115120620542 ) ) ;
#33650 = CARTESIAN_POINT ( 'NONE',  ( -9.093386426035655390, 153.9805809586646888, -0.007641094020508640110 ) ) ;
#33651 = CARTESIAN_POINT ( 'NONE',  ( 5.078986093043052819, 101.1854662015457365, 0.1014902294541237954 ) ) ;
#33652 = CARTESIAN_POINT ( 'NONE',  ( 4.821777392514684735, 117.1414559920645644, 0.5894805283384126904 ) ) ;
#33653 = LINE ( 'NONE', #27658, #4998 ) ;
#33654 = CARTESIAN_POINT ( 'NONE',  ( 3.411744169395244164, -14.91921274028452871, 2.011823270444000666 ) ) ;
#33655 = CARTESIAN_POINT ( 'NONE',  ( -10.61219202125007399, 121.9340018749941663, 1.210411277014657561 ) ) ;
#33656 = CARTESIAN_POINT ( 'NONE',  ( 0.6771123631923940955, -5.471153235863896569, -0.7014129483058207937 ) ) ;
#33657 = CARTESIAN_POINT ( 'NONE',  ( -13.14908049612679974, 156.9583929045107595, -0.9825115876436353313 ) ) ;
#33658 = CARTESIAN_POINT ( 'NONE',  ( -0.3362158861861603287, -7.698726726604804504, -0.9163890413163552351 ) ) ;
#33659 = ORIENTED_EDGE ( 'NONE', *, *, #7627, .T. ) ;
#33660 = CARTESIAN_POINT ( 'NONE',  ( -51.51920269172890698, 12.50394502492935978, 2.730133853924309850 ) ) ;
#33661 = CARTESIAN_POINT ( 'NONE',  ( 5.229314312453159808, 116.0897965414613964, 1.239798673375258842 ) ) ;
#33662 = APPLICATION_PROTOCOL_DEFINITION ( 'draft international standard', 'automotive_design', 1998, #9918 ) ;
#33663 = CARTESIAN_POINT ( 'NONE',  ( -0.009747742627877935620, 156.3581291470199233, 0.4878169013068173743 ) ) ;
#33664 = EDGE_CURVE ( 'NONE', #26949, #28714, #19464, .T. ) ;
#33665 = CARTESIAN_POINT ( 'NONE',  ( 2.771648496353774860, -15.01054376081380148, 5.729243832102374867 ) ) ;
#33666 = CARTESIAN_POINT ( 'NONE',  ( 10.73673663838188475, 123.5542795626547417, -1.004701191943994765 ) ) ;
#33667 = EDGE_LOOP ( 'NONE', ( #10169, #16390, #5452, #22192 ) ) ;
#33668 = CARTESIAN_POINT ( 'NONE',  ( -8.358437701610750281, 156.6436466068687423, -2.074018175080057702 ) ) ;
#33669 = CARTESIAN_POINT ( 'NONE',  ( 3.489354382163187385, 115.7029491485452866, 1.632628334074333720 ) ) ;
#33670 = CARTESIAN_POINT ( 'NONE',  ( 2.946624452826990925, -14.63926610985447141, 4.195571020465345136 ) ) ;
#33671 = CARTESIAN_POINT ( 'NONE',  ( -18.83202234259777441, 80.34319284215894186, 1.523999999999995358 ) ) ;
#33672 = ADVANCED_FACE ( 'NONE', ( #5665 ), #32356, .T. ) ;
#33673 = CARTESIAN_POINT ( 'NONE',  ( 1.597555633484664339, 120.9451058151398399, -0.06333991727891964685 ) ) ;
#33674 = ORIENTED_EDGE ( 'NONE', *, *, #13078, .F. ) ;
#33675 = CARTESIAN_POINT ( 'NONE',  ( 3.174067013697414730, 118.4902560533893592, 0.8904294910640483396 ) ) ;
#33676 = CARTESIAN_POINT ( 'NONE',  ( 3.402909602042748283, 108.3861600575998949, 4.100009543453226435 ) ) ;
#33677 = DIRECTION ( 'NONE',  ( -0.1906721105965039909, 0.9816537812491094028, -2.657572025465702696E-16 ) ) ;
#33678 = EDGE_CURVE ( 'NONE', #16922, #700, #40571, .T. ) ;
#33679 = DIRECTION ( 'NONE',  ( -0.8745520943968243532, 0.4849315768086547296, -5.361993529360573944E-16 ) ) ;
#33680 = CARTESIAN_POINT ( 'NONE',  ( 22.52215935351586751, 150.7865899205276321, 0.2217371156544979960 ) ) ;
#33681 = DIRECTION ( 'NONE',  ( -5.188838149069471174E-16, 1.699382548006136313E-16, 1.000000000000000000 ) ) ;
#33682 = CARTESIAN_POINT ( 'NONE',  ( 2.054492031761760984, -15.24248389176698026, 5.952799576744645549 ) ) ;
#33683 = DIRECTION ( 'NONE',  ( -0.000000000000000000, -0.000000000000000000, -1.000000000000000000 ) ) ;
#33684 = FACE_OUTER_BOUND ( 'NONE', #33065, .T. ) ;
#33685 = CARTESIAN_POINT ( 'NONE',  ( -0.02969037535081452128, 158.7301711276701894, 1.485827791648137275 ) ) ;
#33686 = EDGE_LOOP ( 'NONE', ( #4228, #31964 ) ) ;
#33687 = CARTESIAN_POINT ( 'NONE',  ( 1.932697321913770416, 19.28018055242734619, -8.218723488459904303 ) ) ;
#33688 = CARTESIAN_POINT ( 'NONE',  ( 5.539598496142141393, 117.7704119632382032, -0.8150624102158662287 ) ) ;
#33689 = CARTESIAN_POINT ( 'NONE',  ( -3.894863181655659368, 121.5791280715047122, -0.3237234463424496500 ) ) ;
#33690 = CARTESIAN_POINT ( 'NONE',  ( -5.787341484272856107, 78.89667267365574332, 5.030122981225376932 ) ) ;
#33691 = DIRECTION ( 'NONE',  ( 0.9816537812491126225, 0.1906721105964872265, 8.537024980200846470E-16 ) ) ;
#33692 = CARTESIAN_POINT ( 'NONE',  ( -3.966471221021101723, 104.6144662015457243, 2.768186473823242011 ) ) ;
#33693 = CARTESIAN_POINT ( 'NONE',  ( -4.319812470756069445, 11.96289413176387129, -1.686699837767231536 ) ) ;
#33694 = LINE ( 'NONE', #7912, #30568 ) ;
#33695 = CARTESIAN_POINT ( 'NONE',  ( -5.684927786827005392, 65.51297084251929448, 1.524000000000005572 ) ) ;
#33696 = CARTESIAN_POINT ( 'NONE',  ( 3.191397606779386109, -14.26579101578730224, 3.890870127686782087 ) ) ;
#33697 = CARTESIAN_POINT ( 'NONE',  ( 4.548929788228058158, 119.7344140837147819, -0.3435137807816314726 ) ) ;
#33698 = CARTESIAN_POINT ( 'NONE',  ( -9.616121018674380849, 118.2964180356302961, 0.4479623223841152635 ) ) ;
#33699 = ADVANCED_FACE ( 'NONE', ( #9467 ), #15363, .T. ) ;
#33700 = CARTESIAN_POINT ( 'NONE',  ( -4.062624110921462695, 30.12807731062649452, 3.861355649616186270 ) ) ;
#33701 = AXIS2_PLACEMENT_3D ( 'NONE', #40143, #10935, #29601 ) ;
#33702 = DIRECTION ( 'NONE',  ( 0.7517731442105899387, -0.6594218222380295868, -3.321276712443281495E-16 ) ) ;
#33703 = ORIENTED_EDGE ( 'NONE', *, *, #14042, .T. ) ;
#33704 = CARTESIAN_POINT ( 'NONE',  ( -3.055407127328060746, 104.6144662015402247, -4.375668876421388909 ) ) ;
#33705 = CARTESIAN_POINT ( 'NONE',  ( 4.901850132730561249, -15.30225767492697564, -0.5056678198325348372 ) ) ;
#33706 = CARTESIAN_POINT ( 'NONE',  ( -12.49437611722099994, 122.1796674805547980, 1.295212323302053159 ) ) ;
#33707 = CARTESIAN_POINT ( 'NONE',  ( -3.594857975007920814, -7.703025367003809798, -2.923569511714296798 ) ) ;
#33708 = ORIENTED_EDGE ( 'NONE', *, *, #37510, .F. ) ;
#33709 = EDGE_CURVE ( 'NONE', #17866, #36699, #37800, .T. ) ;
#33710 = ORIENTED_EDGE ( 'NONE', *, *, #16668, .F. ) ;
#33711 = DIRECTION ( 'NONE',  ( 1.011795553208986377E-16, 1.000000000000000000, -0.000000000000000000 ) ) ;
#33712 = CARTESIAN_POINT ( 'NONE',  ( 2.364009027793788853, 119.4803856251332945, 0.6315868319338826531 ) ) ;
#33713 =( NAMED_UNIT ( * ) SI_UNIT ( $, .STERADIAN. ) SOLID_ANGLE_UNIT ( ) );
#33714 = CARTESIAN_POINT ( 'NONE',  ( -16.69554899298730177, 147.2809512400332608, 1.108146210772844809 ) ) ;
#33715 = CARTESIAN_POINT ( 'NONE',  ( -46.04356016636307203, 20.98312584903309386, 4.505114195460657278 ) ) ;
#33716 = CARTESIAN_POINT ( 'NONE',  ( 0.01023306027083611264, 119.5380416804913324, -0.5121041807152043601 ) ) ;
#33717 = CARTESIAN_POINT ( 'NONE',  ( -10.23541510771069696, 120.3038588096988803, -1.551695437301547020 ) ) ;
#33718 = DIRECTION ( 'NONE',  ( 0.000000000000000000, 1.000000000000000000, 0.000000000000000000 ) ) ;
#33719 = CARTESIAN_POINT ( 'NONE',  ( 4.269777116393453475, 118.2237272103456007, -0.2881531109393317136 ) ) ;
#33720 = CARTESIAN_POINT ( 'NONE',  ( 5.897637645108018134, 121.3687970875902806, -0.2476274089428440461 ) ) ;
#33721 = ORIENTED_EDGE ( 'NONE', *, *, #4742, .T. ) ;
#33722 = CARTESIAN_POINT ( 'NONE',  ( 3.283982329611080608, -15.09957111342241731, 3.272784416514652239 ) ) ;
#33723 = EDGE_CURVE ( 'NONE', #20581, #40888, #35123, .T. ) ;
#33724 = CARTESIAN_POINT ( 'NONE',  ( -4.815275531776046947, 117.4047736241515736, 1.012442419610674271 ) ) ;
#33725 = EDGE_CURVE ( 'NONE', #42131, #37617, #7903, .T. ) ;
#33726 = CARTESIAN_POINT ( 'NONE',  ( -58.01460528358251878, 0.4727233027791988285, 0.8404818439586951850 ) ) ;
#33727 = AXIS2_PLACEMENT_3D ( 'NONE', #8065, #37666, #2319 ) ;
#33728 = CARTESIAN_POINT ( 'NONE',  ( 4.623297697159335584, 3.588818502778304609, 0.3943307014320480697 ) ) ;
#33729 = CARTESIAN_POINT ( 'NONE',  ( 16.06787389343314132, 149.3012944676311804, 2.013231008103361308 ) ) ;
#33730 = CARTESIAN_POINT ( 'NONE',  ( -2.475166694215277907, 30.06136823196653296, 2.243632805404280450 ) ) ;
#33731 = CARTESIAN_POINT ( 'NONE',  ( -3.106711772599575649, 110.6400929099055332, 3.287732168264224430 ) ) ;
#33732 = CARTESIAN_POINT ( 'NONE',  ( -4.012847786888796620, 11.73797844546971270, -2.294585225469591983 ) ) ;
#33733 = CARTESIAN_POINT ( 'NONE',  ( 15.21722582537762847, 143.4245298570049840, 0.3558394363636830926 ) ) ;
#33734 = CARTESIAN_POINT ( 'NONE',  ( -8.576171974424218192, 74.02775907367175989, -1.523999999999996913 ) ) ;
#33735 = CARTESIAN_POINT ( 'NONE',  ( -56.42856387642239469, 3.193865871111076338, -9.978765949893178940E-15 ) ) ;
#33736 = CARTESIAN_POINT ( 'NONE',  ( -2.166455499162651233, 116.2749100498806172, -0.2279745749322064641 ) ) ;
#33737 = DIRECTION ( 'NONE',  ( -5.188838149069471174E-16, 1.699382548006136313E-16, 1.000000000000000000 ) ) ;
#33738 = DIRECTION ( 'NONE',  ( 1.000000000000000000, 0.000000000000000000, -3.414809992080326065E-16 ) ) ;
#33739 = CARTESIAN_POINT ( 'NONE',  ( -1.814775304374550924, 106.5834530906598445, 4.954023504585296500 ) ) ;
#33740 = CARTESIAN_POINT ( 'NONE',  ( -9.712308604790303335, 65.53852105402241079, 1.524000000000003352 ) ) ;
#33741 = CARTESIAN_POINT ( 'NONE',  ( 6.696816702757251605, -2.959147833993511778, 5.158690622954519078 ) ) ;
#33742 = CARTESIAN_POINT ( 'NONE',  ( -23.91048590848665967, 81.84235438443283783, 1.269999999999992912 ) ) ;
#33743 = LINE ( 'NONE', #7542, #38893 ) ;
#33744 = CARTESIAN_POINT ( 'NONE',  ( -58.83227707057486811, -0.08366279997995551554, -1.533110566128066119E-14 ) ) ;
#33745 = DIRECTION ( 'NONE',  ( 0.5149185422762213582, -0.8572391118119444542, -8.916573780366528208E-15 ) ) ;
#33746 = CARTESIAN_POINT ( 'NONE',  ( -13.35275951139071005, 156.9675713949798421, 0.1105600748258541571 ) ) ;
#33747 = ORIENTED_EDGE ( 'NONE', *, *, #24850, .T. ) ;
#33748 = CARTESIAN_POINT ( 'NONE',  ( -56.90590057130552282, 4.418898835881354792, -2.427662546266534438 ) ) ;
#33749 = CARTESIAN_POINT ( 'NONE',  ( -6.992180608686842547, 121.9518168112129644, -0.1549296657180008197 ) ) ;
#33750 = ORIENTED_EDGE ( 'NONE', *, *, #3337, .T. ) ;
#33751 = CARTESIAN_POINT ( 'NONE',  ( -47.61073963480660609, 19.67761866751718713, -5.209507068503004490 ) ) ;
#33752 = CARTESIAN_POINT ( 'NONE',  ( -9.083767709417969627, 124.1603612693012053, -0.1367774190269939183 ) ) ;
#33753 = CARTESIAN_POINT ( 'NONE',  ( 4.983883817524661808, -15.00518790705197780, 4.081033524500047527 ) ) ;
#33754 = CARTESIAN_POINT ( 'NONE',  ( -9.293546136053135953, 157.2521837264336853, 1.575842917768122797 ) ) ;
#33755 = CARTESIAN_POINT ( 'NONE',  ( 10.68516669180060319, 157.9381250348597234, 0.6779181152352151685 ) ) ;
#33756 = CARTESIAN_POINT ( 'NONE',  ( 22.27457866854806667, 149.8733841865972920, -0.8555749715664360266 ) ) ;
#33757 = CARTESIAN_POINT ( 'NONE',  ( -3.290491044589036740, 30.52917213649525507, -3.264312889705288878 ) ) ;
#33758 = CARTESIAN_POINT ( 'NONE',  ( -22.49140923449514418, 150.7830971219523519, -0.7772193431698345423 ) ) ;
#33759 = CARTESIAN_POINT ( 'NONE',  ( -52.42485476335930628, 12.17260451344640693, -4.286044700273143881 ) ) ;
#33760 = CARTESIAN_POINT ( 'NONE',  ( 4.812098290572522252, 117.4080384897477813, 1.196841167122759897 ) ) ;
#33761 = VERTEX_POINT ( 'NONE', #2033 ) ;
#33762 = CIRCLE ( 'NONE', #11998, 0.2539999999999931202 ) ;
#33763 = CARTESIAN_POINT ( 'NONE',  ( -8.771991783980059409, 117.8544350838303103, 0.2656743787463436979 ) ) ;
#33764 = CARTESIAN_POINT ( 'NONE',  ( -12.98417868877910131, 125.9520529675768898, 1.303718779035868192 ) ) ;
#33765 = CARTESIAN_POINT ( 'NONE',  ( -57.60835131062518855, 1.351182788547599545, -1.295948770129724315 ) ) ;
#33766 = CARTESIAN_POINT ( 'NONE',  ( 19.87863739466932600, 147.4002846799066333, -1.728157425434577288 ) ) ;
#33767 = CARTESIAN_POINT ( 'NONE',  ( -0.2718671964776636085, -13.46374167387040366, -0.9358251418597670623 ) ) ;
#33768 = CARTESIAN_POINT ( 'NONE',  ( -16.99346516877630719, 153.7580772870718988, -2.083520914717074124 ) ) ;
#33769 = CARTESIAN_POINT ( 'NONE',  ( -48.08949201794742123, 19.91830422262442468, -5.194343260851647770 ) ) ;
#33770 = CARTESIAN_POINT ( 'NONE',  ( -8.519412162535127564, 69.40335734044576554, 1.270000000000003348 ) ) ;
#33771 = CARTESIAN_POINT ( 'NONE',  ( 0.01887828017110892292, 156.5412816204240301, -0.9447463363288812754 ) ) ;
#33772 = DIRECTION ( 'NONE',  ( -0.4849315768086451817, -0.8745520943968297933, 3.311806702191035794E-15 ) ) ;
#33773 = ORIENTED_EDGE ( 'NONE', *, *, #10577, .F. ) ;
#33774 = CARTESIAN_POINT ( 'NONE',  ( -10.38552121992541366, 122.0805278159965610, -1.592441429402149833 ) ) ;
#33775 = CARTESIAN_POINT ( 'NONE',  ( 4.747814429275453385, -15.55672444834840817, 1.946379828023123482 ) ) ;
#33776 = CARTESIAN_POINT ( 'NONE',  ( -19.86616884172038766, 72.62886460123898758, 1.269999999999996687 ) ) ;
#33777 = CARTESIAN_POINT ( 'NONE',  ( -4.535012393063357017, 118.1058069998952362, -0.6732513337841837808 ) ) ;
#33778 = EDGE_CURVE ( 'NONE', #41143, #10068, #33762, .T. ) ;
#33779 = CARTESIAN_POINT ( 'NONE',  ( -52.30895062419047292, 13.66434875625866674, -4.401212925246500873 ) ) ;
#33780 = FACE_OUTER_BOUND ( 'NONE', #15839, .T. ) ;
#33781 = CARTESIAN_POINT ( 'NONE',  ( 18.11471409803301214, 146.9188445454784357, 2.346026295494533453 ) ) ;
#33782 = LINE ( 'NONE', #10133, #10015 ) ;
#33783 = CARTESIAN_POINT ( 'NONE',  ( 16.86202032626302483, 155.2029898760372646, 0.3369432954968345495 ) ) ;
#33784 = CARTESIAN_POINT ( 'NONE',  ( -8.412017540776835389, 12.59877214424737524, 0.8828606482577823211 ) ) ;
#33785 = CARTESIAN_POINT ( 'NONE',  ( -0.006534791579925431325, 156.3267223255430167, 0.3270276925529296275 ) ) ;
#33786 = AXIS2_PLACEMENT_3D ( 'NONE', #10296, #10919, #30304 ) ;
#33787 = CARTESIAN_POINT ( 'NONE',  ( 15.42041356977095745, 121.5363848317736739, -0.5399810379570647578 ) ) ;
#33788 = CARTESIAN_POINT ( 'NONE',  ( -41.23752580366539888, 23.26788267949599742, -1.524000000000005128 ) ) ;
#33789 = CARTESIAN_POINT ( 'NONE',  ( 14.73199999999999932, 57.78500000000000369, 4.848162602465631106E-15 ) ) ;
#33790 = CARTESIAN_POINT ( 'NONE',  ( -57.84361080044246251, 0.8513586351276830611, 1.093731309501891458 ) ) ;
#33791 = CARTESIAN_POINT ( 'NONE',  ( -1.817820247522510924, 116.4909138135563040, 0.03564457049243165837 ) ) ;
#33792 = ORIENTED_EDGE ( 'NONE', *, *, #32083, .T. ) ;
#33793 = CARTESIAN_POINT ( 'NONE',  ( -46.93986413309943373, 25.37947832266650039, -1.074976477481977222 ) ) ;
#33794 = CARTESIAN_POINT ( 'NONE',  ( 5.842028984958227866, 121.2385196568167203, -0.2395641771394423913 ) ) ;
#33795 = CARTESIAN_POINT ( 'NONE',  ( -46.81030548986653628, 25.80411194895076221, -1.573461678945251130 ) ) ;
#33796 = ORIENTED_EDGE ( 'NONE', *, *, #15991, .F. ) ;
#33797 = CARTESIAN_POINT ( 'NONE',  ( 0.1233530899022908384, 118.7629491485454025, -1.274984814944074785 ) ) ;
#33798 = CARTESIAN_POINT ( 'NONE',  ( -15.59067940631276272, 147.5518517437054982, -0.7624272054715743874 ) ) ;
#33799 = CARTESIAN_POINT ( 'NONE',  ( 2.939725130288969979, -14.94165859211278580, 5.651657094137466864 ) ) ;
#33800 = CARTESIAN_POINT ( 'NONE',  ( -21.76596270643833364, 150.3096123636779566, 1.000581967439477360 ) ) ;
#33801 = CARTESIAN_POINT ( 'NONE',  ( -7.017589760824602507, 78.79342665089201603, -2.556811674275342394 ) ) ;
#33802 = CARTESIAN_POINT ( 'NONE',  ( 6.901437262003186746, 117.1762911274595496, 0.2238905109288660267 ) ) ;
#33803 = VERTEX_POINT ( 'NONE', #33992 ) ;
#33804 = CARTESIAN_POINT ( 'NONE',  ( 3.102408547967445696, -0.5812848888516047863, -3.453265078539196509 ) ) ;
#33805 = CARTESIAN_POINT ( 'NONE',  ( -14.89944180985308364, 120.3262451489332818, -0.3144022614128132997 ) ) ;
#33806 = LINE ( 'NONE', #11206, #3922 ) ;
#33807 = CARTESIAN_POINT ( 'NONE',  ( -36.79765817521327165, 27.64956762128696610, -1.524000000000003574 ) ) ;
#33808 = EDGE_LOOP ( 'NONE', ( #25431, #36592, #15813, #29113 ) ) ;
#33809 = CARTESIAN_POINT ( 'NONE',  ( 5.474781159379864093, 119.6919804704018588, 1.105622938617728090 ) ) ;
#33810 = CARTESIAN_POINT ( 'NONE',  ( 4.064497669612420871, 2.951628549105334454, 2.233594334442648766 ) ) ;
#33811 = CARTESIAN_POINT ( 'NONE',  ( 9.366440581936233301, 118.7255599110314961, 1.127239873969282824 ) ) ;
#33812 = CARTESIAN_POINT ( 'NONE',  ( -49.24775882307794461, 17.43196194297031454, -5.046047204416971965 ) ) ;
#33813 = AXIS2_PLACEMENT_3D ( 'NONE', #40433, #17611, #30612 ) ;
#33814 = CARTESIAN_POINT ( 'NONE',  ( 20.18437654629502020, 141.3454246894093274, -1.633934361538418090 ) ) ;
#33815 = CARTESIAN_POINT ( 'NONE',  ( -4.567530434605131084, -10.44214056487004250, 0.7003524306260878740 ) ) ;
#33816 = CARTESIAN_POINT ( 'NONE',  ( -15.23381565553120254, 121.5932973536894934, -1.241876992062232121 ) ) ;
#33817 = VERTEX_POINT ( 'NONE', #18398 ) ;
#33818 = AXIS2_PLACEMENT_3D ( 'NONE', #18778, #9216, #32626 ) ;
#33819 = CARTESIAN_POINT ( 'NONE',  ( -5.280870373041201660, 121.3253820001177417, 0.01155303659100765171 ) ) ;
#33820 = CARTESIAN_POINT ( 'NONE',  ( 3.039728791924208195, -15.34324946256290723, 5.681930179901951483 ) ) ;
#33821 = CARTESIAN_POINT ( 'NONE',  ( -25.83700401581416628, 71.09321415394998667, 1.523999999999994026 ) ) ;
#33822 = CARTESIAN_POINT ( 'NONE',  ( -5.084954045839870318, 114.9389534559779946, -1.737685838023535601 ) ) ;
#33823 = ORIENTED_EDGE ( 'NONE', *, *, #30517, .T. ) ;
#33824 = CARTESIAN_POINT ( 'NONE',  ( 12.25516334840909138, 122.6846661264431191, 1.808440497450061413 ) ) ;
#33825 = DIRECTION ( 'NONE',  ( -0.1565721916417935344, -0.9876665170007969952, 8.659954811668054921E-17 ) ) ;
#33826 = CARTESIAN_POINT ( 'NONE',  ( -29.14852920558610450, 63.08767140637714022, -1.270000000000006013 ) ) ;
#33827 = EDGE_CURVE ( 'NONE', #1007, #11738, #27996, .T. ) ;
#33828 = AXIS2_PLACEMENT_3D ( 'NONE', #21975, #15382, #37343 ) ;
#33829 = CARTESIAN_POINT ( 'NONE',  ( -3.136615966272743083, 159.3365417412370562, 0.7296721229192901781 ) ) ;
#33830 = CARTESIAN_POINT ( 'NONE',  ( 8.344183819546742598, 4.025392264050483782, -1.191670311180863528 ) ) ;
#33831 = CARTESIAN_POINT ( 'NONE',  ( 5.192366003377009598, 121.0352659167314755, 0.5503205103620257832 ) ) ;
#33832 = CARTESIAN_POINT ( 'NONE',  ( -18.83202234259777086, 80.34319284215895607, -1.270000000000003126 ) ) ;
#33833 = CARTESIAN_POINT ( 'NONE',  ( 18.44051311885884914, 154.1649927243852858, -0.3121108635588941138 ) ) ;
#33834 = FACE_OUTER_BOUND ( 'NONE', #22608, .T. ) ;
#33835 = CARTESIAN_POINT ( 'NONE',  ( -57.58811225465035477, 1.394777090889576909, 1.315424955976544297 ) ) ;
#33836 = FACE_OUTER_BOUND ( 'NONE', #24000, .T. ) ;
#33837 = CARTESIAN_POINT ( 'NONE',  ( -57.00508801794419611, 2.691366720778187727, 1.977812201481533583 ) ) ;
#33838 = CARTESIAN_POINT ( 'NONE',  ( -58.61692577976591423, -0.2667954925353184237, 0.4132871861646182365 ) ) ;
#33839 = CARTESIAN_POINT ( 'NONE',  ( -4.242438329162251165, 118.2242328442825681, 0.3186281974751150048 ) ) ;
#33840 = CARTESIAN_POINT ( 'NONE',  ( 4.163769306296988937, 111.0901538136045161, -3.043919495886841631 ) ) ;
#33841 = AXIS2_PLACEMENT_3D ( 'NONE', #8108, #21082, #14275 ) ;
#33842 = VERTEX_POINT ( 'NONE', #8001 ) ;
#33843 = CARTESIAN_POINT ( 'NONE',  ( -46.07906060731711761, 24.80782705053048076, 1.769089518195985367 ) ) ;
#33844 = CARTESIAN_POINT ( 'NONE',  ( 4.224406003510333463, 119.3195559688346066, -0.7598301222401262489 ) ) ;
#33845 = CARTESIAN_POINT ( 'NONE',  ( -5.246745461248100817, 116.0761519159950552, -1.241752167516083194 ) ) ;
#33846 = CARTESIAN_POINT ( 'NONE',  ( 4.397138658150465673, 118.1792182539645353, 0.5669217176520113810 ) ) ;
#33847 = CARTESIAN_POINT ( 'NONE',  ( -8.969937932052687302, 123.1852847016406685, -0.8267063328025512359 ) ) ;
#33848 = SURFACE_STYLE_USAGE ( .BOTH. , #37043 ) ;
#33849 = CARTESIAN_POINT ( 'NONE',  ( 4.410581516669115132, 117.9496053154420423, -1.006313971990577372 ) ) ;
#33850 = ORIENTED_EDGE ( 'NONE', *, *, #30501, .T. ) ;
#33851 = CARTESIAN_POINT ( 'NONE',  ( 3.580579253266004347, 108.6681208952157078, -3.986884027299105071 ) ) ;
#33852 = CARTESIAN_POINT ( 'NONE',  ( -0.5759676376930302766, 120.3589971203204669, -0.3694376532493067189 ) ) ;
#33853 = CARTESIAN_POINT ( 'NONE',  ( 4.141126571459865069, 104.6144662015457243, 4.161112031276615220 ) ) ;
#33854 = CARTESIAN_POINT ( 'NONE',  ( -3.321756749363752537, 31.07797388775926350, -0.5319413560150946241 ) ) ;
#33855 = CARTESIAN_POINT ( 'NONE',  ( -48.02918200001371218, 19.49203439357020429, 5.381710552009359994 ) ) ;
#33856 = CARTESIAN_POINT ( 'NONE',  ( -13.59405114508080992, 150.2694781165900793, -0.07689127809379422973 ) ) ;
#33857 = CARTESIAN_POINT ( 'NONE',  ( 4.980754117605273201, 117.5239965563486919, 0.8160915654990145152 ) ) ;
#33858 = CARTESIAN_POINT ( 'NONE',  ( 22.92073667220923738, 148.8788797244430384, 1.430292205038965037 ) ) ;
#33859 = CARTESIAN_POINT ( 'NONE',  ( 6.059261036834406866, 53.58606249999999704, -5.016499999999999737 ) ) ;
#33861 = CARTESIAN_POINT ( 'NONE',  ( 21.51828093163809896, 145.9698620541949765, -1.394984360948490210 ) ) ;
#33860 = CARTESIAN_POINT ( 'NONE',  ( 3.178195937486941958, -14.44740043277138675, 1.484392166672811930 ) ) ;
#33862 = CARTESIAN_POINT ( 'NONE',  ( -0.5200570697821880195, 119.3183582894065893, 0.5597423419424876201 ) ) ;
#33863 = CARTESIAN_POINT ( 'NONE',  ( -0.4659799999662124215, -3.540968264561009882, -0.8578381542037093466 ) ) ;
#33864 = CARTESIAN_POINT ( 'NONE',  ( -23.01936977803475770, 148.9204423966469335, -1.315221278248082548 ) ) ;
#33865 = AXIS2_PLACEMENT_3D ( 'NONE', #16022, #33078, #29450 ) ;
#33866 = CARTESIAN_POINT ( 'NONE',  ( -0.2236011429256814231, 15.24623788552754888, -0.9474642044971398613 ) ) ;
#33867 = EDGE_LOOP ( 'NONE', ( #17810, #10445, #9815, #21361 ) ) ;
#33868 = CARTESIAN_POINT ( 'NONE',  ( -48.50421218116022004, 14.67712143704007133, 0.4105607596417898408 ) ) ;
#33869 = APPLICATION_PROTOCOL_DEFINITION ( 'draft international standard', 'automotive_design', 1998, #25165 ) ;
#33870 = CARTESIAN_POINT ( 'NONE',  ( -7.092669859378217367, 121.9239394581621809, 0.2697480494961537190 ) ) ;
#33871 = CARTESIAN_POINT ( 'NONE',  ( 4.995837928452414367, -12.01622098921958859, 1.211524600846092481 ) ) ;
#33872 = CARTESIAN_POINT ( 'NONE',  ( 4.353257824593153025, 120.2039194668847699, -0.6262808803686855663 ) ) ;
#33873 = ORIENTED_EDGE ( 'NONE', *, *, #28977, .T. ) ;
#33874 = CARTESIAN_POINT ( 'NONE',  ( 3.605593953823826414, 115.7029500407100926, 1.621980936835669018 ) ) ;
#33875 = B_SPLINE_CURVE_WITH_KNOTS ( 'NONE', 3,
 ( #25141, #38145, #5778, #7548, #31743, #28548 ),
 .UNSPECIFIED., .F., .F.,
 ( 4, 2, 4 ),
 ( -7.295512689534840788E-06, 0.0003601880853872708229, 0.0007276716834640765052 ),
 .UNSPECIFIED. ) ;
#33876 = EDGE_CURVE ( 'NONE', #41261, #27727, #31619, .T. ) ;
#33877 = CARTESIAN_POINT ( 'NONE',  ( 3.370512099616890467, -13.86485436517860492, 3.147780574041331825 ) ) ;
#33878 = FACE_OUTER_BOUND ( 'NONE', #37284, .T. ) ;
#33879 = EDGE_CURVE ( 'NONE', #34211, #17903, #34847, .T. ) ;
#33880 = CARTESIAN_POINT ( 'NONE',  ( 15.26897697690599109, 148.0131224598485744, 0.1773810520481279573 ) ) ;
#33881 = EDGE_LOOP ( 'NONE', ( #37117, #16796, #38963, #4832 ) ) ;
#33882 = CARTESIAN_POINT ( 'NONE',  ( 12.93098116229895211, 122.2940260782629451, 1.802317002068888785 ) ) ;
#33883 = CARTESIAN_POINT ( 'NONE',  ( 3.410149960233146427, 109.2372012348956645, 3.913055101880209552 ) ) ;
#33884 = CARTESIAN_POINT ( 'NONE',  ( -13.85159022459153988, 12.96416000000000146, 5.016499999999999737 ) ) ;
#33885 = CARTESIAN_POINT ( 'NONE',  ( 0.01289612358321986542, 159.5048567107479585, -0.6453747585945881493 ) ) ;
#33886 = CARTESIAN_POINT ( 'NONE',  ( 22.65693159617090657, 137.2763855621842026, 0.2353725067100886914 ) ) ;
#33887 = CARTESIAN_POINT ( 'NONE',  ( -3.174366308152011040, 69.94346620154573202, -0.06343139340882729404 ) ) ;
#33888 = CARTESIAN_POINT ( 'NONE',  ( 1.727570783967031787, -15.53207390529406950, 5.484086197889097569 ) ) ;
#33889 = CARTESIAN_POINT ( 'NONE',  ( 10.54112285291074969, 57.14999999999387370, 5.016499999999999737 ) ) ;
#33890 = CARTESIAN_POINT ( 'NONE',  ( -3.113414239748029111, 30.98679946927233431, 0.04088859964249514506 ) ) ;
#33891 = CARTESIAN_POINT ( 'NONE',  ( 9.223174309219125178, 157.2521837264336853, 1.945851059610182565 ) ) ;
#33892 = ORIENTED_EDGE ( 'NONE', *, *, #24021, .T. ) ;
#33893 = CARTESIAN_POINT ( 'NONE',  ( -6.605212570472872358, 13.46189590645272460, 5.224192399652773489 ) ) ;
#33894 = CARTESIAN_POINT ( 'NONE',  ( -8.578767457482950221, 118.6581505231196161, -1.156225727184389207 ) ) ;
#33895 = CARTESIAN_POINT ( 'NONE',  ( -2.027571083617168313, 109.8863472468248119, -3.714074494666526505 ) ) ;
#33896 = DIRECTION ( 'NONE',  ( 0.6294287539884060312, 0.7770581983690815209, 1.945484789722797568E-16 ) ) ;
#33897 = FACE_OUTER_BOUND ( 'NONE', #39321, .T. ) ;
#33898 = CARTESIAN_POINT ( 'NONE',  ( -0.003708075273252911530, 123.1683257372384901, 0.1855672496570451302 ) ) ;
#33899 = B_SPLINE_CURVE_WITH_KNOTS ( 'NONE', 3,
 ( #9835, #693, #35626, #39234, #10252, #36466, #29431, #25807, #16211, #35838, #32630, #36257, #13665, #16006 ),
 .UNSPECIFIED., .F., .F.,
 ( 4, 1, 1, 1, 2, 1, 1, 1, 1, 1, 4 ),
 ( 0.2031000000004874739, 0.2063375000004613602, 0.2095750000004352187, 0.2128125000004091050, 0.2160500000003829635, 0.2667374999999738705, 0.3174249999995648608, 0.3681124999991557400, 0.4187999999987466193, 0.5201749999979284889, 0.6215499999971102474 ),
 .UNSPECIFIED. ) ;
#33900 = CIRCLE ( 'NONE', #15515, 3.175000000000001155 ) ;
#33901 = CARTESIAN_POINT ( 'NONE',  ( 0.7007450612751181529, 9.901275517365906609, -4.597291952374415125 ) ) ;
#33902 = CARTESIAN_POINT ( 'NONE',  ( -28.65049350906917880, 77.81814547195517662, -1.524000000000008015 ) ) ;
#33903 = CARTESIAN_POINT ( 'NONE',  ( -5.206518307116178690, 115.6909491485453003, 1.025009323720317500 ) ) ;
#33904 = CARTESIAN_POINT ( 'NONE',  ( 3.119424175201863214, -14.34824051949108714, 4.229366443754182470 ) ) ;
#33905 = EDGE_CURVE ( 'NONE', #25505, #31858, #20798, .T. ) ;
#33906 = CARTESIAN_POINT ( 'NONE',  ( 4.368052411777142652, 123.4689364668338385, 0.008193521294100057292 ) ) ;
#33907 = CARTESIAN_POINT ( 'NONE',  ( -3.958300029084214522, 28.23836431654050472, 1.224951011016432778 ) ) ;
#33908 = CARTESIAN_POINT ( 'NONE',  ( -2.027701166914974706, 115.7029486569566785, 1.637676004427128351 ) ) ;
#33909 = EDGE_LOOP ( 'NONE', ( #6917, #17663, #15823, #12643 ) ) ;
#33910 = CARTESIAN_POINT ( 'NONE',  ( -4.648735762212839795, 104.6144662015457527, -1.307085752955095437 ) ) ;
#33911 = CARTESIAN_POINT ( 'NONE',  ( 3.970714270704740922, -15.74271870963887743, 3.976543152134710990 ) ) ;
#33912 = CARTESIAN_POINT ( 'NONE',  ( -17.13393749618838413, 131.5760549582342094, 1.627836260134054802 ) ) ;
#33913 = CARTESIAN_POINT ( 'NONE',  ( -0.9745549951769645336, 13.24125360461694001, -0.07243667530571006041 ) ) ;
#33914 = VERTEX_POINT ( 'NONE', #1621 ) ;
#33915 = ORIENTED_EDGE ( 'NONE', *, *, #4507, .T. ) ;
#33916 = DIRECTION ( 'NONE',  ( -1.011795553208986377E-16, -1.000000000000000000, 0.000000000000000000 ) ) ;
#33917 = CARTESIAN_POINT ( 'NONE',  ( 2.302803873444530858, 118.9955205646042344, 0.7292456921539738346 ) ) ;
#33918 = CARTESIAN_POINT ( 'NONE',  ( -5.165015969722906775, 120.6777149489875569, 0.5489573293230839424 ) ) ;
#33919 = CARTESIAN_POINT ( 'NONE',  ( -42.38674052981945550, 22.29968528929560989, 1.779698276446733507 ) ) ;
#33920 = CARTESIAN_POINT ( 'NONE',  ( 4.619030643355426236, 118.0409184362119532, -0.6363634065985189769 ) ) ;
#33921 = CARTESIAN_POINT ( 'NONE',  ( 17.20821608673143999, 140.2562023718666353, -1.644530994948828706 ) ) ;
#33922 = CARTESIAN_POINT ( 'NONE',  ( -19.97852701226068461, 149.8444905389382882, -2.417717604095676265 ) ) ;
#33923 = CARTESIAN_POINT ( 'NONE',  ( -11.24191166894635074, 82.34025985790688651, -1.523999999999999799 ) ) ;
#33924 = ORIENTED_EDGE ( 'NONE', *, *, #2760, .F. ) ;
#33925 = EDGE_CURVE ( 'NONE', #24827, #25936, #31188, .T. ) ;
#33926 = CARTESIAN_POINT ( 'NONE',  ( 4.157985977180885584, 118.2391351103022430, -0.2336046903670694896 ) ) ;
#33927 = CARTESIAN_POINT ( 'NONE',  ( 9.286476516977916873, 123.9149913687586064, -0.2326040378870055936 ) ) ;
#33928 = ORIENTED_EDGE ( 'NONE', *, *, #27913, .T. ) ;
#33929 = CARTESIAN_POINT ( 'NONE',  ( 3.092086460852839114, -14.79905751219236265, 3.633802299706017980 ) ) ;
#33930 = AXIS2_PLACEMENT_3D ( 'NONE', #5443, #6277, #25015 ) ;
#33931 = CIRCLE ( 'NONE', #22328, 2.540000000000000480 ) ;
#33932 = CARTESIAN_POINT ( 'NONE',  ( 11.66725022230187214, 55.42194143536249840, -5.016499999999354031 ) ) ;
#33933 = CARTESIAN_POINT ( 'NONE',  ( -57.40739589891827421, 2.334961046639910442, 1.895125133209311308 ) ) ;
#33934 = EDGE_CURVE ( 'NONE', #40008, #2172, #13452, .T. ) ;
#33935 = CARTESIAN_POINT ( 'NONE',  ( 0.5082173563136543892, -13.24086043563247728, -4.610200172643777350 ) ) ;
#33936 = CARTESIAN_POINT ( 'NONE',  ( 10.62607977745477505, 123.8807653058400575, 1.354828998092944659 ) ) ;
#33937 = CARTESIAN_POINT ( 'NONE',  ( -3.222454021317843864, 28.56592918162606054, 1.039686905332308342 ) ) ;
#33938 = CARTESIAN_POINT ( 'NONE',  ( -0.6941271473899978117, 106.1608668108878817, 5.200699783222979988 ) ) ;
#33939 = CARTESIAN_POINT ( 'NONE',  ( -4.478778176974228309, 3.316883148187759645, 1.141857468124592101 ) ) ;
#33940 = CARTESIAN_POINT ( 'NONE',  ( 2.896036792256140302, 156.0891579660883508, 0.1428477814196380258 ) ) ;
#33941 = CARTESIAN_POINT ( 'NONE',  ( -11.62920297224754762, 55.59919541885980721, 5.016499999999892268 ) ) ;
#33942 = CARTESIAN_POINT ( 'NONE',  ( -56.90807066679607829, 2.849439543264234320, -1.873271221587442081 ) ) ;
#33943 = CARTESIAN_POINT ( 'NONE',  ( 2.180768841371605316, 116.2301253052036145, -0.09025952647190275957 ) ) ;
#33944 = FACE_OUTER_BOUND ( 'NONE', #17247, .T. ) ;
#33945 = DIRECTION ( 'NONE',  ( 5.188838149069472160E-16, -1.699382548006136559E-16, -1.000000000000000000 ) ) ;
#33946 = CARTESIAN_POINT ( 'NONE',  ( -1.205614202975156202, 106.0882118856389980, 5.200918596848653763 ) ) ;
#33947 = CARTESIAN_POINT ( 'NONE',  ( 14.60500000000000043, 71.11999999999999034, 1.904999999999990701 ) ) ;
#33948 = CARTESIAN_POINT ( 'NONE',  ( 7.077328715112659374, 6.763356510963684620, 4.580356461215433939 ) ) ;
#33949 = CARTESIAN_POINT ( 'NONE',  ( -5.177913976931286300, 57.14999999999999858, 5.372100000000003206 ) ) ;
#33950 = CARTESIAN_POINT ( 'NONE',  ( -23.43300365160793319, 82.12916405548841681, 1.269999999999993134 ) ) ;
#33951 = CARTESIAN_POINT ( 'NONE',  ( -58.18408008067591197, 1.689533369873860824, 0.1826487275623747131 ) ) ;
#33952 = EDGE_CURVE ( 'NONE', #10652, #7720, #37154, .T. ) ;
#33953 = CARTESIAN_POINT ( 'NONE',  ( 0.008700780990288231598, 121.2597428844645293, -0.4354226598342533783 ) ) ;
#33954 = CARTESIAN_POINT ( 'NONE',  ( -9.739177221546430729, 118.0756159837034716, 0.1634508798788867900 ) ) ;
#33955 = ORIENTED_EDGE ( 'NONE', *, *, #19071, .T. ) ;
#33956 = CARTESIAN_POINT ( 'NONE',  ( -56.01560174880540188, 6.374421267034191985, -2.942705720416971094 ) ) ;
#33957 = EDGE_CURVE ( 'NONE', #30054, #20091, #27787, .T. ) ;
#33958 = TOROIDAL_SURFACE ( 'NONE', #16252, 3.683000000000000718, 0.5080000000000000071 ) ;
#33959 = VERTEX_POINT ( 'NONE', #17774 ) ;
#33960 = CARTESIAN_POINT ( 'NONE',  ( -44.75127360237845409, 21.22985803518790604, -3.557274316436290995 ) ) ;
#33961 = CARTESIAN_POINT ( 'NONE',  ( -8.487687333566288572, 123.3253871723413368, -0.1696041924978711757 ) ) ;
#33962 = CARTESIAN_POINT ( 'NONE',  ( 2.853125897180512460, -15.37704012655945185, 5.752692477956393269 ) ) ;
#33963 = CARTESIAN_POINT ( 'NONE',  ( -13.44735859403588840, 121.7711344121973411, 1.154596522737721953 ) ) ;
#33964 = EDGE_CURVE ( 'NONE', #28056, #37511, #38314, .T. ) ;
#33965 = CARTESIAN_POINT ( 'NONE',  ( 18.94714202558204619, 128.6554162386474047, -0.8647899522199679057 ) ) ;
#33966 = CARTESIAN_POINT ( 'NONE',  ( -29.88361747175496319, 69.13349703878448338, 1.269999999999992024 ) ) ;
#33967 = CARTESIAN_POINT ( 'NONE',  ( -15.13553065988589275, 156.1345691653134509, -0.5893329488795887583 ) ) ;
#33968 = CARTESIAN_POINT ( 'NONE',  ( -49.52080500732375867, 17.04929614760187917, -5.023366860225153552 ) ) ;
#33969 = ORIENTED_EDGE ( 'NONE', *, *, #13568, .F. ) ;
#33970 = CARTESIAN_POINT ( 'NONE',  ( 6.059261036834406866, 56.81853847168529370, 4.948064083792229617 ) ) ;
#33971 = CARTESIAN_POINT ( 'NONE',  ( -10.63443090528977031, 122.8495954190337898, 1.101905667251144472 ) ) ;
#33972 = CARTESIAN_POINT ( 'NONE',  ( -55.84895358435638713, 5.076860723676236198, -2.553460122158255796 ) ) ;
#33973 = CARTESIAN_POINT ( 'NONE',  ( 7.611130975157075262, 119.9600249249614592, -1.076879093209133442 ) ) ;
#33974 = CARTESIAN_POINT ( 'NONE',  ( -12.03559625110899312, 156.5645100661158153, -1.882936990620205586 ) ) ;
#33975 = CARTESIAN_POINT ( 'NONE',  ( -45.82931853585289872, 22.14969803457954356, -3.600065900675656128 ) ) ;
#33976 = CARTESIAN_POINT ( 'NONE',  ( 0.7813136802278927151, 156.5584078035761593, -0.9574549430346843693 ) ) ;
#33977 = CARTESIAN_POINT ( 'NONE',  ( -15.77133435453296606, 146.5691041611200660, -0.3151487940933135334 ) ) ;
#33978 = EDGE_LOOP ( 'NONE', ( #36264, #29934, #42078, #7504 ) ) ;
#33979 = CARTESIAN_POINT ( 'NONE',  ( -5.554730375463081238, 156.7050554705274408, -1.852363956736410522 ) ) ;
#33980 = CARTESIAN_POINT ( 'NONE',  ( 4.466571682983457414, -15.50692525667736454, 1.643437993322231838 ) ) ;
#33981 = FACE_OUTER_BOUND ( 'NONE', #35640, .T. ) ;
#33982 = CARTESIAN_POINT ( 'NONE',  ( -4.342952997683876326, 118.1822044573729471, -0.6217259542595968691 ) ) ;
#33983 = CARTESIAN_POINT ( 'NONE',  ( -56.04137470801128273, 5.508142037592367757, -2.879222540163135058 ) ) ;
#33984 = CARTESIAN_POINT ( 'NONE',  ( -4.979023873620669782, 117.5329379046127656, 0.7799942829153793111 ) ) ;
#33985 = CARTESIAN_POINT ( 'NONE',  ( 5.064401052258119762, 119.9665122172617231, 0.9903757029826919522 ) ) ;
#33986 = CARTESIAN_POINT ( 'NONE',  ( -28.42835727709238114, 77.69497285144578314, 1.523999999999991806 ) ) ;
#33987 = CIRCLE ( 'NONE', #26486, 0.5556250000000014788 ) ;
#33988 = CIRCLE ( 'NONE', #12205, 0.5080000000000004512 ) ;
#33989 = CARTESIAN_POINT ( 'NONE',  ( 23.45022726768229404, 146.8469795362756258, 0.4427096500589556838 ) ) ;
#33990 = CARTESIAN_POINT ( 'NONE',  ( -0.4304388160753707671, 14.75877898171113145, 8.412599170943037663 ) ) ;
#33991 = CARTESIAN_POINT ( 'NONE',  ( -0.003052472355949370757, 120.8426702770480148, 0.1527581987772198835 ) ) ;
#33992 = CARTESIAN_POINT ( 'NONE',  ( -19.68500000000000227, 71.11999999999999034, -5.016499999999999737 ) ) ;
#33993 = EDGE_CURVE ( 'NONE', #14172, #537, #35667, .T. ) ;
#33994 = CARTESIAN_POINT ( 'NONE',  ( -46.47694366848682535, 20.52739116796101726, -4.723822614978507417 ) ) ;
#33995 = CARTESIAN_POINT ( 'NONE',  ( 4.799946221453406103, 115.6909491485452435, 1.474290515418332115 ) ) ;
#33996 = CARTESIAN_POINT ( 'NONE',  ( -57.70855261479918141, 1.142328357490882240, 1.228565355105990298 ) ) ;
#33997 = CARTESIAN_POINT ( 'NONE',  ( -23.44551923343654209, 146.8400249081559537, -0.3912800906488113073 ) ) ;
#33998 = ORIENTED_EDGE ( 'NONE', *, *, #37840, .F. ) ;
#33999 = CARTESIAN_POINT ( 'NONE',  ( -48.05877817626803505, 25.10121868647436472, -9.935001874592197936E-15 ) ) ;
#34000 = CARTESIAN_POINT ( 'NONE',  ( 5.827611813826044873, 121.2139407771506541, -0.2588721111321020674 ) ) ;
#34001 = CARTESIAN_POINT ( 'NONE',  ( -3.174366308152012817, 88.99346620154574339, -0.06343139340882730792 ) ) ;
#34002 = ORIENTED_EDGE ( 'NONE', *, *, #39644, .F. ) ;
#34003 = CARTESIAN_POINT ( 'NONE',  ( 0.6166252005165503425, 115.7029855507786209, -1.738059646771149547 ) ) ;
#34004 = CARTESIAN_POINT ( 'NONE',  ( -0.6320571215040977631, 120.9405031987692212, -0.1040377489725131110 ) ) ;
#34005 = CARTESIAN_POINT ( 'NONE',  ( 4.964329757808820354, -12.46733462535230785, 1.954119038396571417 ) ) ;
#34006 = CARTESIAN_POINT ( 'NONE',  ( -6.863242444369421769, 118.1252062928739832, 0.7545491157480666011 ) ) ;
#34007 = LINE ( 'NONE', #38033, #34265 ) ;
#34008 = CARTESIAN_POINT ( 'NONE',  ( 4.741236776273888509, 116.7839080817633430, 0.2126559219428779679 ) ) ;
#34009 = EDGE_CURVE ( 'NONE', #28646, #3540, #32038, .T. ) ;
#34010 = CARTESIAN_POINT ( 'NONE',  ( 5.959810334499592521, 155.3892724211786742, 0.1190911940436167188 ) ) ;
#34011 = ORIENTED_EDGE ( 'NONE', *, *, #3872, .F. ) ;
#34012 = CARTESIAN_POINT ( 'NONE',  ( 0.5005776846888100318, 19.73258526448893591, -0.8400667230076528380 ) ) ;
#34013 = B_SPLINE_CURVE_WITH_KNOTS ( 'NONE', 3,
 ( #18678, #24440, #18465, #11665 ),
 .UNSPECIFIED., .F., .F.,
 ( 4, 4 ),
 ( 0.000000000000000000, 0.0004246169644143726364 ),
 .UNSPECIFIED. ) ;
#34014 = CARTESIAN_POINT ( 'NONE',  ( -18.63389541082843337, 154.1203422869290023, -0.3962720605433150967 ) ) ;
#34015 = CARTESIAN_POINT ( 'NONE',  ( -41.61051026975745515, 22.90141404205858677, -1.547907765227501953 ) ) ;
#34016 = AXIS2_PLACEMENT_3D ( 'NONE', #29410, #39215, #464 ) ;
#34017 = ORIENTED_EDGE ( 'NONE', *, *, #34061, .F. ) ;
#34018 = CARTESIAN_POINT ( 'NONE',  ( -6.503981220335420706E-14, 66.64146620154573952, -9.408573323119121831E-18 ) ) ;
#34019 = ADVANCED_FACE ( 'NONE', ( #12654 ), #2667, .T. ) ;
#34020 = ORIENTED_EDGE ( 'NONE', *, *, #9989, .F. ) ;
#34021 = CARTESIAN_POINT ( 'NONE',  ( -3.222226742346633088, 117.5522224569482574, 0.6736568086485349438 ) ) ;
#34022 = CARTESIAN_POINT ( 'NONE',  ( 4.406646451516359697, -6.344046434980911364, 1.391598188203984288 ) ) ;
#34023 = CARTESIAN_POINT ( 'NONE',  ( 21.97492997893991884, 149.1257232373000647, 2.026018130409337648 ) ) ;
#34024 = CARTESIAN_POINT ( 'NONE',  ( -58.78565887484196395, -0.2971860671469456205, -0.1726678976672988974 ) ) ;
#34025 = CARTESIAN_POINT ( 'NONE',  ( 11.63724909022833387, 121.0393782313542346, -1.189926691809806814 ) ) ;
#34026 = CARTESIAN_POINT ( 'NONE',  ( -2.092221094934305192, 20.21789226318614041, 8.165053130886693822 ) ) ;
#34027 = CARTESIAN_POINT ( 'NONE',  ( -13.98195098595651942, 120.5923583732999873, -1.177051350580812894 ) ) ;
#34028 = CARTESIAN_POINT ( 'NONE',  ( 4.814618516084593125, 117.6401595242498530, -0.9373198651747913779 ) ) ;
#34029 = EDGE_LOOP ( 'NONE', ( #13259, #8609, #24846, #17458 ) ) ;
#34030 = CARTESIAN_POINT ( 'NONE',  ( -9.357997026032906618, 124.2740283646700306, 0.04730198213477326136 ) ) ;
#34031 = CARTESIAN_POINT ( 'NONE',  ( 2.292478802652971659, -15.50831694688660534, 5.896745190559482985 ) ) ;
#34032 = CARTESIAN_POINT ( 'NONE',  ( -6.401666570281882684, 64.12941061790216679, -1.269999999999994023 ) ) ;
#34033 = CARTESIAN_POINT ( 'NONE',  ( -0.1782324565444364795, 117.3993841991624834, -1.495935750720309265 ) ) ;
#34034 = ORIENTED_EDGE ( 'NONE', *, *, #23484, .T. ) ;
#34035 = CARTESIAN_POINT ( 'NONE',  ( 19.20654067994509262, 147.6776069388173767, 2.506343067704081218 ) ) ;
#34036 = LINE ( 'NONE', #31028, #18820 ) ;
#34037 = DIRECTION ( 'NONE',  ( -4.017660918040594346E-17, 1.000000000000000000, 2.376309959284834438E-19 ) ) ;
#34038 = CARTESIAN_POINT ( 'NONE',  ( -1.604275531929196363, 118.9836165220538504, 0.7112099450351576646 ) ) ;
#34039 = CARTESIAN_POINT ( 'NONE',  ( 7.658903097349539557, 3.149683656735901671, 3.518291596705641400 ) ) ;
#34040 = CARTESIAN_POINT ( 'NONE',  ( 15.86545709684687111, 148.0001117310855250, 1.424070646214982139 ) ) ;
#34041 = CARTESIAN_POINT ( 'NONE',  ( -13.85159022459153988, 12.96416000000000146, -5.016499999999999737 ) ) ;
#34042 = CARTESIAN_POINT ( 'NONE',  ( 1.391432384042537551, 159.5643428290674990, -0.4004207282219805486 ) ) ;
#34043 = DIRECTION ( 'NONE',  ( -0.9998004120163608288, 0.000000000000000000, -0.01997839162482749342 ) ) ;
#34044 = CARTESIAN_POINT ( 'NONE',  ( -56.13560805112248175, 4.477488644328690981, 2.380442300579769910 ) ) ;
#34045 = CARTESIAN_POINT ( 'NONE',  ( -27.88833342972739970, 78.11058938209563962, -1.270000000000007345 ) ) ;
#34046 = CARTESIAN_POINT ( 'NONE',  ( -57.29531047346088712, 2.067549486662559222, 1.749273462387482603 ) ) ;
#34047 = CARTESIAN_POINT ( 'NONE',  ( -57.66714133758789274, 1.778435395999748536, 1.675315631185262166 ) ) ;
#34048 = CARTESIAN_POINT ( 'NONE',  ( 1.831848720338790093, -15.17974794010013539, 5.463771816453675712 ) ) ;
#34049 = CARTESIAN_POINT ( 'NONE',  ( -4.123206031880720879, 118.2429491485453354, 0.1807802907187911756 ) ) ;
#34050 = CARTESIAN_POINT ( 'NONE',  ( 1.454130924128286484, 106.2090255614461398, -5.133973488550625852 ) ) ;
#34051 = ORIENTED_EDGE ( 'NONE', *, *, #8932, .F. ) ;
#34052 = CARTESIAN_POINT ( 'NONE',  ( -51.58367816905025194, 14.91232437457545146, 4.609044670965822377 ) ) ;
#34053 = EDGE_CURVE ( 'NONE', #35130, #5873, #19452, .T. ) ;
#34054 = CARTESIAN_POINT ( 'NONE',  ( 8.327809159883996060, 120.1035990385444592, -1.118180374562136148 ) ) ;
#34055 = CARTESIAN_POINT ( 'NONE',  ( -5.590287297675261335, 117.9270669303711117, -0.7481252288361712743 ) ) ;
#34056 = CARTESIAN_POINT ( 'NONE',  ( 4.264584009495184347, 118.2128444281766946, 0.5331355191356830225 ) ) ;
#34057 = CARTESIAN_POINT ( 'NONE',  ( -4.469395743915104191, 155.8822484669112214, -0.8121950557409370886 ) ) ;
#34058 =( NAMED_UNIT ( * ) PLANE_ANGLE_UNIT ( ) SI_UNIT ( $, .RADIAN. ) );
#34059 = VECTOR ( 'NONE', #3907, 1000.000000000000000 ) ;
#34060 = CARTESIAN_POINT ( 'NONE',  ( 0.2172131096560099284, 118.1651004646295888, -0.8870994772933850081 ) ) ;
#34061 = EDGE_CURVE ( 'NONE', #23452, #29626, #9269, .T. ) ;
#34062 = ORIENTED_EDGE ( 'NONE', *, *, #26384, .F. ) ;
#34063 = CARTESIAN_POINT ( 'NONE',  ( 3.874746376330849618, 18.20996518813934628, -2.522041008920607563 ) ) ;
#34064 = CARTESIAN_POINT ( 'NONE',  ( -12.60153737394488438, 128.4643691153342218, -1.495224527512394985 ) ) ;
#34065 = DIRECTION ( 'NONE',  ( -6.353134868986659519E-16, 1.000000000000000000, 0.000000000000000000 ) ) ;
#34066 = CARTESIAN_POINT ( 'NONE',  ( -47.84356795211436264, 19.38525671449518128, 5.197506975154978726 ) ) ;
#34067 = CARTESIAN_POINT ( 'NONE',  ( -6.507153519498132566E-14, 76.29346620154572634, 3.067795752821199360E-29 ) ) ;
#34068 = CARTESIAN_POINT ( 'NONE',  ( -5.946351765289578317, 155.4082313378804088, -0.01440516234414714047 ) ) ;
#34069 = CARTESIAN_POINT ( 'NONE',  ( 4.982727044776202874, 117.5252055169183762, -0.7682891009986807518 ) ) ;
#34070 = CARTESIAN_POINT ( 'NONE',  ( 15.07172804838052471, 121.1899582252741112, 1.138989471373297535 ) ) ;
#34071 = CARTESIAN_POINT ( 'NONE',  ( -3.682264917456323339, 76.29346620154572634, -0.07358041635423923088 ) ) ;
#34073 = CARTESIAN_POINT ( 'NONE',  ( 17.30645727728350280, 153.8449085212272678, -1.293747054194649415 ) ) ;
#34072 = CARTESIAN_POINT ( 'NONE',  ( 2.102813808753936087, -15.18136450426021256, 5.202461169095355942 ) ) ;
#34074 = AXIS2_PLACEMENT_3D ( 'NONE', #2820, #22363, #35388 ) ;
#34075 = CARTESIAN_POINT ( 'NONE',  ( -11.99432760026360434, 123.0912118827050108, 1.285395851362399977 ) ) ;
#34076 = CARTESIAN_POINT ( 'NONE',  ( -0.9748693424575083366, -1.807339741155509660, 0.05984739681150109264 ) ) ;
#34077 = CARTESIAN_POINT ( 'NONE',  ( -15.01050271945743653, 120.7699597703182945, -0.9001124940000717611 ) ) ;
#34078 = CARTESIAN_POINT ( 'NONE',  ( 0.7251766580790658390, 11.37246313919491314, 0.6538263676454795226 ) ) ;
#34079 = ORIENTED_EDGE ( 'NONE', *, *, #18274, .F. ) ;
#34080 = CARTESIAN_POINT ( 'NONE',  ( -48.96835380800505533, 15.76965437727898056, 2.261121166259635107 ) ) ;
#34081 = CARTESIAN_POINT ( 'NONE',  ( -9.519849589794810996, 124.0643708016488063, 0.3285928725474107082 ) ) ;
#34082 = CARTESIAN_POINT ( 'NONE',  ( 2.009495809369673314, -15.14277677434763802, 5.899592854099822148 ) ) ;
#34083 = CARTESIAN_POINT ( 'NONE',  ( 8.931878350220390672, 122.0520977060996586, -0.9029078837920735401 ) ) ;
#34084 = ORIENTED_EDGE ( 'NONE', *, *, #27427, .T. ) ;
#34085 = CARTESIAN_POINT ( 'NONE',  ( 2.528150074622308452, 115.7031097523288139, 1.694672199128987256 ) ) ;
#34086 = CARTESIAN_POINT ( 'NONE',  ( 2.604768916882071128, -14.79682312136586297, 4.847387382002324330 ) ) ;
#34087 = CARTESIAN_POINT ( 'NONE',  ( -4.970811386520536779, 117.4009602783328461, -0.9886943268754924130 ) ) ;
#34088 = CARTESIAN_POINT ( 'NONE',  ( 10.26263990951786198, 126.0184183664171655, 0.1119868329536249096 ) ) ;
#34089 = ORIENTED_EDGE ( 'NONE', *, *, #33091, .T. ) ;
#34090 = CARTESIAN_POINT ( 'NONE',  ( 5.841774105247304227, 118.7305451321402501, 1.158284778981343743 ) ) ;
#34091 = CARTESIAN_POINT ( 'NONE',  ( 5.242938621905797625, 115.7725906505842488, 0.9935740274284472484 ) ) ;
#34092 = DIRECTION ( 'NONE',  ( -0.9816537812491095139, -0.1906721105965040186, -4.769617732184484037E-16 ) ) ;
#34093 = AXIS2_PLACEMENT_3D ( 'NONE', #41715, #1899, #21450 ) ;
#34094 = CARTESIAN_POINT ( 'NONE',  ( 0.02768739821002592222, 156.9833357668885014, -1.385590625008458643 ) ) ;
#34095 = CARTESIAN_POINT ( 'NONE',  ( 0.002459401150238499107, 159.6023738651833810, -0.1230784904792618234 ) ) ;
#34096 = CARTESIAN_POINT ( 'NONE',  ( -10.84307050033138786, 78.30450799593342026, 1.524000000000000687 ) ) ;
#34097 = CIRCLE ( 'NONE', #6884, 2.285999999999999588 ) ;
#34098 = CARTESIAN_POINT ( 'NONE',  ( 1.786952995998799532, -15.53348570852046429, 5.439464539514906605 ) ) ;
#34099 = CARTESIAN_POINT ( 'NONE',  ( 10.45888906141538399, 56.51500000000000057, 4.393716635381806235 ) ) ;
#34100 = CYLINDRICAL_SURFACE ( 'NONE', #13743, 5.588000000000006295 ) ;
#34101 = CARTESIAN_POINT ( 'NONE',  ( -4.726345281775343743, 117.8966967845652505, 0.7850290684345025971 ) ) ;
#34102 = EDGE_LOOP ( 'NONE', ( #1178, #1539, #33773, #32048 ) ) ;
#34103 = CARTESIAN_POINT ( 'NONE',  ( -0.1233619748781853986, 118.7629491485454025, 1.274984637400677245 ) ) ;
#34104 = CARTESIAN_POINT ( 'NONE',  ( -3.290814539092682622, 118.4664756651339701, -0.9164823782932540741 ) ) ;
#34105 = CARTESIAN_POINT ( 'NONE',  ( -4.585195778441760517, 124.9344662015457459, -0.09162312381275013184 ) ) ;
#34106 = CARTESIAN_POINT ( 'NONE',  ( 4.755188516126013454, 117.4716628415562525, 1.195539700728312393 ) ) ;
#34107 = CARTESIAN_POINT ( 'NONE',  ( -12.16475753114696978, 55.74362973025101553, -5.016499999999999737 ) ) ;
#34108 = CARTESIAN_POINT ( 'NONE',  ( -0.04081796246458029020, 114.7739974199301969, 2.042697753608868627 ) ) ;
#34109 = CARTESIAN_POINT ( 'NONE',  ( -3.158589313471108273, 4.191505055319898254, 3.400481138232230194 ) ) ;
#34110 = CARTESIAN_POINT ( 'NONE',  ( -3.630816577625875226E-14, 57.14999999999999147, 0.000000000000000000 ) ) ;
#34111 = FACE_OUTER_BOUND ( 'NONE', #16237, .T. ) ;
#34112 = CARTESIAN_POINT ( 'NONE',  ( 3.930318996895993955, -12.97851325427171254, 2.595110522791146401 ) ) ;
#34113 = CARTESIAN_POINT ( 'NONE',  ( 4.039333660417788074, 117.0582680968029905, -0.9406562914258044250 ) ) ;
#34114 = CARTESIAN_POINT ( 'NONE',  ( 0.9692622191906820062, 39.20946620154573026, 1.289621693195544205 ) ) ;
#34115 = CARTESIAN_POINT ( 'NONE',  ( -1.844538656955264866, 115.7029491485453292, 1.651265962246492913 ) ) ;
#34116 = ORIENTED_EDGE ( 'NONE', *, *, #14373, .F. ) ;
#34117 = CARTESIAN_POINT ( 'NONE',  ( -5.138143029425324748, 105.1220589700577079, -1.444278753282428385 ) ) ;
#34118 = CARTESIAN_POINT ( 'NONE',  ( 4.161657294200716173, -15.28457189793756754, -0.5145498944859950852 ) ) ;
#34119 = CARTESIAN_POINT ( 'NONE',  ( -19.22223103763165497, 149.5120288530235655, 1.725574580128898861 ) ) ;
#34120 = AXIS2_PLACEMENT_3D ( 'NONE', #6460, #3271, #79 ) ;
#34121 = CARTESIAN_POINT ( 'NONE',  ( 0.6140693529284619867, 19.51110927180549481, -0.7576854961706591673 ) ) ;
#34122 = ORIENTED_EDGE ( 'NONE', *, *, #30040, .T. ) ;
#34123 = ORIENTED_EDGE ( 'NONE', *, *, #7190, .T. ) ;
#34124 = CARTESIAN_POINT ( 'NONE',  ( -5.861642722916909243, 64.54502714855203749, -1.523999999999993804 ) ) ;
#34125 = CARTESIAN_POINT ( 'NONE',  ( 4.467639297142982358, 123.9529229959338608, 0.1358511699341446444 ) ) ;
#34126 = CARTESIAN_POINT ( 'NONE',  ( -16.21676096112159371, 148.3349945484709451, 1.109893536416839188 ) ) ;
#34127 = CARTESIAN_POINT ( 'NONE',  ( -4.394136353581303389, 70.68697878297604120, 1.270000000000005347 ) ) ;
#34128 = CARTESIAN_POINT ( 'NONE',  ( 4.523391899494686896, 118.0850475785753559, -0.6138312095713829297 ) ) ;
#34129 = CARTESIAN_POINT ( 'NONE',  ( 11.45258232062217907, 123.1738952066917534, -1.204891439250160401 ) ) ;
#34130 = CIRCLE ( 'NONE', #21837, 0.5080000000000002292 ) ;
#34131 = CARTESIAN_POINT ( 'NONE',  ( -8.818906024077520556, 119.8693228481767932, -1.468947216590822169 ) ) ;
#34132 = CARTESIAN_POINT ( 'NONE',  ( -23.69188486464780752, 78.08202335040543574, 1.269999999999993801 ) ) ;
#34133 = ORIENTED_EDGE ( 'NONE', *, *, #38673, .F. ) ;
#34134 = CARTESIAN_POINT ( 'NONE',  ( 4.253933811591600112, 118.2250371594836906, -0.3060402623648788567 ) ) ;
#34135 = CARTESIAN_POINT ( 'NONE',  ( 4.346810452489679122, 155.8404949922767742, -0.3425513195823393087 ) ) ;
#34136 = ORIENTED_EDGE ( 'NONE', *, *, #1643, .F. ) ;
#34137 = CARTESIAN_POINT ( 'NONE',  ( 3.213008622916347701, -14.43860267280072662, 2.307402664594705222 ) ) ;
#34138 = CIRCLE ( 'NONE', #26641, 0.5080000000000002292 ) ;
#34139 = DIRECTION ( 'NONE',  ( 1.000000000000000000, -1.177520686924251719E-16, 0.000000000000000000 ) ) ;
#34140 = CARTESIAN_POINT ( 'NONE',  ( -55.81791661756895451, 5.217579515125359002, 2.786573170145867806 ) ) ;
#34141 = CARTESIAN_POINT ( 'NONE',  ( -0.4757704999385121702, -3.320450887815510121, -4.596079559024887295 ) ) ;
#34142 = CARTESIAN_POINT ( 'NONE',  ( 11.12341512264660892, 124.6236798342360856, 1.410428355923976751 ) ) ;
#34143 = CARTESIAN_POINT ( 'NONE',  ( 0.08255133343488754716, 33.15144596319247938, 2.721925856402449551 ) ) ;
#34144 = CARTESIAN_POINT ( 'NONE',  ( -5.416028590487236727, 119.2618716387835747, 0.3471801096392534425 ) ) ;
#34145 = AXIS2_PLACEMENT_3D ( 'NONE', #39386, #41955, #41750 ) ;
#34146 = VECTOR ( 'NONE', #24129, 1000.000000000000000 ) ;
#34147 = CARTESIAN_POINT ( 'NONE',  ( 3.746277899330032302, -0.8937244826341392834, -2.755274729908455900 ) ) ;
#34148 = CARTESIAN_POINT ( 'NONE',  ( 14.17736129766400310, 138.8817910697950140, 0.3341079978015795149 ) ) ;
#34149 = FACE_OUTER_BOUND ( 'NONE', #11860, .T. ) ;
#34150 = EDGE_CURVE ( 'NONE', #29590, #34241, #4509, .T. ) ;
#34151 = CARTESIAN_POINT ( 'NONE',  ( -57.97703582661664967, 0.5002880090035632943, -0.5798895178195351274 ) ) ;
#34152 = CARTESIAN_POINT ( 'NONE',  ( -5.529636975226489781, 116.8416598262861896, -0.5092621927480067701 ) ) ;
#34153 = CARTESIAN_POINT ( 'NONE',  ( -6.422645615570758970, 77.88548590848095898, -1.269999999999996465 ) ) ;
#34154 = CARTESIAN_POINT ( 'NONE',  ( -20.21600168833980149, 80.16988503754176065, 1.269999999999995355 ) ) ;
#34155 = CARTESIAN_POINT ( 'NONE',  ( 1.824651611884651636, -15.33505462125984131, 5.392305443003409415 ) ) ;
#34156 = CARTESIAN_POINT ( 'NONE',  ( -8.095114962461808616, 74.19100168833409725, -1.523999999999996691 ) ) ;
#34157 = CARTESIAN_POINT ( 'NONE',  ( -8.364652471777612064, 2.666895906452835252, -0.9765287277423425616 ) ) ;
#34158 = DIRECTION ( 'NONE',  ( -1.000000000000000000, 0.000000000000000000, 0.000000000000000000 ) ) ;
#34159 = CARTESIAN_POINT ( 'NONE',  ( -6.376221727585796537E-14, 51.14746620154573264, 5.777789833161707559E-29 ) ) ;
#34160 = DIRECTION ( 'NONE',  ( -1.000000000000000000, 0.000000000000000000, 0.000000000000000000 ) ) ;
#34161 = EDGE_CURVE ( 'NONE', #15637, #38156, #11966, .T. ) ;
#34162 = CARTESIAN_POINT ( 'NONE',  ( -5.809227842914839179, 77.60418761620948658, 1.270000000000003126 ) ) ;
#34163 = CARTESIAN_POINT ( 'NONE',  ( -1.900581966506003084, 116.7132768022172797, 0.2320997050762017011 ) ) ;
#34164 = EDGE_LOOP ( 'NONE', ( #15451, #13814, #11251, #27924, #1801 ) ) ;
#34165 = CARTESIAN_POINT ( 'NONE',  ( -58.18408008067591197, 1.689533369873860824, -0.1826487275623958351 ) ) ;
#34166 = ORIENTED_EDGE ( 'NONE', *, *, #31332, .T. ) ;
#34167 = CARTESIAN_POINT ( 'NONE',  ( -44.26155013454958720, 21.23036713625713290, -2.970720547513511889 ) ) ;
#34168 = CARTESIAN_POINT ( 'NONE',  ( -0.0006557933561996413981, 120.9974662015457767, 0.03281858119439454852 ) ) ;
#34169 = CARTESIAN_POINT ( 'NONE',  ( 6.347728850385006005, -14.18411723689298753, 0.2678442101147658905 ) ) ;
#34170 = CARTESIAN_POINT ( 'NONE',  ( -4.967439785005512753, 118.2512723699127832, 0.8146033317824223907 ) ) ;
#34171 = CARTESIAN_POINT ( 'NONE',  ( 22.55594873278722545, 149.0203452686010337, -0.8552431815872718612 ) ) ;
#34172 = CARTESIAN_POINT ( 'NONE',  ( -1.471791394198959102, 24.03230288535706549, 4.399545648925609065 ) ) ;
#34173 = CARTESIAN_POINT ( 'NONE',  ( -18.54318072098663706, 125.2038358216989735, -0.7288164436403700153 ) ) ;
#34174 = CARTESIAN_POINT ( 'NONE',  ( -49.53032856719786992, 17.03460727780356265, -5.021522771277230568 ) ) ;
#34175 = ADVANCED_FACE ( 'NONE', ( #42064 ), #34445, .T. ) ;
#34176 = EDGE_LOOP ( 'NONE', ( #2982, #9603, #21099, #29440 ) ) ;
#34177 = DIRECTION ( 'NONE',  ( -5.188838149069471174E-16, 1.699382548006136313E-16, 1.000000000000000000 ) ) ;
#34178 = CARTESIAN_POINT ( 'NONE',  ( 5.706393392231229988, 57.14999999999913882, 5.041882957777255037 ) ) ;
#34179 = CARTESIAN_POINT ( 'NONE',  ( -0.02874415600673332558, 157.0795416643300939, 1.438475106415294302 ) ) ;
#34180 = DIRECTION ( 'NONE',  ( -0.01997839162482761832, -1.040247600000950455E-18, 0.9998004120163610509 ) ) ;
#34181 = CARTESIAN_POINT ( 'NONE',  ( 0.03256023585714045571, 157.9544661776888290, -1.629447346748784220 ) ) ;
#34182 = CARTESIAN_POINT ( 'NONE',  ( -21.52870603658947957, 148.1022500232506616, -2.247031159961963898 ) ) ;
#34183 = CARTESIAN_POINT ( 'NONE',  ( -44.55074271434504851, 21.27721161058206789, -3.389857510897070547 ) ) ;
#34184 = AXIS2_PLACEMENT_3D ( 'NONE', #29005, #6859, #26018 ) ;
#34185 = CARTESIAN_POINT ( 'NONE',  ( 1.514956540612153235, 120.4980338609919386, -0.3173598453907556793 ) ) ;
#34186 = EDGE_CURVE ( 'NONE', #19839, #27753, #20137, .T. ) ;
#34187 = EDGE_LOOP ( 'NONE', ( #17948, #31250, #19709, #28033 ) ) ;
#34188 = CARTESIAN_POINT ( 'NONE',  ( -11.01240597710811997, 122.5598569164413334, -1.651065454484658801 ) ) ;
#34189 = CARTESIAN_POINT ( 'NONE',  ( 4.008975597637738808, -15.55340266690961926, 2.658432704422428738 ) ) ;
#34190 = CARTESIAN_POINT ( 'NONE',  ( -4.357656026889322298, 118.1846519306246250, -0.6081638617269276015 ) ) ;
#34191 = EDGE_CURVE ( 'NONE', #30888, #31300, #29255, .T. ) ;
#34192 = CARTESIAN_POINT ( 'NONE',  ( -57.22363667057550884, 2.289652018204080264, -1.875138655370660379 ) ) ;
#34193 = AXIS2_PLACEMENT_3D ( 'NONE', #995, #4610, #27578 ) ;
#34194 = CARTESIAN_POINT ( 'NONE',  ( -4.880246989775093525, 117.5475785438034961, 0.9414120544623780784 ) ) ;
#34195 = CARTESIAN_POINT ( 'NONE',  ( 9.561780282765681704, 155.2307989660268959, 2.006535919638082532 ) ) ;
#34196 = DIRECTION ( 'NONE',  ( 5.188838149069472160E-16, -1.699382548006136559E-16, -1.000000000000000000 ) ) ;
#34197 = EDGE_CURVE ( 'NONE', #1422, #6797, #15626, .T. ) ;
#34198 = CARTESIAN_POINT ( 'NONE',  ( 13.43647848967384029, 156.9186530619738562, 0.2471310363275584510 ) ) ;
#34199 = CARTESIAN_POINT ( 'NONE',  ( -0.3997009428961929567, 0.5197794802236572753, -8.431077252154732804 ) ) ;
#34200 = CARTESIAN_POINT ( 'NONE',  ( 9.229671467331764134, 123.9961275534082148, 0.5040434471971629860 ) ) ;
#34201 = CARTESIAN_POINT ( 'NONE',  ( 0.01793833495430298061, 118.1627382089642566, -0.8977079103094813828 ) ) ;
#34202 = CARTESIAN_POINT ( 'NONE',  ( -43.02406770836220318, 21.15087974136648086, -0.6363192884524098147 ) ) ;
#34203 = CARTESIAN_POINT ( 'NONE',  ( -2.755218082995318341, 118.1588897907562625, 0.7196486339555533407 ) ) ;
#34204 = CARTESIAN_POINT ( 'NONE',  ( -57.82296528090891030, 0.8544030886276504644, 0.9114307699690248343 ) ) ;
#34205 = CARTESIAN_POINT ( 'NONE',  ( -51.38196307026375820, 20.99359797579823805, -9.826526185745439485E-15 ) ) ;
#34206 = CARTESIAN_POINT ( 'NONE',  ( -8.060084350832312339, 158.6724238832827609, -0.05135189671889796303 ) ) ;
#34207 = EDGE_LOOP ( 'NONE', ( #34412, #16860, #25983, #41611 ) ) ;
#34208 = CARTESIAN_POINT ( 'NONE',  ( -49.93085365557847410, 21.08514737284949803, -1.613137678015130305 ) ) ;
#34209 = CARTESIAN_POINT ( 'NONE',  ( 7.896700704331069076, 122.1485567550560205, -0.5293793203400826153 ) ) ;
#34210 = CARTESIAN_POINT ( 'NONE',  ( -8.321979263998686704, 120.1320355853848554, 1.118248183737064583 ) ) ;
#34211 = VERTEX_POINT ( 'NONE', #16251 ) ;
#34212 = CARTESIAN_POINT ( 'NONE',  ( -4.757346424997288103, 117.3993836135861386, -1.207075064218979810 ) ) ;
#34213 = CARTESIAN_POINT ( 'NONE',  ( -14.70702164887893559, 148.8393470518043955, -0.6194100056173926783 ) ) ;
#34214 = CARTESIAN_POINT ( 'NONE',  ( 4.982342844640083257, -12.32172870019713962, 1.713706004506841740 ) ) ;
#34215 = CARTESIAN_POINT ( 'NONE',  ( -2.946692055775997687, 159.0164033662945258, 1.213088979206726314 ) ) ;
#34216 = CARTESIAN_POINT ( 'NONE',  ( 14.73199999999999754, 17.14499999999999957, 1.804149664503880250E-15 ) ) ;
#34217 = CARTESIAN_POINT ( 'NONE',  ( 16.05840932322194803, 121.2308719818149712, 0.4813400273897942006 ) ) ;
#34218 = CARTESIAN_POINT ( 'NONE',  ( 4.209818400188686027, 155.8650778562950450, 0.1319121167718819154 ) ) ;
#34219 = CARTESIAN_POINT ( 'NONE',  ( 0.6140693529284619867, 19.51110927180549481, -0.7576854961706591673 ) ) ;
#34220 = CARTESIAN_POINT ( 'NONE',  ( -22.53527615164633602, 150.7831677823008363, -0.4503084484864735004 ) ) ;
#34221 = CARTESIAN_POINT ( 'NONE',  ( -20.59944062528794362, 79.83666051618703818, -1.270000000000004015 ) ) ;
#34222 = CONICAL_SURFACE ( 'NONE', #32849, 12.69999999999999751, 0.7853981633974471688 ) ;
#34223 = ORIENTED_EDGE ( 'NONE', *, *, #30555, .F. ) ;
#34224 = CARTESIAN_POINT ( 'NONE',  ( -8.594951744493888768, 74.76616009375631222, 1.270000000000002238 ) ) ;
#34225 = EDGE_LOOP ( 'NONE', ( #7162, #37237, #29862, #16820 ) ) ;
#34226 = CARTESIAN_POINT ( 'NONE',  ( -4.211597740687054170, 118.4194010483798536, 0.8451905551736870192 ) ) ;
#34227 = CARTESIAN_POINT ( 'NONE',  ( -28.09515292912719175, 77.51021392068167870, -1.524000000000007571 ) ) ;
#34228 = CARTESIAN_POINT ( 'NONE',  ( 21.36223069762250049, 149.8571540977637255, 2.130384393597193782 ) ) ;
#34229 = CARTESIAN_POINT ( 'NONE',  ( -57.69387532515962391, 1.166760082113346808, -1.211409762388148792 ) ) ;
#34230 = CARTESIAN_POINT ( 'NONE',  ( 13.10063739191614118, 155.4510764517707742, -1.634185922311342409 ) ) ;
#34231 = CARTESIAN_POINT ( 'NONE',  ( 6.371402057089752269, 24.08812572624405135, -5.527521448792488634 ) ) ;
#34232 = CARTESIAN_POINT ( 'NONE',  ( -22.43644356963083908, 149.3130771379323392, -1.752678757896036332 ) ) ;
#34233 = CARTESIAN_POINT ( 'NONE',  ( 4.978618612593685988, 117.5329194034797382, -0.7802320411340670780 ) ) ;
#34234 = EDGE_LOOP ( 'NONE', ( #24030, #19213, #7437, #20772 ) ) ;
#34235 = CARTESIAN_POINT ( 'NONE',  ( -7.582677863711315247, 122.4179301937671767, -0.01237541680613125222 ) ) ;
#34236 = CARTESIAN_POINT ( 'NONE',  ( 6.238852630440780977, -14.32403127715267743, 0.8647906437036265714 ) ) ;
#34237 = EDGE_CURVE ( 'NONE', #21262, #33817, #9456, .T. ) ;
#34238 = CARTESIAN_POINT ( 'NONE',  ( -17.14500000000000313, 71.11999999999999034, -5.080000000000000959 ) ) ;
#34239 = AXIS2_PLACEMENT_3D ( 'NONE', #9634, #35633, #32428 ) ;
#34240 = CARTESIAN_POINT ( 'NONE',  ( 5.249640227149889427, 56.51499999999963819, 4.563681476173430340 ) ) ;
#34241 = VERTEX_POINT ( 'NONE', #19245 ) ;
#34242 = CARTESIAN_POINT ( 'NONE',  ( 4.177977944338209682, 119.2415290214368042, 0.9917981586689075257 ) ) ;
#34243 = DIRECTION ( 'NONE',  ( 0.000000000000000000, 0.000000000000000000, 1.000000000000000000 ) ) ;
#34244 = EDGE_CURVE ( 'NONE', #8945, #28854, #12700, .T. ) ;
#34245 = FACE_OUTER_BOUND ( 'NONE', #28520, .T. ) ;
#34246 = CIRCLE ( 'NONE', #13837, 0.3810000000000032250 ) ;
#34247 = CARTESIAN_POINT ( 'NONE',  ( -3.292372560053943520, 124.4927030837263118, -0.04348745598417495112 ) ) ;
#34248 = EDGE_CURVE ( 'NONE', #18759, #31609, #12021, .T. ) ;
#34249 = CARTESIAN_POINT ( 'NONE',  ( -1.603550922812138735, -3.093932695209369754, -8.287855504117967342 ) ) ;
#34250 = CARTESIAN_POINT ( 'NONE',  ( 0.5945828676174961247, 120.5739061664170606, 0.2962085107056581790 ) ) ;
#34251 = CARTESIAN_POINT ( 'NONE',  ( -4.787919979293251416, 115.6909491485453003, -1.476228160204360096 ) ) ;
#34252 = CARTESIAN_POINT ( 'NONE',  ( 22.47867321467002810, 150.2745577238280816, -0.5153050491938899746 ) ) ;
#34253 = CARTESIAN_POINT ( 'NONE',  ( 5.706177858098580913, 57.14999999999916724, -5.041924732081959348 ) ) ;
#34254 = EDGE_CURVE ( 'NONE', #30484, #22227, #39068, .T. ) ;
#34255 = CARTESIAN_POINT ( 'NONE',  ( -58.36799900954421361, -0.2878193565351589989, 0.05096520709193082949 ) ) ;
#34256 = CARTESIAN_POINT ( 'NONE',  ( -28.89366501109621410, 63.08038031665430623, -1.524000000000005350 ) ) ;
#34257 = CARTESIAN_POINT ( 'NONE',  ( -52.24107345384238954, 12.50354915519380583, 4.344814160204590436 ) ) ;
#34258 = CARTESIAN_POINT ( 'NONE',  ( 1.930977371672658816, -15.05712096081326123, 5.742647184725755416 ) ) ;
#34259 = CARTESIAN_POINT ( 'NONE',  ( -4.298763888250202392, 118.2143499254979133, 0.3450211622763035280 ) ) ;
#34260 = CARTESIAN_POINT ( 'NONE',  ( 2.560925085873138052, 106.9236017804954599, -4.673771261702133195 ) ) ;
#34261 = ORIENTED_EDGE ( 'NONE', *, *, #36293, .T. ) ;
#34262 = CARTESIAN_POINT ( 'NONE',  ( -51.73272837791831336, 13.19950324185369794, 4.393710239503571202 ) ) ;
#34263 = CARTESIAN_POINT ( 'NONE',  ( -6.212440689485183576, 119.7770897763353446, -1.234393554324211939 ) ) ;
#34264 = CARTESIAN_POINT ( 'NONE',  ( 5.243110457265114377, 104.6144662015457527, 1.505012106405181127 ) ) ;
#34265 = VECTOR ( 'NONE', #24600, 1000.000000000000000 ) ;
#34266 = CARTESIAN_POINT ( 'NONE',  ( 4.381688799442883031, 118.1622743267563607, 0.6667146239118652007 ) ) ;
#34267 = CARTESIAN_POINT ( 'NONE',  ( -5.875838086862464671, 121.3091694753028520, -0.5415667612380997697 ) ) ;
#34268 = CARTESIAN_POINT ( 'NONE',  ( -24.26619908708081041, 81.70586579672512073, 1.269999999999992912 ) ) ;
#34269 = CARTESIAN_POINT ( 'NONE',  ( 13.70496720262315193, 119.6480011847128253, 0.2738578607176476165 ) ) ;
#34270 = VERTEX_POINT ( 'NONE', #6690 ) ;
#34271 = CARTESIAN_POINT ( 'NONE',  ( 2.163044864548389956, 28.58015952483584954, -4.087059112497700042 ) ) ;
#34272 = CARTESIAN_POINT ( 'NONE',  ( 0.007600002268316488618, 120.2037396364829505, -0.3803351912374555721 ) ) ;
#34273 = CARTESIAN_POINT ( 'NONE',  ( -8.095114962461808616, 74.19100168833409725, 1.270000000000002460 ) ) ;
#34274 = CARTESIAN_POINT ( 'NONE',  ( -43.44488126592214883, 21.78892034651229181, 2.392822157539306271 ) ) ;
#34275 = CARTESIAN_POINT ( 'NONE',  ( 5.586884702347364673, 94.32746620154571815, 0.1116392523995368424 ) ) ;
#34276 = CARTESIAN_POINT ( 'NONE',  ( 6.990440677580159523, 121.9275277802277344, 0.3101014599809851502 ) ) ;
#34277 = CARTESIAN_POINT ( 'NONE',  ( -4.488006035213030209, 18.49445617864287073, 1.146732334616328286 ) ) ;
#34278 = CARTESIAN_POINT ( 'NONE',  ( 15.50015290592184591, 121.4967652112180048, 1.085784428920436584 ) ) ;
#34279 = DIRECTION ( 'NONE',  ( 0.000000000000000000, 1.000000000000000000, 0.000000000000000000 ) ) ;
#34281 = CARTESIAN_POINT ( 'NONE',  ( 10.67497907003066260, 119.8050749133877275, -0.9899969268117742027 ) ) ;
#34280 = CARTESIAN_POINT ( 'NONE',  ( 3.162130362391316840, -14.71481139081727640, 3.323541290955854599 ) ) ;
#34282 = CARTESIAN_POINT ( 'NONE',  ( -12.69690185265283056, 124.0847267554996591, 1.337322108705696566 ) ) ;
#34283 = CARTESIAN_POINT ( 'NONE',  ( -2.131885088311801901, 26.04095958170969638, -4.099730575217565232 ) ) ;
#34284 = CARTESIAN_POINT ( 'NONE',  ( -18.41332411163130800, 154.1649927243852858, -1.048538238682171775 ) ) ;
#34285 = AXIS2_PLACEMENT_3D ( 'NONE', #35642, #9235, #2646 ) ;
#34286 = CARTESIAN_POINT ( 'NONE',  ( -0.8578381542044509755, 18.04903173543935679, 0.4659799999690844019 ) ) ;
#34287 = ORIENTED_EDGE ( 'NONE', *, *, #20181, .T. ) ;
#34288 = CARTESIAN_POINT ( 'NONE',  ( -47.93564525088159201, 15.36257551998192916, 0.4079155175245546272 ) ) ;
#34289 = CARTESIAN_POINT ( 'NONE',  ( -9.705341575047336633, 124.1466939447965814, 0.4180229424618550627 ) ) ;
#34290 = CARTESIAN_POINT ( 'NONE',  ( 4.326150682005948767, -14.13415638199089130, 4.511655897031580764 ) ) ;
#34291 = CARTESIAN_POINT ( 'NONE',  ( 5.149255372874153913, 120.5246234221128248, -0.6142761105479899175 ) ) ;
#34292 = VECTOR ( 'NONE', #4292, 1000.000000000000000 ) ;
#34293 = VERTEX_POINT ( 'NONE', #12236 ) ;
#34294 = CARTESIAN_POINT ( 'NONE',  ( 1.791698859000329769, 115.7029403034601103, 1.723151393639055229 ) ) ;
#34295 = CARTESIAN_POINT ( 'NONE',  ( 1.878022632408997250, -15.11918648689831990, 5.509382895440600336 ) ) ;
#34296 = CARTESIAN_POINT ( 'NONE',  ( -4.697896922046175483, 117.7521787132836408, -1.088562244697523385 ) ) ;
#34297 = CARTESIAN_POINT ( 'NONE',  ( 5.301853325284109353, 121.3529869156830046, 0.07809170188345493369 ) ) ;
#34298 = ORIENTED_EDGE ( 'NONE', *, *, #22871, .T. ) ;
#34299 = CARTESIAN_POINT ( 'NONE',  ( 20.36154792711260697, 148.1475078817917961, 2.480623434655590209 ) ) ;
#34300 = CARTESIAN_POINT ( 'NONE',  ( -6.580517660824093636E-14, 85.69146620154573668, -4.881702850681514412E-18 ) ) ;
#34301 = AXIS2_PLACEMENT_3D ( 'NONE', #3238, #16196, #29201 ) ;
#34302 = DIRECTION ( 'NONE',  ( -4.017660918040594346E-17, 1.000000000000000000, 2.376309959284832031E-19 ) ) ;
#34303 = EDGE_CURVE ( 'NONE', #6455, #4992, #25227, .T. ) ;
#34304 = CARTESIAN_POINT ( 'NONE',  ( 0.01443894962456205439, 159.4760848062415732, -0.7225840825867285711 ) ) ;
#34305 = CARTESIAN_POINT ( 'NONE',  ( 13.61761151811281501, 119.6358206793323404, 0.1207630679856301764 ) ) ;
#34306 = FACE_OUTER_BOUND ( 'NONE', #8545, .T. ) ;
#34307 = CIRCLE ( 'NONE', #3028, 3.175000000000001155 ) ;
#34308 = CARTESIAN_POINT ( 'NONE',  ( 1.661411379530861154, -15.34330027928626450, 5.771677961256235001 ) ) ;
#34309 = CARTESIAN_POINT ( 'NONE',  ( 4.962080476404062246, 117.4056796065936368, 1.029808796348710143 ) ) ;
#34310 = CARTESIAN_POINT ( 'NONE',  ( -41.25198653392084935, 23.25239942703034401, -1.524000000000005128 ) ) ;
#34311 = CARTESIAN_POINT ( 'NONE',  ( -4.712400925315380462, 117.8378367728824117, 0.8491269253323575628 ) ) ;
#34312 = EDGE_LOOP ( 'NONE', ( #19859, #40776, #30689, #31472 ) ) ;
#34313 = PLANE ( 'NONE',  #28878 ) ;
#34314 = CARTESIAN_POINT ( 'NONE',  ( -3.010539197181554272, 118.1721198718190635, -0.8802744401777266026 ) ) ;
#34315 = CARTESIAN_POINT ( 'NONE',  ( -3.281580062219434435, 118.9685052735122355, -0.6847577310700789788 ) ) ;
#34316 = CARTESIAN_POINT ( 'NONE',  ( 4.932381249567058035, 117.4753000372011229, 1.061590090608461212 ) ) ;
#34317 = CARTESIAN_POINT ( 'NONE',  ( -4.697896922046175483, 117.7521787132836408, -1.088562244697523385 ) ) ;
#34318 = CARTESIAN_POINT ( 'NONE',  ( -0.09934209769005267199, 106.7790779034713324, 4.971484795507161714 ) ) ;
#34319 = CARTESIAN_POINT ( 'NONE',  ( 4.636249899789679496, -11.37698174978397958, -0.2454043791197063895 ) ) ;
#34320 = CARTESIAN_POINT ( 'NONE',  ( 5.007034960109912447, 117.4001718673160468, -0.7827158424842978190 ) ) ;
#34321 = DIRECTION ( 'NONE',  ( -0.9998004120163608288, 0.000000000000000000, -0.01997839162482747608 ) ) ;
#34322 = CARTESIAN_POINT ( 'NONE',  ( 1.889397806843069905, -15.09730794468430659, 5.542604807410119072 ) ) ;
#34323 = CARTESIAN_POINT ( 'NONE',  ( 6.279970060868345527, 120.0898888515776264, -0.2014705954985338276 ) ) ;
#34324 = CARTESIAN_POINT ( 'NONE',  ( 2.928799644063047936, 38.81416391459460158, 1.351591292951386247 ) ) ;
#34325 = CARTESIAN_POINT ( 'NONE',  ( -0.3836348520032437648, 115.7029491485453008, 1.750602596047696524 ) ) ;
#34326 = CARTESIAN_POINT ( 'NONE',  ( -1.471791394198959324, 24.03230288535706549, 4.399545648925609065 ) ) ;
#34327 = ORIENTED_EDGE ( 'NONE', *, *, #15761, .T. ) ;
#34328 = CARTESIAN_POINT ( 'NONE',  ( -3.608777164148366801, 104.6144662015523465, -3.943486902631163638 ) ) ;
#34329 = TOROIDAL_SURFACE ( 'NONE', #15930, 0.3809999999999995057, 0.2540000000000000036 ) ;
#34330 = CARTESIAN_POINT ( 'NONE',  ( 4.057567908148627112, -15.53776324113162488, 2.457816012360223290 ) ) ;
#34331 = CARTESIAN_POINT ( 'NONE',  ( -12.64706598677953764, 155.2353133052689032, 1.715565181845534637 ) ) ;
#34332 = CARTESIAN_POINT ( 'NONE',  ( 0.5691593726700751033, 20.64373787749807576, 0.7897743370290384313 ) ) ;
#34333 = CARTESIAN_POINT ( 'NONE',  ( -0.2901879621234837447, 21.01165217803846730, -0.9340445150429393939 ) ) ;
#34334 = VERTEX_POINT ( 'NONE', #27113 ) ;
#34335 = EDGE_LOOP ( 'NONE', ( #17327, #38291, #27046, #21655 ) ) ;
#34336 = CARTESIAN_POINT ( 'NONE',  ( 12.69999999999999929, 14.60500000000000043, 0.000000000000000000 ) ) ;
#34337 = CARTESIAN_POINT ( 'NONE',  ( 3.231038154352767311, 124.0549386377059307, 0.1153833196696142788 ) ) ;
#34338 = CARTESIAN_POINT ( 'NONE',  ( -7.181592176188232202, 121.6016026263613838, 0.5649366106928357389 ) ) ;
#34339 = CARTESIAN_POINT ( 'NONE',  ( -6.453647670433203483E-14, 66.13346620154574396, 1.207165459738467839E-19 ) ) ;
#34340 = CARTESIAN_POINT ( 'NONE',  ( 4.728982595459171101, 117.9669356887236376, -0.6198681105378882616 ) ) ;
#34341 = CARTESIAN_POINT ( 'NONE',  ( 15.17272240541826989, 131.2890697635526465, -1.517944203131903036 ) ) ;
#34342 = CARTESIAN_POINT ( 'NONE',  ( -20.08651816730963802, 147.5185649274072830, -2.508444087122727595 ) ) ;
#34343 = CARTESIAN_POINT ( 'NONE',  ( -4.377002418771855474, 72.24507371176854065, -1.269999999999994245 ) ) ;
#34344 = CARTESIAN_POINT ( 'NONE',  ( -1.535725013305945685, 36.30113686556708785, 2.247037283891923476 ) ) ;
#34345 = CARTESIAN_POINT ( 'NONE',  ( 15.93731397951207107, 146.3070982487133165, -0.2768821801232402291 ) ) ;
#34346 = ORIENTED_EDGE ( 'NONE', *, *, #40277, .F. ) ;
#34347 = CARTESIAN_POINT ( 'NONE',  ( 3.141231902390079878, -14.40076222614043644, 1.273921468989656969 ) ) ;
#34348 = CARTESIAN_POINT ( 'NONE',  ( 11.97180806971946332, 56.20439414706017089, -5.016500000000000625 ) ) ;
#34349 = CARTESIAN_POINT ( 'NONE',  ( -56.42349525705669322, 3.945591430476133255, 2.427201670075267881 ) ) ;
#34350 = CARTESIAN_POINT ( 'NONE',  ( -4.434453077421578904, -10.21728329253013179, 1.368390957472948921 ) ) ;
#34351 = CARTESIAN_POINT ( 'NONE',  ( 1.805426509874223262, 156.5029897098349636, 1.055579731365336338 ) ) ;
#34352 = CARTESIAN_POINT ( 'NONE',  ( -3.938977128594349342, 28.07268674286775223, 0.7495841607770360460 ) ) ;
#34353 = CARTESIAN_POINT ( 'NONE',  ( -6.650203214911595495, 123.1390089711370166, -0.06171709628626032701 ) ) ;
#34354 = CARTESIAN_POINT ( 'NONE',  ( 1.719524320724281852, 5.915668354077112667, 4.300554535892874064 ) ) ;
#34355 = CARTESIAN_POINT ( 'NONE',  ( 8.959768907663312021, 123.9105667600146177, 0.2128205007565313611 ) ) ;
#34356 = CARTESIAN_POINT ( 'NONE',  ( 1.876134371277577761, -7.842104223405461205, 8.241158351834352302 ) ) ;
#34357 = CARTESIAN_POINT ( 'NONE',  ( -57.68935019796909813, 1.134378438699040759, -1.023808352551158318 ) ) ;
#34358 = CARTESIAN_POINT ( 'NONE',  ( -8.748764066053464461, 117.8789303818463452, -0.6453613471464660911 ) ) ;
#34359 = DIRECTION ( 'NONE',  ( -0.1951894777626611566, -0.9807655518882887336, 0.000000000000000000 ) ) ;
#34360 = LINE ( 'NONE', #31149, #36648 ) ;
#34361 = CARTESIAN_POINT ( 'NONE',  ( -2.169500164636429140, 35.42160933236649356, 3.123960633263313635 ) ) ;
#34362 = CARTESIAN_POINT ( 'NONE',  ( -8.161197318747062113, 2.438352165997351495, -2.203247879407881804 ) ) ;
#34363 = CARTESIAN_POINT ( 'NONE',  ( 0.08161408160584908422, 118.1588881536456199, 0.9086033322154761782 ) ) ;
#34364 = DIRECTION ( 'NONE',  ( 0.9998004120163609398, 4.016384292689130894E-17, 0.01997839162482749689 ) ) ;
#34365 = CARTESIAN_POINT ( 'NONE',  ( 0.3885115210725473278, 119.2343925067223722, -0.8110907263698885483 ) ) ;
#34366 = CARTESIAN_POINT ( 'NONE',  ( -22.41683308396160967, 150.7562895891929031, 0.1409227600426841420 ) ) ;
#34367 = EDGE_LOOP ( 'NONE', ( #9017, #14395, #25528, #35537 ) ) ;
#34368 = CARTESIAN_POINT ( 'NONE',  ( -58.70413935429054675, 0.2332485698458008905, -0.6626129746612970939 ) ) ;
#34369 = VERTEX_POINT ( 'NONE', #6902 ) ;
#34370 = CARTESIAN_POINT ( 'NONE',  ( -46.78765925927731217, 20.34570826442521962, -4.900687844021752504 ) ) ;
#34371 = CARTESIAN_POINT ( 'NONE',  ( -15.72385166996626715, 146.8976323831864477, -0.3141999770531619940 ) ) ;
#34372 = CARTESIAN_POINT ( 'NONE',  ( 5.095505811086057157, -15.28584205578724386, 3.479711806413861908 ) ) ;
#34373 = CARTESIAN_POINT ( 'NONE',  ( -5.883034912960858343, 118.4234969239897453, 0.8666102449821463383 ) ) ;
#34374 = CARTESIAN_POINT ( 'NONE',  ( 21.51828904745222815, 136.6907720476960435, -0.8331038389761593610 ) ) ;
#34375 = CARTESIAN_POINT ( 'NONE',  ( 1.325333094648095011, 19.28447512809159292, -4.440015753949128730 ) ) ;
#34376 = CARTESIAN_POINT ( 'NONE',  ( -15.91552649980327772, 121.2232988859741027, -0.6415868299260653052 ) ) ;
#34377 = CARTESIAN_POINT ( 'NONE',  ( -52.67526711997813749, 11.72273190574651913, -4.206385566853321656 ) ) ;
#34378 = VERTEX_POINT ( 'NONE', #26484 ) ;
#34379 = CARTESIAN_POINT ( 'NONE',  ( -5.563746608210566436, 116.6985881138792962, -0.07299084064307925779 ) ) ;
#34380 = CARTESIAN_POINT ( 'NONE',  ( -13.85159022459153988, 12.96416000000000146, -5.016499999999999737 ) ) ;
#34381 = CARTESIAN_POINT ( 'NONE',  ( -17.77977776825587597, 147.3864036964934598, 1.530147356706996753 ) ) ;
#34382 = DIRECTION ( 'NONE',  ( -0.3213437296502684171, 0.9469626219732514283, 0.000000000000000000 ) ) ;
#34383 = CARTESIAN_POINT ( 'NONE',  ( 12.16919611748917518, 122.5392882283422864, -1.309229788656694815 ) ) ;
#34384 = CARTESIAN_POINT ( 'NONE',  ( -18.77683424009551771, 152.0234722879370111, -2.226617664588433243 ) ) ;
#34385 = CARTESIAN_POINT ( 'NONE',  ( -54.97180548219925100, 8.422794459035404913, -3.467293221275798309 ) ) ;
#34386 = CARTESIAN_POINT ( 'NONE',  ( 1.530333064024422374, 120.5919059741422217, -0.2783515840389083063 ) ) ;
#34387 = CIRCLE ( 'NONE', #17354, 9.048749999999998295 ) ;
#34388 = ORIENTED_EDGE ( 'NONE', *, *, #41542, .F. ) ;
#34389 = CARTESIAN_POINT ( 'NONE',  ( -7.383155613640980164, 155.9567503867590972, -1.861932028473975986 ) ) ;
#34390 = CARTESIAN_POINT ( 'NONE',  ( 4.538337246427208704, -15.41107556132688394, 0.6303774773485874006 ) ) ;
#34391 = CARTESIAN_POINT ( 'NONE',  ( -4.459763086995446990, 118.1136472263767558, -0.7513301278392107152 ) ) ;
#34392 = EDGE_CURVE ( 'NONE', #12640, #16254, #23264, .T. ) ;
#34393 = CARTESIAN_POINT ( 'NONE',  ( -57.24023649071029496, 3.661034843983918208, -2.195083147259570211 ) ) ;
#34394 = CARTESIAN_POINT ( 'NONE',  ( -4.992877067835030935, 117.4692132720523432, 0.8000675072955271139 ) ) ;
#34395 = CARTESIAN_POINT ( 'NONE',  ( 9.425008295912057577, 155.1592096034013366, 1.957465225861826807 ) ) ;
#34396 = DIRECTION ( 'NONE',  ( -0.8745520943968223548, 0.4849315768086582268, -6.829619984160691573E-16 ) ) ;
#34397 = CARTESIAN_POINT ( 'NONE',  ( -8.412600736458745843, -6.831223903669816799, -0.4304377746521336201 ) ) ;
#34398 = CARTESIAN_POINT ( 'NONE',  ( 13.11017186724473405, 133.9996589410087324, 0.6993036124459158787 ) ) ;
#34399 = DIRECTION ( 'NONE',  ( 0.8138664877804109299, 0.5810519254489895369, 0.000000000000000000 ) ) ;
#34401 = ORIENTED_EDGE ( 'NONE', *, *, #11859, .T. ) ;
#34400 = CARTESIAN_POINT ( 'NONE',  ( -44.22601141000046709, 20.28211486706537414, -1.272444536529930836 ) ) ;
#34402 = CARTESIAN_POINT ( 'NONE',  ( -1.585929963085191741, 118.1588900223178058, 0.8129015274758119025 ) ) ;
#34403 = CARTESIAN_POINT ( 'NONE',  ( 1.967271012213831938, 118.7629491485454025, 1.232500030677896374 ) ) ;
#34404 = CARTESIAN_POINT ( 'NONE',  ( -58.22824150656796860, 0.01698906185855497686, 0.5964212723216197887 ) ) ;
#34405 = CARTESIAN_POINT ( 'NONE',  ( -51.75204694603132083, 19.49597778360960021, 0.7628839638999955763 ) ) ;
#34406 = CARTESIAN_POINT ( 'NONE',  ( -23.41759249777153684, 146.8136392739129974, -0.2357739188755807458 ) ) ;
#34407 = AXIS2_PLACEMENT_3D ( 'NONE', #30176, #39786, #599 ) ;
#34408 = ORIENTED_EDGE ( 'NONE', *, *, #29800, .F. ) ;
#34409 = CARTESIAN_POINT ( 'NONE',  ( -47.91489772873670461, 20.73163290703075745, -4.601312741205012991 ) ) ;
#34410 = CARTESIAN_POINT ( 'NONE',  ( 6.912737236431420129, 121.7988612569186984, -0.2654354181093423470 ) ) ;
#34411 = CARTESIAN_POINT ( 'NONE',  ( -8.036149603168206923, 121.5005262100067256, 0.8572904197357047451 ) ) ;
#34412 = ORIENTED_EDGE ( 'NONE', *, *, #17757, .T. ) ;
#34413 = CARTESIAN_POINT ( 'NONE',  ( -47.84623148323176878, 19.38793950428539503, 5.205198760075354869 ) ) ;
#34414 = CARTESIAN_POINT ( 'NONE',  ( -15.80537369954035753, 146.5893318786020814, -0.6464893008334197111 ) ) ;
#34415 = CARTESIAN_POINT ( 'NONE',  ( 4.916912942907655903, -13.49232782388964935, 3.465564004687308408 ) ) ;
#34416 = CARTESIAN_POINT ( 'NONE',  ( -20.76678851138498416, 151.0745573368290593, 1.154740394482948407 ) ) ;
#34417 = B_SPLINE_CURVE_WITH_KNOTS ( 'NONE', 3,
 ( #36484, #30081, #7305, #39895, #26886, #10487, #23457, #33291, #30285, #1127 ),
 .UNSPECIFIED., .F., .F.,
 ( 4, 2, 2, 2, 4 ),
 ( 0.000000000000000000, 0.001159180624616241214, 0.002318361249232482428, 0.003477541873848724509, 0.004636722498464966591 ),
 .UNSPECIFIED. ) ;
#34418 = CARTESIAN_POINT ( 'NONE',  ( 14.39766717389552042, 60.02151067229126369, -1.904999999999999583 ) ) ;
#34419 = CARTESIAN_POINT ( 'NONE',  ( 22.64824804725698826, 137.2763855621842026, 0.6699328029008020380 ) ) ;
#34420 = CARTESIAN_POINT ( 'NONE',  ( -0.0006556493172109406848, 120.9974662015457767, 0.03281137289327806100 ) ) ;
#34421 = DIRECTION ( 'NONE',  ( 1.000000000000000000, 0.000000000000000000, -5.975917486140574681E-16 ) ) ;
#34422 = CARTESIAN_POINT ( 'NONE',  ( -0.7472855871240335901, 21.88424109716052612, -0.6269268744489370215 ) ) ;
#34423 = EDGE_CURVE ( 'NONE', #14494, #18759, #4557, .T. ) ;
#34424 = CARTESIAN_POINT ( 'NONE',  ( -1.804784692667670054, 116.4728921782852922, -0.07541441754812425180 ) ) ;
#34425 = CARTESIAN_POINT ( 'NONE',  ( -41.06677624538381366, 23.07857903911209974, -1.524000000001595856 ) ) ;
#34426 = DIRECTION ( 'NONE',  ( 0.5149185422762101449, -0.8572391118119511155, 4.128606161907551211E-16 ) ) ;
#34427 = VERTEX_POINT ( 'NONE', #16678 ) ;
#34428 = CARTESIAN_POINT ( 'NONE',  ( 3.896950258392768873, 118.1803102188741121, 0.9604330818198881792 ) ) ;
#34429 = DIRECTION ( 'NONE',  ( -0.8745520943968235761, 0.4849315768086558398, -4.268512490100410909E-16 ) ) ;
#34430 = CARTESIAN_POINT ( 'NONE',  ( 12.43751437118950953, 120.3283006479967128, 1.391730434942824779 ) ) ;
#34431 = CARTESIAN_POINT ( 'NONE',  ( -54.51629495444830553, 7.799846118215131519, -3.232377281229704025 ) ) ;
#34432 = CARTESIAN_POINT ( 'NONE',  ( 19.84954981513660499, 141.2215177107240436, -1.686013488323441001 ) ) ;
#34433 = CARTESIAN_POINT ( 'NONE',  ( 4.135298993362768627, -14.76517611359900961, -2.065434832541708676 ) ) ;
#34434 = CARTESIAN_POINT ( 'NONE',  ( -13.81631647976139909, 120.6843904051541898, -1.269697867868519792 ) ) ;
#34435 = CARTESIAN_POINT ( 'NONE',  ( 4.784420482501478666, 117.7320086554665721, -0.8971979045722391355 ) ) ;
#34436 = CARTESIAN_POINT ( 'NONE',  ( 1.980401745280924830, 106.6864334246082961, 4.967395836420048560 ) ) ;
#34437 = ORIENTED_EDGE ( 'NONE', *, *, #38483, .T. ) ;
#34438 = B_SPLINE_CURVE_WITH_KNOTS ( 'NONE', 3,
 ( #27213, #1252, #16985, #24003 ),
 .UNSPECIFIED., .F., .F.,
 ( 4, 4 ),
 ( 0.000000000000000000, 1.000000000000000000 ),
 .UNSPECIFIED. ) ;
#34439 = CARTESIAN_POINT ( 'NONE',  ( -11.90298433346896090, 130.3805625696445816, -0.1299774887382022792 ) ) ;
#34440 = CARTESIAN_POINT ( 'NONE',  ( -19.37512658372783747, 148.3988719805327037, -2.511650730565585299 ) ) ;
#34441 = CARTESIAN_POINT ( 'NONE',  ( 6.104261451579751530, -14.47397795074312299, 1.449478640324443290 ) ) ;
#34442 = FACE_OUTER_BOUND ( 'NONE', #23240, .T. ) ;
#34443 = AXIS2_PLACEMENT_3D ( 'NONE', #24036, #18055, #8275 ) ;
#34444 = CARTESIAN_POINT ( 'NONE',  ( -1.086168526012032842, 117.3993836040899623, -1.476592527281789691 ) ) ;
#34446 = ORIENTED_EDGE ( 'NONE', *, *, #32350, .T. ) ;
#34445 = TOROIDAL_SURFACE ( 'NONE', #38521, 6.905624999999998792, 0.5556250000000014788 ) ;
#34447 = CARTESIAN_POINT ( 'NONE',  ( 18.98749958112889757, 148.5750135429820205, 2.495758040776019371 ) ) ;
#34448 = TOROIDAL_SURFACE ( 'NONE', #1137, 5.080000000000005400, 0.5080000000000000071 ) ;
#34449 = DIRECTION ( 'NONE',  ( 1.000000000000000000, -1.288607544181256449E-16, 0.000000000000000000 ) ) ;
#34450 = CARTESIAN_POINT ( 'NONE',  ( -4.842657161150313527, 118.7629491485453599, -0.3779612899170270435 ) ) ;
#34451 = CARTESIAN_POINT ( 'NONE',  ( -0.5876368209473940007, 111.1955024190080223, 3.248215591009249170 ) ) ;
#34452 = CARTESIAN_POINT ( 'NONE',  ( 5.926391002875100789, -6.993723907645660098, 5.986726992520772228 ) ) ;
#34453 = CARTESIAN_POINT ( 'NONE',  ( 10.86813797462336950, 153.1125297277760069, 1.236783938685797501 ) ) ;
#34454 = CARTESIAN_POINT ( 'NONE',  ( -4.911716961673469939, 115.6909491485453003, -1.456282297173534301 ) ) ;
#34455 = EDGE_CURVE ( 'NONE', #588, #41686, #36501, .T. ) ;
#34456 = CARTESIAN_POINT ( 'NONE',  ( 5.603706277412528358, 159.0849926622337023, -0.4754325247485730599 ) ) ;
#34457 = DIRECTION ( 'NONE',  ( 1.000000000000000000, -9.627370216492862708E-17, 0.000000000000000000 ) ) ;
#34458 = CARTESIAN_POINT ( 'NONE',  ( -57.96289673749877380, 0.5850535986806209010, 0.9075947480399308986 ) ) ;
#34459 = FILL_AREA_STYLE_COLOUR ( '', #36437 ) ;
#34460 = CARTESIAN_POINT ( 'NONE',  ( 22.46755768833288158, 150.8526571111528654, 0.4489552724284878171 ) ) ;
#34461 = CARTESIAN_POINT ( 'NONE',  ( -4.267945882554810666, 118.2240384700266418, 0.2902935525537765904 ) ) ;
#34462 = CARTESIAN_POINT ( 'NONE',  ( -17.31377588638430964, 122.7721875394316555, -0.3459704467065359834 ) ) ;
#34463 = ORIENTED_EDGE ( 'NONE', *, *, #36513, .T. ) ;
#34464 = EDGE_CURVE ( 'NONE', #30173, #30054, #31729, .T. ) ;
#34465 = CARTESIAN_POINT ( 'NONE',  ( -49.59816314059867182, 17.91649583374774224, 5.069000701391649599 ) ) ;
#34466 = CARTESIAN_POINT ( 'NONE',  ( 8.297356343339515661, 120.2518627151980013, -1.115698539510747489 ) ) ;
#34467 = FACE_OUTER_BOUND ( 'NONE', #9117, .T. ) ;
#34468 = CARTESIAN_POINT ( 'NONE',  ( 4.254265354952431188, 118.2238472574425998, 0.4591671670676380490 ) ) ;
#34469 = CARTESIAN_POINT ( 'NONE',  ( -9.255566420661768490, 123.6186430441458981, -0.7743267827205286835 ) ) ;
#34470 = DIRECTION ( 'NONE',  ( 0.9336303900108928744, 0.3582377630123714241, 0.000000000000000000 ) ) ;
#34471 = CARTESIAN_POINT ( 'NONE',  ( 1.794468298957800689, 116.4672891243423578, 0.03585774721038179763 ) ) ;
#34472 = ORIENTED_EDGE ( 'NONE', *, *, #15989, .T. ) ;
#34473 = CARTESIAN_POINT ( 'NONE',  ( -4.460028654926622593, 22.53297844546955631, 1.214995109042491528 ) ) ;
#34474 = CARTESIAN_POINT ( 'NONE',  ( -30.59449053071180558, 55.40488188707849559, 1.523999999999994692 ) ) ;
#34475 = FACE_OUTER_BOUND ( 'NONE', #7817, .T. ) ;
#34476 = CARTESIAN_POINT ( 'NONE',  ( 5.424023212060550492, 78.92586886208859198, -5.134886908577998454 ) ) ;
#34477 = CIRCLE ( 'NONE', #23571, 0.6350000000000006750 ) ;
#34478 = CARTESIAN_POINT ( 'NONE',  ( -6.995060180358994906, 121.8891585157791866, 0.1212626282798120736 ) ) ;
#34479 = EDGE_CURVE ( 'NONE', #30442, #7672, #4546, .T. ) ;
#34480 = CARTESIAN_POINT ( 'NONE',  ( -2.714482067202859561, 26.26591195808746448, -3.750338772627290762 ) ) ;
#34481 = CARTESIAN_POINT ( 'NONE',  ( 14.73023064483735922, 156.1040168620350244, 1.249499669456201723 ) ) ;
#34482 = CARTESIAN_POINT ( 'NONE',  ( -0.7257356453791840023, 104.6144662015456390, -4.780984660456490509 ) ) ;
#34484 = CARTESIAN_POINT ( 'NONE',  ( 7.037849409249268717, 158.0922581832940921, -1.451942896407524275 ) ) ;
#34483 = CARTESIAN_POINT ( 'NONE',  ( 3.092086460852839114, -14.79905751219236265, 3.633802299706017980 ) ) ;
#34485 = CARTESIAN_POINT ( 'NONE',  ( -0.9532528233480704882, 157.3234082283764792, 1.521469375400507529 ) ) ;
#34486 = CARTESIAN_POINT ( 'NONE',  ( 4.626035402534343532, 22.79242798913371360, 0.3558936578225105341 ) ) ;
#34487 = CARTESIAN_POINT ( 'NONE',  ( -23.03149411880800912, 148.7220611141358404, -1.316198435982438575 ) ) ;
#34488 = EDGE_CURVE ( 'NONE', #22232, #4990, #8352, .T. ) ;
#34489 = CARTESIAN_POINT ( 'NONE',  ( 0.7093541224826089842, 23.24201423063343697, -0.6674325600367136957 ) ) ;
#34490 = ORIENTED_EDGE ( 'NONE', *, *, #25321, .F. ) ;
#34491 = CARTESIAN_POINT ( 'NONE',  ( -54.85284047870325708, 7.073525668766899699, 2.945785012852135676 ) ) ;
#34492 = CARTESIAN_POINT ( 'NONE',  ( -10.70072142757971889, 153.0728289088170300, 0.5595718250706017693 ) ) ;
#34493 = CARTESIAN_POINT ( 'NONE',  ( 5.386302285778954868, -11.84411807400357475, 0.7125209553660817319 ) ) ;
#34494 = CARTESIAN_POINT ( 'NONE',  ( 12.26974321764554965, 126.0625018263836807, -1.123002009909297438 ) ) ;
#34495 = ORIENTED_EDGE ( 'NONE', *, *, #20228, .T. ) ;
#34496 = VECTOR ( 'NONE', #31550, 1000.000000000000000 ) ;
#34497 = CARTESIAN_POINT ( 'NONE',  ( 0.7571409010366814130, 115.7028914826202595, 1.755555203384807861 ) ) ;
#34498 = ORIENTED_EDGE ( 'NONE', *, *, #17066, .F. ) ;
#34499 = CARTESIAN_POINT ( 'NONE',  ( 2.253193219399967973, -14.99063959920543532, 5.175666457621841410 ) ) ;
#34500 = CARTESIAN_POINT ( 'NONE',  ( -4.656554223671448334, 117.8898311454812244, -0.9968106679264355785 ) ) ;
#34501 = CARTESIAN_POINT ( 'NONE',  ( 12.88210196283048248, 133.7932622986943159, 0.2101989309002757766 ) ) ;
#34502 = EDGE_CURVE ( 'NONE', #19961, #14753, #40591, .T. ) ;
#34503 = ORIENTED_EDGE ( 'NONE', *, *, #18066, .T. ) ;
#34504 = CARTESIAN_POINT ( 'NONE',  ( 11.40914533023166832, 121.1873859956591843, 1.678693868224012009 ) ) ;
#34505 = DIRECTION ( 'NONE',  ( -0.9998004120163609398, -4.016384292689130894E-17, -0.01997839162482749689 ) ) ;
#34506 = AXIS2_PLACEMENT_3D ( 'NONE', #32299, #3129, #35088 ) ;
#34507 = CARTESIAN_POINT ( 'NONE',  ( 5.938381009910428610, 56.51499999999999346, 4.381499999999999062 ) ) ;
#34508 = CARTESIAN_POINT ( 'NONE',  ( 0.02874415600660452930, 157.0795416643300939, -1.438475106415293858 ) ) ;
#34509 = AXIS2_PLACEMENT_3D ( 'NONE', #28850, #6280, #22846 ) ;
#34510 = CARTESIAN_POINT ( 'NONE',  ( 9.765169485063754706, 118.0373187826741486, -0.07890504670268475018 ) ) ;
#34511 = DIRECTION ( 'NONE',  ( 9.627370216492862708E-17, 1.000000000000000000, -0.000000000000000000 ) ) ;
#34512 = CARTESIAN_POINT ( 'NONE',  ( 1.680419162510425002, -15.45927319065069838, 5.515672785773912068 ) ) ;
#34513 = DIRECTION ( 'NONE',  ( -0.8745520943968243532, 0.4849315768086547296, -6.829619984160642269E-16 ) ) ;
#34514 = CARTESIAN_POINT ( 'NONE',  ( -6.059261036834476144, 57.14999999999999858, -5.016499999999999737 ) ) ;
#34515 = ADVANCED_FACE ( 'NONE', ( #39916 ), #23690, .F. ) ;
#34516 = CARTESIAN_POINT ( 'NONE',  ( -4.617919775738188015, 117.9735533346422187, 0.7423233486650107071 ) ) ;
#34517 = ADVANCED_FACE ( 'NONE', ( #39276 ), #30101, .T. ) ;
#34518 = ORIENTED_EDGE ( 'NONE', *, *, #26363, .F. ) ;
#34519 = ORIENTED_EDGE ( 'NONE', *, *, #11795, .F. ) ;
#34520 = DIRECTION ( 'NONE',  ( -5.188838149069471174E-16, 1.699382548006136313E-16, 1.000000000000000000 ) ) ;
#34521 = CARTESIAN_POINT ( 'NONE',  ( -2.668721918458945019, 117.7585162296088583, -0.8088457382527453055 ) ) ;
#34522 = CARTESIAN_POINT ( 'NONE',  ( -6.983090746392761616, 124.7321584522365896, -0.1405484879196982895 ) ) ;
#34523 = CARTESIAN_POINT ( 'NONE',  ( 4.741947938571901666, 117.6342773529492547, 1.141888482007099137 ) ) ;
#34524 = CARTESIAN_POINT ( 'NONE',  ( -11.66725022230187037, 55.42194143536166706, -5.016499999999783910 ) ) ;
#34525 = CARTESIAN_POINT ( 'NONE',  ( -1.012635771704909038, 123.9312678891798640, 0.06995516121779321583 ) ) ;
#34526 = AXIS2_PLACEMENT_3D ( 'NONE', #32488, #22660, #41457 ) ;
#34527 = CARTESIAN_POINT ( 'NONE',  ( -3.832284926465886254, -5.753926550059754064, 2.584458424559757272 ) ) ;
#34528 = CARTESIAN_POINT ( 'NONE',  ( 4.866147868668515564, 117.4089627612368076, -0.9906677743061890196 ) ) ;
#34529 = LINE ( 'NONE', #5355, #887 ) ;
#34530 = CARTESIAN_POINT ( 'NONE',  ( 2.131140412894510838, -15.01828590152304344, 5.319755587316977952 ) ) ;
#34531 = CARTESIAN_POINT ( 'NONE',  ( 5.235361408262197536, 116.2637919873444190, -0.9632728985350239581 ) ) ;
#34532 = CARTESIAN_POINT ( 'NONE',  ( 7.787533423162888546, 122.6196153997145473, 0.09973116958504993357 ) ) ;
#34533 = CARTESIAN_POINT ( 'NONE',  ( -6.346781410994640993, 30.04503731349425166, 1.591420273447384348 ) ) ;
#34534 = CARTESIAN_POINT ( 'NONE',  ( -0.6270198638313982942, 115.7029626491897716, 1.737414609200174542 ) ) ;
#34535 = CARTESIAN_POINT ( 'NONE',  ( 4.256838582791900194, 16.71066835407712858, 1.825063967593055558 ) ) ;
#34537 = ORIENTED_EDGE ( 'NONE', *, *, #25378, .F. ) ;
#34536 = CARTESIAN_POINT ( 'NONE',  ( 22.84108495963309693, 150.1122123445777277, 1.048654020290956446 ) ) ;
#34538 = CARTESIAN_POINT ( 'NONE',  ( 0.2171711340010081537, 104.6144662015456674, -4.831476934653068156 ) ) ;
#34539 = CARTESIAN_POINT ( 'NONE',  ( 2.152540537132713538, -15.51301927577993034, 5.194954439406326507 ) ) ;
#34540 = CARTESIAN_POINT ( 'NONE',  ( -15.79478014299093580, 153.2725199748809928, 1.714666983805330780 ) ) ;
#34541 = CARTESIAN_POINT ( 'NONE',  ( -0.7801697309092696653, 18.27050645547500451, 0.5824522774875325881 ) ) ;
#34542 = EDGE_CURVE ( 'NONE', #40365, #29748, #33100, .T. ) ;
#34543 = CARTESIAN_POINT ( 'NONE',  ( 0.9475510003767251277, 17.78785052102138664, 0.2306771022979090535 ) ) ;
#34544 = ORIENTED_EDGE ( 'NONE', *, *, #30250, .F. ) ;
#34545 = ORIENTED_EDGE ( 'NONE', *, *, #30069, .F. ) ;
#34546 = DIRECTION ( 'NONE',  ( -6.829619984160660610E-15, 0.000000000000000000, -1.000000000000000000 ) ) ;
#34547 = CIRCLE ( 'NONE', #20894, 0.2540000000000012248 ) ;
#34548 = CARTESIAN_POINT ( 'NONE',  ( 2.044121638888182435, 114.8832439220486350, 1.972317757894941570 ) ) ;
#34549 = CARTESIAN_POINT ( 'NONE',  ( -1.473868052710668675, 120.2326517397585377, 0.4086940711265545922 ) ) ;
#34550 = CARTESIAN_POINT ( 'NONE',  ( -42.24009424636936672, 22.39526031405182849, 1.717801471214081444 ) ) ;
#34551 = CARTESIAN_POINT ( 'NONE',  ( 3.494528270914563528, -13.06595970051097133, 2.012497701936279082 ) ) ;
#34552 = CARTESIAN_POINT ( 'NONE',  ( 10.29797255167324010, 122.2012759285571946, -1.140151759267314047 ) ) ;
#34553 = CARTESIAN_POINT ( 'NONE',  ( -13.17434061382168231, 122.5785676075921060, -1.825321299320728397 ) ) ;
#34554 = CARTESIAN_POINT ( 'NONE',  ( -14.53564353655538000, 79.78436006922240153, -1.270000000000000906 ) ) ;
#34555 = CARTESIAN_POINT ( 'NONE',  ( -19.15923810799328209, 79.68098548105338352, -1.270000000000003348 ) ) ;
#34556 = CARTESIAN_POINT ( 'NONE',  ( 4.520495148372919658, 121.0527503406816123, -0.1761357111252131458 ) ) ;
#34557 = ORIENTED_EDGE ( 'NONE', *, *, #6569, .F. ) ;
#34558 = CARTESIAN_POINT ( 'NONE',  ( 2.993548201347409510, -14.88003303992029025, 3.932447912750371977 ) ) ;
#34559 = CARTESIAN_POINT ( 'NONE',  ( 0.03201377673046579275, 33.52827609515317420, 3.383309648808628278 ) ) ;
#34560 = AXIS2_PLACEMENT_3D ( 'NONE', #36798, #20161, #10380 ) ;
#34561 = CARTESIAN_POINT ( 'NONE',  ( -58.63691926681516975, -0.7730888055359085298, 0.03927874230119918209 ) ) ;
#34562 = CARTESIAN_POINT ( 'NONE',  ( -4.070821798575407158, -9.904843093959119216, 2.245307785351264407 ) ) ;
#34563 = CARTESIAN_POINT ( 'NONE',  ( 9.825947633753759902, 123.3250567171901082, 1.189973159844531114 ) ) ;
#34564 = CARTESIAN_POINT ( 'NONE',  ( -3.032836294544972056, 29.78154503720477919, 3.248403939658073281 ) ) ;
#34565 = CARTESIAN_POINT ( 'NONE',  ( -5.480007210012731278, 117.5214873295501405, 0.6081561229113362499 ) ) ;
#34566 = CARTESIAN_POINT ( 'NONE',  ( 0.6989348986720191892, -4.029744825116962303, 4.573446973323917142 ) ) ;
#34567 = CARTESIAN_POINT ( 'NONE',  ( 9.538359384048550993, 124.8019839352694476, 0.1905991205270211042 ) ) ;
#34568 = CARTESIAN_POINT ( 'NONE',  ( 7.363685156731384573, -6.572911479292511849, 4.144591825403105112 ) ) ;
#34569 = CARTESIAN_POINT ( 'NONE',  ( -56.90438685736649660, 2.765855619508456265, -1.561774844827678033 ) ) ;
#34570 = CARTESIAN_POINT ( 'NONE',  ( 2.157000451504500482, 116.4221920678469928, -0.2562403356321266146 ) ) ;
#34571 = CARTESIAN_POINT ( 'NONE',  ( 0.09221630143964076876, 107.6766875080336376, -4.614880812453268533 ) ) ;
#34572 = CARTESIAN_POINT ( 'NONE',  ( -17.09698261757901960, 84.43312239790384410, -1.524000000000002908 ) ) ;
#34573 = FACE_OUTER_BOUND ( 'NONE', #8423, .T. ) ;
#34574 = CARTESIAN_POINT ( 'NONE',  ( -6.690270197923770645, -5.753818539685515709, 5.116497609988504891 ) ) ;
#34575 = CARTESIAN_POINT ( 'NONE',  ( 1.551977928113887462, 118.1588881584012825, 0.8756194964229589983 ) ) ;
#34576 = DIRECTION ( 'NONE',  ( -0.9998501190848635423, -0.01731298258487451447, -5.158639060800523934E-16 ) ) ;
#34577 = CARTESIAN_POINT ( 'NONE',  ( -6.564189886853176475E-14, 81.62746620154572952, -5.847435218134868453E-18 ) ) ;
#34578 = CARTESIAN_POINT ( 'NONE',  ( 0.9632506926927688617, 123.2612876230388395, -0.1349244037310162458 ) ) ;
#34579 = CARTESIAN_POINT ( 'NONE',  ( -22.86474403352236706, 150.1122123445777277, 0.1353427831800517178 ) ) ;
#34580 = ORIENTED_EDGE ( 'NONE', *, *, #5011, .T. ) ;
#34581 = CARTESIAN_POINT ( 'NONE',  ( -58.76922381231047865, 0.08391971067571446508, -0.07695160083613393487 ) ) ;
#34582 = ORIENTED_EDGE ( 'NONE', *, *, #36900, .F. ) ;
#34583 = CARTESIAN_POINT ( 'NONE',  ( -3.770027696949578289, 121.0935558011302930, -0.04039886233734658882 ) ) ;
#34584 = CARTESIAN_POINT ( 'NONE',  ( 5.672040739448011237, -14.80640238898532601, 2.735881018706089129 ) ) ;
#34585 = CARTESIAN_POINT ( 'NONE',  ( -18.67489051167937930, 151.9584835496716266, 1.528205706551668541 ) ) ;
#34586 = CARTESIAN_POINT ( 'NONE',  ( 22.59612908711461188, 148.7221180073953235, -0.8559155618276410582 ) ) ;
#34587 = CARTESIAN_POINT ( 'NONE',  ( -3.453265078539333288, 21.00871511114837276, -3.102408547967784092 ) ) ;
#34588 = CARTESIAN_POINT ( 'NONE',  ( -22.45364888651512913, 150.7739627601066275, -0.8979154079963819202 ) ) ;
#34589 = CARTESIAN_POINT ( 'NONE',  ( -52.06727285681002115, 12.81026601648138019, -4.396686699310198954 ) ) ;
#34590 = ORIENTED_EDGE ( 'NONE', *, *, #22473, .T. ) ;
#34591 = CARTESIAN_POINT ( 'NONE',  ( -5.563323361884090268, 116.7152635471598359, 0.01911022379953509695 ) ) ;
#34592 = DIRECTION ( 'NONE',  ( 0.8745520943968246863, -0.4849315768086538414, 5.122214988120500191E-16 ) ) ;
#34593 = CARTESIAN_POINT ( 'NONE',  ( -16.76421760064445365, 140.0893442862094673, 1.556517483701108207 ) ) ;
#34594 = CARTESIAN_POINT ( 'NONE',  ( -57.04684799334965106, 2.555418974455772041, -1.775728233086056873 ) ) ;
#34595 = CARTESIAN_POINT ( 'NONE',  ( 5.043395383124224196, 119.2220797256985350, -0.8992592568097312888 ) ) ;
#34596 = CARTESIAN_POINT ( 'NONE',  ( -14.14688762606146177, 122.0820592118662091, -1.654226634644705651 ) ) ;
#34597 = CARTESIAN_POINT ( 'NONE',  ( -50.82551848962686591, 16.13924203555649228, -4.804203053272171786 ) ) ;
#34598 = CARTESIAN_POINT ( 'NONE',  ( 0.6059414056332816934, 120.5739061664170606, -0.2722191786371236377 ) ) ;
#34599 = ORIENTED_EDGE ( 'NONE', *, *, #586, .T. ) ;
#34600 = CARTESIAN_POINT ( 'NONE',  ( -11.24613893767488548, 123.2561760277034324, -1.620791190024704953 ) ) ;
#34601 = CARTESIAN_POINT ( 'NONE',  ( 3.662106647173574370, -15.69883703644059381, 4.006612474821164227 ) ) ;
#34602 = AXIS2_PLACEMENT_3D ( 'NONE', #29210, #25598, #53 ) ;
#34603 = CARTESIAN_POINT ( 'NONE',  ( -4.154103066237196273, 118.2394448457162497, -0.3903888767277005067 ) ) ;
#34604 = CARTESIAN_POINT ( 'NONE',  ( -58.24002838079472610, 0.001074765447070524793, -0.6562585879479864159 ) ) ;
#34605 = DIRECTION ( 'NONE',  ( -0.000000000000000000, -0.000000000000000000, -1.000000000000000000 ) ) ;
#34606 = CARTESIAN_POINT ( 'NONE',  ( 4.277613954752398584, 119.9149831030956932, 0.8793409099722719890 ) ) ;
#34607 = DIRECTION ( 'NONE',  ( -0.6594218222380264782, -0.7517731442105928252, -1.663245240604415392E-15 ) ) ;
#34608 = PRODUCT_DEFINITION_FORMATION_WITH_SPECIFIED_SOURCE ( 'ANY', '', #35769, .NOT_KNOWN. ) ;
#34609 = CARTESIAN_POINT ( 'NONE',  ( -2.337594367139880003, 4.813278044257511823, 8.129740476481943645 ) ) ;
#34610 = CARTESIAN_POINT ( 'NONE',  ( 1.586003330670501699, 156.2604006213118453, 0.2328413704193784128 ) ) ;
#34611 = CARTESIAN_POINT ( 'NONE',  ( -58.20820809768403592, 1.420579653404085985, -1.355822160094614759 ) ) ;
#34612 = AXIS2_PLACEMENT_3D ( 'NONE', #41008, #23590, #16790 ) ;
#34614 = EDGE_LOOP ( 'NONE', ( #22645, #25055, #34827, #37861 ) ) ;
#34613 = DIRECTION ( 'NONE',  ( 0.000000000000000000, 0.000000000000000000, 1.000000000000000000 ) ) ;
#34615 = LINE ( 'NONE', #38445, #40738 ) ;
#34616 = AXIS2_PLACEMENT_3D ( 'NONE', #10109, #35474, #36114 ) ;
#34617 = CARTESIAN_POINT ( 'NONE',  ( -7.846889724220757145, 122.2670687553216879, -0.7512547164983297554 ) ) ;
#34618 = CARTESIAN_POINT ( 'NONE',  ( -11.17805678602830355, 77.92260723867444483, -1.523999999999998911 ) ) ;
#34619 = CARTESIAN_POINT ( 'NONE',  ( -50.06424591225965059, 20.16147316606144813, 2.291703678227654972 ) ) ;
#34620 = CARTESIAN_POINT ( 'NONE',  ( -0.001640166039862459230, 159.6041700698465036, 0.08208061555506504514 ) ) ;
#34621 = ORIENTED_EDGE ( 'NONE', *, *, #311, .T. ) ;
#34622 = CARTESIAN_POINT ( 'NONE',  ( -47.99264284736476327, 22.55967899981254376, -2.517363275470477113 ) ) ;
#34623 = CARTESIAN_POINT ( 'NONE',  ( -5.815556676244801437, 121.2350703429551686, -0.4688114442016741434 ) ) ;
#34624 = CARTESIAN_POINT ( 'NONE',  ( -7.810699836270218910, 122.5400548736092645, 0.1271298722260623126 ) ) ;
#34625 = VERTEX_POINT ( 'NONE', #23909 ) ;
#34626 = CARTESIAN_POINT ( 'NONE',  ( 1.110063233458014054, 118.7629491485454025, -1.217940297164741059 ) ) ;
#34627 = CARTESIAN_POINT ( 'NONE',  ( -15.55764736111898827, 147.5402044622178153, -0.6398501105574219139 ) ) ;
#34628 = CARTESIAN_POINT ( 'NONE',  ( 5.898638393742167807, -12.20234047945549527, 0.6047796074133310329 ) ) ;
#34629 = CARTESIAN_POINT ( 'NONE',  ( -21.49647223597101942, 141.8478887571778273, 1.286173174470951475 ) ) ;
#34630 = DIRECTION ( 'NONE',  ( -0.3086833358528130455, 0.9511648638205574269, -1.501066210750425580E-13 ) ) ;
#34631 = CARTESIAN_POINT ( 'NONE',  ( 15.17534484293427610, 156.1124880001465556, 0.4370721430752774750 ) ) ;
#34632 = CARTESIAN_POINT ( 'NONE',  ( 14.14780984094775995, 138.8477333867038226, 0.3490212194013133651 ) ) ;
#34633 = FACE_OUTER_BOUND ( 'NONE', #16694, .T. ) ;
#34634 = CARTESIAN_POINT ( 'NONE',  ( 0.8139239711521952803, 26.85569158835278003, 0.5393279072465841928 ) ) ;
#34635 = CARTESIAN_POINT ( 'NONE',  ( -0.8904708500337824573, 116.4394364983335493, -0.05634004476769395586 ) ) ;
#34636 = CARTESIAN_POINT ( 'NONE',  ( -47.23734572760722017, 20.07943206202290298, -5.152903761255795523 ) ) ;
#34637 = CARTESIAN_POINT ( 'NONE',  ( -17.64290547347870941, 83.78857423953914463, -1.270000000000003126 ) ) ;
#34638 = ORIENTED_EDGE ( 'NONE', *, *, #39902, .T. ) ;
#34639 = CARTESIAN_POINT ( 'NONE',  ( -8.528025516331789291, 119.1134116098120046, 0.9763900485721217493 ) ) ;
#34640 = CARTESIAN_POINT ( 'NONE',  ( 0.5082173563136543892, -13.24086043563247728, -4.610200172643778238 ) ) ;
#34641 = CARTESIAN_POINT ( 'NONE',  ( 10.85289063249347485, 119.5270080912504653, 1.298249717235596901 ) ) ;
#34642 = CARTESIAN_POINT ( 'NONE',  ( 16.76200238010684984, 128.5636217276695561, -1.481418206722939335 ) ) ;
#34643 = CARTESIAN_POINT ( 'NONE',  ( -7.510622214715407807, 18.91685342841953954, 3.806420843228597306 ) ) ;
#34644 = CARTESIAN_POINT ( 'NONE',  ( -10.11685142855846564, 157.7687470436769388, -1.412159022929360574 ) ) ;
#34645 = CARTESIAN_POINT ( 'NONE',  ( 4.824598637124480227, 117.6415664293784999, -0.9314390197744758515 ) ) ;
#34646 = CARTESIAN_POINT ( 'NONE',  ( 6.508649675961964753, 120.6419738463991536, 0.3953840990482028750 ) ) ;
#34647 = ORIENTED_EDGE ( 'NONE', *, *, #16675, .F. ) ;
#34648 = CARTESIAN_POINT ( 'NONE',  ( -2.818990841020207139, 121.0122979933374978, 0.009253692138209404852 ) ) ;
#34649 = CARTESIAN_POINT ( 'NONE',  ( -18.69815986816982800, 149.1225091032880528, -2.485088035475524038 ) ) ;
#34651 = CARTESIAN_POINT ( 'NONE',  ( 2.074264724554232053, -15.58053249244904848, 5.900626476732238501 ) ) ;
#34650 = VECTOR ( 'NONE', #39238, 1000.000000000000000 ) ;
#34652 = CIRCLE ( 'NONE', #25787, 6.349999999999999645 ) ;
#34653 = DIRECTION ( 'NONE',  ( 4.017660918040594346E-17, -1.000000000000000000, -2.376309959284834438E-19 ) ) ;
#34654 = DIRECTION ( 'NONE',  ( -0.3256999990547876367, -0.9454731675810326141, -8.328397965208553695E-18 ) ) ;
#34655 = ORIENTED_EDGE ( 'NONE', *, *, #20890, .T. ) ;
#34656 = CARTESIAN_POINT ( 'NONE',  ( 14.41820472940914932, 152.7616507467334372, 2.289036833064873822 ) ) ;
#34657 = DIRECTION ( 'NONE',  ( -0.3256999990547836399, -0.9454731675810339464, 0.000000000000000000 ) ) ;
#34658 = CARTESIAN_POINT ( 'NONE',  ( 1.650612623617701257E-15, 17.14499999999999957, 0.000000000000000000 ) ) ;
#34659 = CARTESIAN_POINT ( 'NONE',  ( -2.040875107092424479, 122.5452913651401587, 0.1521094801190008561 ) ) ;
#34660 = CARTESIAN_POINT ( 'NONE',  ( -6.568537450833661140, -2.023721358670699466, -5.272568914532883788 ) ) ;
#34661 = CARTESIAN_POINT ( 'NONE',  ( 15.61785206596066899, 148.1291547725267037, 1.273309296088947828 ) ) ;
#34662 = CARTESIAN_POINT ( 'NONE',  ( -5.167980139463525191, 115.6909491485453003, -1.237717243154890845 ) ) ;
#34663 = CARTESIAN_POINT ( 'NONE',  ( 9.649066847268002789, 118.2334930433176652, -0.3843608719459136180 ) ) ;
#34664 = CARTESIAN_POINT ( 'NONE',  ( 5.936145915410036444, 56.51500000000000057, -4.381499802576882097 ) ) ;
#34665 = CARTESIAN_POINT ( 'NONE',  ( -58.33727096013997482, -0.2232939613935198409, 0.2257470585846221012 ) ) ;
#34666 = CARTESIAN_POINT ( 'NONE',  ( 5.177913976931196594, 78.94499979771845233, 5.372100000000001430 ) ) ;
#34667 = DIRECTION ( 'NONE',  ( 0.1951894777626589361, 0.9807655518882891776, -6.538892540527331846E-17 ) ) ;
#34669 = CARTESIAN_POINT ( 'NONE',  ( -4.318590049495329097, 118.2119091611040886, 0.3227723479053775102 ) ) ;
#34668 = VECTOR ( 'NONE', #4604, 1000.000000000000000 ) ;
#34670 = CARTESIAN_POINT ( 'NONE',  ( -8.216926545874587262, 117.5004104479096583, -0.1641937475849288286 ) ) ;
#34671 = ORIENTED_EDGE ( 'NONE', *, *, #4075, .F. ) ;
#34672 = CARTESIAN_POINT ( 'NONE',  ( -47.61549956331938915, 19.66157307908738261, 5.197827534590556908 ) ) ;
#34673 = VECTOR ( 'NONE', #31057, 1000.000000000000000 ) ;
#34674 = CARTESIAN_POINT ( 'NONE',  ( 4.042069430835217858, 119.1497344468857875, -0.7634344030164779138 ) ) ;
#34675 = CARTESIAN_POINT ( 'NONE',  ( -2.498958912387992282, 107.2142675576569530, -4.733253560342793875 ) ) ;
#34676 = CARTESIAN_POINT ( 'NONE',  ( -9.680894551640223611, 124.1466939447965814, -0.8054060769509037154 ) ) ;
#34677 = CARTESIAN_POINT ( 'NONE',  ( -6.474089935681887051E-14, 69.94346620154573202, 3.752704589293910110E-29 ) ) ;
#34678 = DIRECTION ( 'NONE',  ( 1.000000000000000000, -9.627370216492862708E-17, 0.000000000000000000 ) ) ;
#34679 = EDGE_CURVE ( 'NONE', #26041, #16908, #15400, .T. ) ;
#34680 = VERTEX_POINT ( 'NONE', #13282 ) ;
#34681 = CARTESIAN_POINT ( 'NONE',  ( 3.979181138743986601, 26.09377549647152961, 2.406711837290479661 ) ) ;
#34682 = CARTESIAN_POINT ( 'NONE',  ( -7.127785904777471870, 78.78377652171661794, 2.231330898844070987 ) ) ;
#34683 = DIRECTION ( 'NONE',  ( 0.2883665106726619465, 0.9575201071113199625, 6.014747832865860437E-16 ) ) ;
#34684 = CARTESIAN_POINT ( 'NONE',  ( -42.07367843439215704, 22.17357734922920187, 1.489526742669803783 ) ) ;
#34685 = CARTESIAN_POINT ( 'NONE',  ( 7.784012320830338005, 122.6313477005580665, 0.1555430910899518460 ) ) ;
#34686 = CARTESIAN_POINT ( 'NONE',  ( 6.999941501148388312, 121.9564690986170916, 0.1592458515995052726 ) ) ;
#34687 = CARTESIAN_POINT ( 'NONE',  ( -2.673854242087471356, 19.56896771519852862, 3.769861741755948348 ) ) ;
#34688 = CARTESIAN_POINT ( 'NONE',  ( 22.33788829447780344, 150.2360280492587776, 1.519312068210846300 ) ) ;
#34689 = CARTESIAN_POINT ( 'NONE',  ( 3.957988466488265633, 104.6144662015457669, -2.766880044203430256 ) ) ;
#34691 = CARTESIAN_POINT ( 'NONE',  ( 5.881556420379451033, 118.2031694463412634, -0.8113220510518367456 ) ) ;
#34690 = CARTESIAN_POINT ( 'NONE',  ( 2.233078627056604759, -15.14192004606506536, 5.083345892419886880 ) ) ;
#34692 = CARTESIAN_POINT ( 'NONE',  ( -2.217461812776308161, 157.2504501563031738, 1.545323669738358774 ) ) ;
#34693 = CARTESIAN_POINT ( 'NONE',  ( 0.5230511744754561265, -14.76557578359995837, -0.8217837604668620788 ) ) ;
#34694 = CARTESIAN_POINT ( 'NONE',  ( -9.590549175011975791, 118.2964180356302961, -0.8317573021886299767 ) ) ;
#34695 = CARTESIAN_POINT ( 'NONE',  ( 0.7990752137124343957, 23.01725015362593396, -0.5559626729366093922 ) ) ;
#34696 = ORIENTED_EDGE ( 'NONE', *, *, #30316, .T. ) ;
#34697 = ADVANCED_FACE ( 'NONE', ( #23054 ), #21793, .T. ) ;
#34698 = CARTESIAN_POINT ( 'NONE',  ( -57.29531047346088712, 2.067549486662559222, 1.749273462387482381 ) ) ;
#34699 = CARTESIAN_POINT ( 'NONE',  ( -8.758948435532792232, 123.3024417045633498, 0.2233049321804339571 ) ) ;
#34700 = CARTESIAN_POINT ( 'NONE',  ( 5.009217890960311337, -13.99182267686448178, 3.873128360714999552 ) ) ;
#34701 = CARTESIAN_POINT ( 'NONE',  ( 13.78713281179550876, 131.0408573235120571, -1.173264656791310534 ) ) ;
#34702 = ORIENTED_EDGE ( 'NONE', *, *, #38026, .T. ) ;
#34703 = CARTESIAN_POINT ( 'NONE',  ( 0.6180999634803059362, 115.7031371519886562, 1.759524179880340267 ) ) ;
#34704 = CARTESIAN_POINT ( 'NONE',  ( -4.871873180668504943, 117.6697712886699350, -1.013429949543328989 ) ) ;
#34705 = CARTESIAN_POINT ( 'NONE',  ( 8.507314851146803747, 123.3280575159016905, 0.1373787248657621640 ) ) ;
#34706 = ORIENTED_EDGE ( 'NONE', *, *, #21414, .F. ) ;
#34707 = CARTESIAN_POINT ( 'NONE',  ( 15.05911097818674094, 125.5446871707752763, 2.024973821723874856 ) ) ;
#34708 = DIRECTION ( 'NONE',  ( 9.627370216492862708E-17, 1.000000000000000000, -0.000000000000000000 ) ) ;
#34709 = DIRECTION ( 'NONE',  ( 0.8572391118119510045, 0.5149185422762100339, 3.573031421855330583E-16 ) ) ;
#34710 = EDGE_CURVE ( 'NONE', #18324, #19839, #34477, .T. ) ;
#34711 = CARTESIAN_POINT ( 'NONE',  ( 0.01887828017110892292, 156.5412816204240301, -0.9447463363288812754 ) ) ;
#34712 = CARTESIAN_POINT ( 'NONE',  ( 13.52003375314293265, 119.6474162840860771, -0.03304800104807574523 ) ) ;
#34713 = ADVANCED_FACE ( 'NONE', ( #34149 ), #30350, .F. ) ;
#34714 = DIRECTION ( 'NONE',  ( -0.8745520943968347893, 0.4849315768086356893, -6.829619984160681712E-16 ) ) ;
#34715 = EDGE_CURVE ( 'NONE', #27671, #22599, #28638, .T. ) ;
#34716 = AXIS2_PLACEMENT_3D ( 'NONE', #11676, #24663, #12102 ) ;
#34717 = CARTESIAN_POINT ( 'NONE',  ( 1.882827824557420815, -15.10077973259936535, 5.845967129181769195 ) ) ;
#34718 = DIRECTION ( 'NONE',  ( -5.188838149069472160E-16, 1.699382548006136559E-16, 1.000000000000000000 ) ) ;
#34719 = CARTESIAN_POINT ( 'NONE',  ( -5.309060684617390516E-14, 83.56599999999998829, 0.000000000000000000 ) ) ;
#34720 = CARTESIAN_POINT ( 'NONE',  ( -4.833760488234558395, 117.8347844218319125, 0.7195636590734230120 ) ) ;
#34721 = ORIENTED_EDGE ( 'NONE', *, *, #20371, .T. ) ;
#34722 = CYLINDRICAL_SURFACE ( 'NONE', #23410, 0.2540000000000031677 ) ;
#34723 = CARTESIAN_POINT ( 'NONE',  ( -3.249327724917783211, 118.4242012496010688, -0.9118293563264334711 ) ) ;
#34724 = CARTESIAN_POINT ( 'NONE',  ( -4.774443427420668407, 116.8297769931967309, -1.047991251433075366 ) ) ;
#34726 = CARTESIAN_POINT ( 'NONE',  ( 4.760793893673167076, 117.5395337211100326, 1.175852012856988926 ) ) ;
#34725 = AXIS2_PLACEMENT_3D ( 'NONE', #10074, #7111, #20069 ) ;
#34727 = CARTESIAN_POINT ( 'NONE',  ( -4.748912967724773004, 117.5371765964522126, -1.178473615865876400 ) ) ;
#34728 = CARTESIAN_POINT ( 'NONE',  ( -0.3798947725662609742, 120.3637084677653633, 0.5835535210198283806 ) ) ;
#34729 = CARTESIAN_POINT ( 'NONE',  ( -3.974385726840726107, -7.478117039488521023, -2.359557994316856533 ) ) ;
#34730 = CARTESIAN_POINT ( 'NONE',  ( 14.60500000000000043, 71.11999999999999034, 5.016499999999999737 ) ) ;
#34731 = DIRECTION ( 'NONE',  ( 0.000000000000000000, 0.000000000000000000, 1.000000000000000000 ) ) ;
#34732 = CARTESIAN_POINT ( 'NONE',  ( 3.513860297840244673, -13.27766151250851756, 2.382095677556017588 ) ) ;
#34733 = CARTESIAN_POINT ( 'NONE',  ( 5.907561988889377780, 118.9932487913337411, -0.3492918592308484338 ) ) ;
#34734 = CARTESIAN_POINT ( 'NONE',  ( -5.838061318223103591, 120.4133487461328826, -1.005638731867922742 ) ) ;
#34735 = CARTESIAN_POINT ( 'NONE',  ( 6.079477277396037493, 121.4435701191419952, 0.1217998136931948000 ) ) ;
#34736 = CARTESIAN_POINT ( 'NONE',  ( -6.442297258278467886, 29.65178619621697464, 0.8020365093557799696 ) ) ;
#34737 = CARTESIAN_POINT ( 'NONE',  ( -0.7270430668245355665, 115.7031259515097474, 1.730794492507717441 ) ) ;
#34738 = CARTESIAN_POINT ( 'NONE',  ( 3.548611814566905664, 16.26088872207684943, 2.983771105379771971 ) ) ;
#34740 = ORIENTED_EDGE ( 'NONE', *, *, #27268, .T. ) ;
#34739 = CARTESIAN_POINT ( 'NONE',  ( 0.9473015597125142850, 116.7004868406603322, 0.2634242240387512646 ) ) ;
#34741 = CARTESIAN_POINT ( 'NONE',  ( 3.700359840729924521, 105.1233170995033959, -3.856631435510931905 ) ) ;
#34742 = CARTESIAN_POINT ( 'NONE',  ( 4.296659151754357531, -15.58794764271442901, 2.529927869898711545 ) ) ;
#34743 = CARTESIAN_POINT ( 'NONE',  ( -10.95471005835515577, 121.6366708983051836, 1.250572042008267548 ) ) ;
#34744 = CARTESIAN_POINT ( 'NONE',  ( -0.9409916986186561694, 26.46864381685040257, -0.2619748070941995688 ) ) ;
#34745 = VECTOR ( 'NONE', #39444, 999.9999999999998863 ) ;
#34746 = CARTESIAN_POINT ( 'NONE',  ( -0.7871466699833823411, 12.39035052102135914, -0.5757299225971378442 ) ) ;
#34747 = ORIENTED_EDGE ( 'NONE', *, *, #12874, .F. ) ;
#34748 = EDGE_LOOP ( 'NONE', ( #4586, #36533, #37, #10664 ) ) ;
#34749 = CARTESIAN_POINT ( 'NONE',  ( 13.73816324777078890, 59.55066437026322745, 5.662797264199856073 ) ) ;
#34750 = CARTESIAN_POINT ( 'NONE',  ( 1.876195077988473292, 107.8038693663528278, 4.521701016168464093 ) ) ;
#34751 = CARTESIAN_POINT ( 'NONE',  ( -12.88338908221817114, 130.8243885708800747, 0.7627239795610335493 ) ) ;
#34752 = DIRECTION ( 'NONE',  ( 5.463695987328526437E-16, -1.000000000000000000, -1.672774450599033775E-31 ) ) ;
#34753 = CARTESIAN_POINT ( 'NONE',  ( 3.416089938271958726, -12.71546774565127080, 1.400931973480754822 ) ) ;
#34754 = CARTESIAN_POINT ( 'NONE',  ( 16.76421760064431865, 140.0893442862094673, -1.556517483701107984 ) ) ;
#34755 = CARTESIAN_POINT ( 'NONE',  ( -14.32444608545413089, 154.4775811199918110, -2.255247442408088165 ) ) ;
#34756 = LINE ( 'NONE', #5591, #29036 ) ;
#34757 = VECTOR ( 'NONE', #27037, 1000.000000000000114 ) ;
#34758 = CARTESIAN_POINT ( 'NONE',  ( -15.52687642492895037, 147.5330934759543879, -0.3102639428822864254 ) ) ;
#34759 = CARTESIAN_POINT ( 'NONE',  ( -5.495523183683928004, 31.57050297546189199, 3.325088329614593885 ) ) ;
#34760 = CARTESIAN_POINT ( 'NONE',  ( 11.98620439842957097, 151.9649008058812569, -0.3157042427443430554 ) ) ;
#34761 = EDGE_CURVE ( 'NONE', #19019, #1397, #35972, .T. ) ;
#34762 = VERTEX_POINT ( 'NONE', #19755 ) ;
#34763 = CARTESIAN_POINT ( 'NONE',  ( 3.096790694169950342, -14.35231825047024401, 1.054797312298405121 ) ) ;
#34764 = DIRECTION ( 'NONE',  ( 0.9454731675810332803, -0.3256999990547855828, 8.537024980200802097E-16 ) ) ;
#34765 = EDGE_CURVE ( 'NONE', #38342, #10310, #18978, .T. ) ;
#34766 = VECTOR ( 'NONE', #34709, 1000.000000000000114 ) ;
#34767 = DIRECTION ( 'NONE',  ( 4.017660918040594346E-17, -1.000000000000000000, -2.376309959284834438E-19 ) ) ;
#34768 = CARTESIAN_POINT ( 'NONE',  ( -57.79860935920279275, 1.496589803099593219, 1.561213607911194901 ) ) ;
#34769 = CARTESIAN_POINT ( 'NONE',  ( -4.449009123739010363, -11.09185097514761331, -1.246716907482375847 ) ) ;
#34770 = CARTESIAN_POINT ( 'NONE',  ( 16.54853992722322786, 147.5857818452174115, 1.770514083359864266 ) ) ;
#34771 = CARTESIAN_POINT ( 'NONE',  ( 3.682264917456193665, 63.33946620154573282, 0.07358041635423968885 ) ) ;
#34772 = CARTESIAN_POINT ( 'NONE',  ( -6.497658445673645033, 120.6500652548963899, 0.1353193420278800130 ) ) ;
#34773 = EDGE_CURVE ( 'NONE', #35331, #14379, #32436, .T. ) ;
#34774 = CARTESIAN_POINT ( 'NONE',  ( -4.595132424582489605, -6.828429371805166959, -0.5093739664528403877 ) ) ;
#34775 = CARTESIAN_POINT ( 'NONE',  ( 12.85860202769631755, 133.7716054015561156, 0.2569454702854388484 ) ) ;
#34776 = CARTESIAN_POINT ( 'NONE',  ( 7.114778624005384522, 4.676967889965610858, -4.534447634950107719 ) ) ;
#34777 = CARTESIAN_POINT ( 'NONE',  ( -57.82296528090891030, 0.8544030886276504644, -0.9114307699690453735 ) ) ;
#34778 = CARTESIAN_POINT ( 'NONE',  ( -8.740223524600960303, 117.9165407173578899, -0.6868026839525182003 ) ) ;
#34779 = CARTESIAN_POINT ( 'NONE',  ( 0.01331772328987725074, 119.9741034315943864, -0.6664733318051296873 ) ) ;
#34780 = CARTESIAN_POINT ( 'NONE',  ( -10.75478607932181241, 82.07015292912137738, 1.269999999999999796 ) ) ;
#34781 = DIRECTION ( 'NONE',  ( -4.017660918040594346E-17, 1.000000000000000000, 2.376309959284834438E-19 ) ) ;
#34782 = CIRCLE ( 'NONE', #4874, 0.6350000000000001199 ) ;
#34783 = CARTESIAN_POINT ( 'NONE',  ( -3.982871878373832164, -5.105173558950587775, 7.419718595111914894 ) ) ;
#34784 = DIRECTION ( 'NONE',  ( -0.8745520943968249084, 0.4849315768086534528, -5.361993529360573944E-16 ) ) ;
#34785 = CARTESIAN_POINT ( 'NONE',  ( 4.897655256226217446, 56.53910281269280347, -5.081330806033660608 ) ) ;
#34786 = CARTESIAN_POINT ( 'NONE',  ( 0.9126123168628460514, 122.5862318000603182, -0.2067773319678722355 ) ) ;
#34787 = CARTESIAN_POINT ( 'NONE',  ( -0.3287531253415878485, 116.7093555017326452, 0.2203909396130739051 ) ) ;
#34788 = ORIENTED_EDGE ( 'NONE', *, *, #13898, .T. ) ;
#34789 = CARTESIAN_POINT ( 'NONE',  ( -58.83227707057485389, -0.08366279997994163775, -5.898546760656774196E-15 ) ) ;
#34790 = EDGE_LOOP ( 'NONE', ( #3339, #16383, #6059, #39051, #37589, #25730, #24717, #584 ) ) ;
#34791 = CARTESIAN_POINT ( 'NONE',  ( -41.34781391883380053, 22.78346824044358954, -1.529410470714712700 ) ) ;
#34793 = CARTESIAN_POINT ( 'NONE',  ( -8.871044653442362815, 123.8953218705242421, -0.08906294657775859491 ) ) ;
#34792 = AXIS2_PLACEMENT_3D ( 'NONE', #41266, #14622, #12287 ) ;
#34794 = CARTESIAN_POINT ( 'NONE',  ( 2.825551972395176303, -15.60239892947398666, 5.624417742107700846 ) ) ;
#34795 = CARTESIAN_POINT ( 'NONE',  ( -2.242939865367220342, 118.2767885243204944, 0.6835633642702236834 ) ) ;
#34796 = CARTESIAN_POINT ( 'NONE',  ( 1.091392056212987960, 117.4935207075373569, -0.4954137919519207012 ) ) ;
#34797 = CARTESIAN_POINT ( 'NONE',  ( 0.1710433496020407063, 14.98650505531991506, 4.637963194678765610 ) ) ;
#34798 = CARTESIAN_POINT ( 'NONE',  ( -14.58714721168234796, 120.3300541288867862, -0.7025926276034525353 ) ) ;
#34799 = CARTESIAN_POINT ( 'NONE',  ( -57.92803731934569811, 1.218056268468654002, -1.434962409700567987 ) ) ;
#34800 = ORIENTED_EDGE ( 'NONE', *, *, #25087, .F. ) ;
#34801 = CARTESIAN_POINT ( 'NONE',  ( 8.797014378848668770, 117.6856624139819445, 0.2140604904457499569 ) ) ;
#34802 = DIRECTION ( 'NONE',  ( 0.6825627711659328911, 0.7308269722843309113, 2.299753143848213649E-16 ) ) ;
#34803 = CARTESIAN_POINT ( 'NONE',  ( -3.432158483474483379, 119.7942873563901713, 0.6544105580379842024 ) ) ;
#34804 = CARTESIAN_POINT ( 'NONE',  ( -6.519774838065697039E-14, 78.83346620154574680, 1.207165459601591275E-19 ) ) ;
#34805 = CARTESIAN_POINT ( 'NONE',  ( 1.037157837436363916, 157.7941190989783991, -1.604419329240821979 ) ) ;
#34806 = TOROIDAL_SURFACE ( 'NONE', #19814, 0.3809999999999999498, 0.2540000000000000036 ) ;
#34807 = CARTESIAN_POINT ( 'NONE',  ( -20.93418857319378645, 149.0309112320384486, -2.352213276463849034 ) ) ;
#34808 = CARTESIAN_POINT ( 'NONE',  ( -56.26318288983030413, 4.268071985104968213, -2.480832006587858185 ) ) ;
#34809 = CARTESIAN_POINT ( 'NONE',  ( 3.624202338748673036, 120.7384399880717467, -0.3073100964232672316 ) ) ;
#34810 = ORIENTED_EDGE ( 'NONE', *, *, #29749, .T. ) ;
#34811 = CARTESIAN_POINT ( 'NONE',  ( -12.41677917861200164, 153.6617311634574037, -2.127417120026096953 ) ) ;
#34812 = CARTESIAN_POINT ( 'NONE',  ( 4.057567908148627112, -15.53776324113162488, 2.457816012360223290 ) ) ;
#34813 = AXIS2_PLACEMENT_3D ( 'NONE', #24441, #5724, #37445 ) ;
#34814 = CARTESIAN_POINT ( 'NONE',  ( -4.250359704263266813, 118.2244096797001731, -0.4633146300828262509 ) ) ;
#34815 = TOROIDAL_SURFACE ( 'NONE', #3549, 5.080000000000005400, 0.5080000000000000071 ) ;
#34816 = CARTESIAN_POINT ( 'NONE',  ( -58.75009580408200094, 0.1057190229620807997, -0.6617493214611014363 ) ) ;
#34817 = CIRCLE ( 'NONE', #34716, 3.683000000000001162 ) ;
#34818 = CARTESIAN_POINT ( 'NONE',  ( -4.825875739449531743, 117.4745444320467129, 0.9994230495043341378 ) ) ;
#34819 = CARTESIAN_POINT ( 'NONE',  ( 10.01853622893594853, 122.3915136462027817, 1.471741716425344570 ) ) ;
#34820 = FACE_BOUND ( 'NONE', #38275, .T. ) ;
#34821 = EDGE_CURVE ( 'NONE', #27053, #21375, #17988, .T. ) ;
#34822 = EDGE_CURVE ( 'NONE', #6660, #1790, #20167, .T. ) ;
#34823 = CARTESIAN_POINT ( 'NONE',  ( 4.223004820120735303, -0.3563183945215069870, -7.287282906663286930 ) ) ;
#34824 = CARTESIAN_POINT ( 'NONE',  ( 15.55764736111886037, 147.5402044622178153, 0.6398501105574221359 ) ) ;
#34825 = CARTESIAN_POINT ( 'NONE',  ( -55.60486134785667645, 7.243031971518515633, -3.140198620020504094 ) ) ;
#34827 = ORIENTED_EDGE ( 'NONE', *, *, #17569, .T. ) ;
#34826 = DIRECTION ( 'NONE',  ( -5.188838149069471174E-16, 1.699382548006136313E-16, 1.000000000000000000 ) ) ;
#34828 = CARTESIAN_POINT ( 'NONE',  ( -1.043075768918328983, 117.9394518566729033, 1.353628448391521077 ) ) ;
#34829 = DIRECTION ( 'NONE',  ( 0.7308269722843147020, -0.6825627711659504326, 8.537024980200894788E-16 ) ) ;
#34830 = CARTESIAN_POINT ( 'NONE',  ( -7.962997644397243668, 121.6654936142849692, -1.110444070604056366 ) ) ;
#34831 = CARTESIAN_POINT ( 'NONE',  ( -58.37241122568489970, -0.2962816677228030660, -1.043042736874535760E-14 ) ) ;
#34832 = CARTESIAN_POINT ( 'NONE',  ( -49.81807968324856972, 18.07223176367294570, 4.612844822355046226 ) ) ;
#34833 = CARTESIAN_POINT ( 'NONE',  ( -23.10641284836741960, 149.8968678342272653, -0.3080169626343541300 ) ) ;
#34834 = ORIENTED_EDGE ( 'NONE', *, *, #10562, .F. ) ;
#34835 = CARTESIAN_POINT ( 'NONE',  ( -49.29989578322635424, 20.38947471906982756, -3.123819567266207464 ) ) ;
#34836 = CARTESIAN_POINT ( 'NONE',  ( 6.959716963148959046, 121.9406942131701754, -0.009715431953628055062 ) ) ;
#34837 = FACE_OUTER_BOUND ( 'NONE', #18279, .T. ) ;
#34838 = ORIENTED_EDGE ( 'NONE', *, *, #3434, .T. ) ;
#34839 = CARTESIAN_POINT ( 'NONE',  ( 0.9195240100825864404, 115.7029491485453434, -1.717302178571716409 ) ) ;
#34840 = CARTESIAN_POINT ( 'NONE',  ( -8.097005894254575509, 122.8525693413601800, -0.3074703907764577693 ) ) ;
#34841 = CARTESIAN_POINT ( 'NONE',  ( 3.183750377336629356, -15.03749083096926675, 5.611903928707999256 ) ) ;
#34842 = CARTESIAN_POINT ( 'NONE',  ( -10.77577921906396163, 119.6772744462923157, 0.9367561965627281273 ) ) ;
#34843 = CARTESIAN_POINT ( 'NONE',  ( 5.496588887047727745, 78.91991874857603761, -5.121802412194443654 ) ) ;
#34844 = CIRCLE ( 'NONE', #40301, 3.683000000000001162 ) ;
#34845 = CARTESIAN_POINT ( 'NONE',  ( 23.30140632484780383, 142.7201128741078833, 0.7978754358820902004 ) ) ;
#34846 = CARTESIAN_POINT ( 'NONE',  ( 2.884051542275651414, 156.0957788938021054, 0.05763021347587640730 ) ) ;
#34847 = B_SPLINE_CURVE_WITH_KNOTS ( 'NONE', 3,
 ( #18187, #8198, #24801, #4820 ),
 .UNSPECIFIED., .F., .F.,
 ( 4, 4 ),
 ( 0.000000000000000000, 1.000000000000000000 ),
 .UNSPECIFIED. ) ;
#34848 = CARTESIAN_POINT ( 'NONE',  ( -10.93398011767285283, 82.89560043784887000, -1.269999999999999352 ) ) ;
#34849 = CARTESIAN_POINT ( 'NONE',  ( 0.1724166890850278577, 29.87817833284422875, -0.9617850639438362270 ) ) ;
#34850 = CARTESIAN_POINT ( 'NONE',  ( -1.814945173922756227, 116.4909138135563040, -0.1082358691141156737 ) ) ;
#34851 = LINE ( 'NONE', #2486, #26330 ) ;
#34852 = DIRECTION ( 'NONE',  ( 0.000000000000000000, -1.000000000000000000, -0.000000000000000000 ) ) ;
#34853 = ORIENTED_EDGE ( 'NONE', *, *, #30047, .T. ) ;
#34854 = CARTESIAN_POINT ( 'NONE',  ( -6.156441858550770085, 118.9979555525181496, 0.9955410089892811065 ) ) ;
#34855 = CARTESIAN_POINT ( 'NONE',  ( 4.581716828367337513, -15.30239761468843973, -0.5121115983836379559 ) ) ;
#34856 = CARTESIAN_POINT ( 'NONE',  ( 21.62407820142100690, 149.9601031839316079, 2.013249247985050783 ) ) ;
#34857 = CARTESIAN_POINT ( 'NONE',  ( 12.92430874792252560, 121.9120276846612256, -1.237792553996327261 ) ) ;
#34858 = CARTESIAN_POINT ( 'NONE',  ( 4.500746820419270655, 24.54286538861932598, -7.153999163526271410 ) ) ;
#34859 = CARTESIAN_POINT ( 'NONE',  ( -7.493104803958972049, 158.4854300789945398, -1.293057490532128151 ) ) ;
#34860 = CARTESIAN_POINT ( 'NONE',  ( 4.766322966312536380, 117.7281155096933674, -0.9072089781911022444 ) ) ;
#34861 = CARTESIAN_POINT ( 'NONE',  ( 5.210105874137030746, 116.2501875120488393, 1.173469071234783723 ) ) ;
#34862 = CIRCLE ( 'NONE', #27372, 0.2539999999999983937 ) ;
#34863 = CARTESIAN_POINT ( 'NONE',  ( -5.999396524113779883, 155.3621521873626534, 0.05839828084409132841 ) ) ;
#34864 = CARTESIAN_POINT ( 'NONE',  ( -18.57576200519322640, 149.2887123452801745, -2.480868434872863126 ) ) ;
#34865 = CARTESIAN_POINT ( 'NONE',  ( 2.105506875138051459, -15.57594099408041188, 5.887502213194136580 ) ) ;
#34866 = DIRECTION ( 'NONE',  ( -4.017660918040594346E-17, 1.000000000000000000, 2.376309959284834438E-19 ) ) ;
#34867 = CARTESIAN_POINT ( 'NONE',  ( -46.60530155212503445, 26.17382724835477958, -1.524000000000008459 ) ) ;
#34868 = ORIENTED_EDGE ( 'NONE', *, *, #31919, .F. ) ;
#34869 = CARTESIAN_POINT ( 'NONE',  ( 11.21148455117555898, 122.4230570912197038, 1.693600966768365357 ) ) ;
#34870 = DIRECTION ( 'NONE',  ( -0.1469470846586743706, -9.335746474409589170E-17, -0.9891443546370348727 ) ) ;
#34871 = CARTESIAN_POINT ( 'NONE',  ( -27.97106122948731155, 77.87043919753004673, 1.523999999999992028 ) ) ;
#34872 = AXIS2_PLACEMENT_3D ( 'NONE', #31525, #2369, #15327 ) ;
#34873 = CARTESIAN_POINT ( 'NONE',  ( -3.079316153087905850, 123.1875568577169560, 0.05586128712921783340 ) ) ;
#34874 = CARTESIAN_POINT ( 'NONE',  ( 2.619848522501802446, -13.46771402114085703, -8.002427727062926266 ) ) ;
#34875 = CARTESIAN_POINT ( 'NONE',  ( 15.73537819279951755, 147.9505201145231865, 1.277015258756127869 ) ) ;
#34876 = CARTESIAN_POINT ( 'NONE',  ( -4.727273527973792078, 118.5930653697794384, -1.020421541027422219 ) ) ;
#34877 = EDGE_CURVE ( 'NONE', #41561, #40395, #32306, .T. ) ;
#34878 = CARTESIAN_POINT ( 'NONE',  ( 22.93637923037181992, 149.5023856264156450, -0.3943874666890923586 ) ) ;
#34879 = CARTESIAN_POINT ( 'NONE',  ( 4.737240446979628317, 56.51499999999997215, -4.914899999999988722 ) ) ;
#34880 = CARTESIAN_POINT ( 'NONE',  ( -58.24403404964675701, -0.02353476031055234952, 0.4695906566965602491 ) ) ;
#34881 = DIRECTION ( 'NONE',  ( -5.188838149069472160E-16, 1.699382548006136559E-16, 1.000000000000000000 ) ) ;
#34882 = DIRECTION ( 'NONE',  ( 0.1565721916418034432, 0.9876665170007953298, -8.659954811667511346E-17 ) ) ;
#34883 = CARTESIAN_POINT ( 'NONE',  ( -5.638141748386694907, 56.51500000000081769, 5.060111600421964617 ) ) ;
#34884 = AXIS2_PLACEMENT_3D ( 'NONE', #8194, #2027, #5020 ) ;
#34885 = DIRECTION ( 'NONE',  ( -0.8745520943968235761, 0.4849315768086558953, -5.361993529360570985E-16 ) ) ;
#34886 = ORIENTED_EDGE ( 'NONE', *, *, #26690, .F. ) ;
#34887 = CARTESIAN_POINT ( 'NONE',  ( -50.82551848962686591, 16.13924203555649228, 4.804203053272154911 ) ) ;
#34888 =( BOUNDED_CURVE ( )  B_SPLINE_CURVE ( 2, ( #16261, #3726, #32468 ),
 .UNSPECIFIED., .F., .T. ) 
 B_SPLINE_CURVE_WITH_KNOTS ( ( 3, 3 ),
 ( 0.000000000000000000, 1.000000000000000000 ),
 .UNSPECIFIED. ) 
 CURVE ( )  GEOMETRIC_REPRESENTATION_ITEM ( )  RATIONAL_B_SPLINE_CURVE ( ( 1.000000000000000000, 0.4190531958282215919, 1.000000000000000000 ) ) 
 REPRESENTATION_ITEM ( '' )  );
#34889 = CARTESIAN_POINT ( 'NONE',  ( -8.215589217028934854, 120.4019796500743809, -1.435742804604346556 ) ) ;
#34890 = CARTESIAN_POINT ( 'NONE',  ( -1.987587706212319727, 106.6795586461009009, -4.969950645211479667 ) ) ;
#34891 = CARTESIAN_POINT ( 'NONE',  ( -8.259016884199036568, 122.7564308547279666, -0.6276379194545151918 ) ) ;
#34892 = CARTESIAN_POINT ( 'NONE',  ( -29.36432400326824066, 68.35621600878259585, 1.523999999999992916 ) ) ;
#34893 = FACE_OUTER_BOUND ( 'NONE', #8924, .T. ) ;
#34894 = ORIENTED_EDGE ( 'NONE', *, *, #21122, .F. ) ;
#34895 = CARTESIAN_POINT ( 'NONE',  ( 4.636458409304901274, 17.36039413176390411, -0.09481320587925551324 ) ) ;
#34896 = CARTESIAN_POINT ( 'NONE',  ( -29.22020851875563352, 63.09400180735026709, 1.270000000000041540 ) ) ;
#34897 = CARTESIAN_POINT ( 'NONE',  ( -3.911441847776591985, 70.75305732235845824, 1.270000000000006235 ) ) ;
#34898 = CYLINDRICAL_SURFACE ( 'NONE', #15596, 0.2540000000000052771 ) ;
#34899 = CARTESIAN_POINT ( 'NONE',  ( -23.62918761621517305, 82.45577215708875940, -1.270000000000006013 ) ) ;
#34900 = CARTESIAN_POINT ( 'NONE',  ( -6.995832315028981618, 121.9523011290228283, -0.1203680031076684170 ) ) ;
#34901 = DIRECTION ( 'NONE',  ( -0.01731298258488817021, 0.9998501190848633202, 8.235542606122962463E-15 ) ) ;
#34902 = CARTESIAN_POINT ( 'NONE',  ( 15.18175346423885230, 121.1469641333237917, 1.070035192906481303 ) ) ;
#34903 = CARTESIAN_POINT ( 'NONE',  ( -10.92199999999999704, 12.96416000000000146, 0.000000000000000000 ) ) ;
#34905 = CARTESIAN_POINT ( 'NONE',  ( 21.50873886539572410, 148.9071063441643048, -1.383230070950766777 ) ) ;
#34904 = CARTESIAN_POINT ( 'NONE',  ( 5.256666791691227303, 57.14999999999997726, 5.296388421271908342 ) ) ;
#34906 = CARTESIAN_POINT ( 'NONE',  ( -11.76378629788681174, 123.2143981803894093, 1.250304744737055440 ) ) ;
#34907 = CARTESIAN_POINT ( 'NONE',  ( 0.4006815055314144058, 20.64345356492705719, 4.603752038498275745 ) ) ;
#34908 = CARTESIAN_POINT ( 'NONE',  ( -2.883180212088917393, 116.9538966677400254, -0.4754005367760562040 ) ) ;
#34909 = CIRCLE ( 'NONE', #16523, 2.857500000000000817 ) ;
#34910 = CARTESIAN_POINT ( 'NONE',  ( -0.06925455797148694081, -4.192134993018743927, -0.9746272421430232091 ) ) ;
#34911 = B_SPLINE_CURVE_WITH_KNOTS ( 'NONE', 3,
 ( #40404, #1012, #594, #20150, #26771, #20352, #10995, #30588, #32965, #16959, #11198, #39781, #6974 ),
 .UNSPECIFIED., .F., .F.,
 ( 4, 1, 1, 1, 1, 1, 1, 1, 1, 1, 4 ),
 ( 0.000000000000000000, 0.1249999999999999167, 0.1767086109055020227, 0.2499999999999998335, 0.3750000000000003886, 0.5000000000000003331, 0.5890287030183404271, 0.6249999999999998890, 0.7499999999999995559, 0.8749999999999997780, 1.000000000000000000 ),
 .UNSPECIFIED. ) ;
#34912 = ORIENTED_EDGE ( 'NONE', *, *, #37945, .F. ) ;
#34913 = CARTESIAN_POINT ( 'NONE',  ( -55.10067240196883631, 5.634149028679341420, 0.4880682687715845458 ) ) ;
#34914 = CARTESIAN_POINT ( 'NONE',  ( -16.01386893308431780, 146.3393691146323761, 0.4087692286948390596 ) ) ;
#34915 = ADVANCED_FACE ( 'NONE', ( #23113 ), #13132, .F. ) ;
#34916 = CARTESIAN_POINT ( 'NONE',  ( 5.365742231761132963, -12.30384844886438245, 1.459887348375163096 ) ) ;
#34917 = CARTESIAN_POINT ( 'NONE',  ( 12.98740932513240764, 152.2092440956282076, -1.257387005612584652 ) ) ;
#34918 = ORIENTED_EDGE ( 'NONE', *, *, #16264, .F. ) ;
#34919 = CARTESIAN_POINT ( 'NONE',  ( 1.183385436418662007, 115.7029491485453008, 1.742418698461533522 ) ) ;
#34920 = AXIS2_PLACEMENT_3D ( 'NONE', #6167, #35971, #19340 ) ;
#34921 = ORIENTED_EDGE ( 'NONE', *, *, #31930, .T. ) ;
#34922 = CARTESIAN_POINT ( 'NONE',  ( -4.825672693197581964, 117.7347280262817293, -1.017632466350065990 ) ) ;
#34923 = EDGE_CURVE ( 'NONE', #37655, #8441, #18129, .T. ) ;
#34924 = CARTESIAN_POINT ( 'NONE',  ( 6.503408402854558013, 121.7799126398724354, 0.1299535771408518448 ) ) ;
#34925 = VERTEX_POINT ( 'NONE', #9725 ) ;
#34926 = CARTESIAN_POINT ( 'NONE',  ( 19.79373099999700258, 147.4002846799066333, 2.520905760949471386 ) ) ;
#34927 = DIRECTION ( 'NONE',  ( 0.01997839162482749689, 1.040247600000945640E-18, -0.9998004120163610509 ) ) ;
#34928 = CARTESIAN_POINT ( 'NONE',  ( 15.70103477329399766, 145.5797129992483292, 0.3137440411564567100 ) ) ;
#34929 = EDGE_CURVE ( 'NONE', #588, #33761, #26329, .T. ) ;
#34930 = CARTESIAN_POINT ( 'NONE',  ( 4.799155079147907621, 117.4716649492776241, -1.004620440989309138 ) ) ;
#34931 = CARTESIAN_POINT ( 'NONE',  ( 20.20614143541403962, 128.9119615565081176, 0.01722291150864752388 ) ) ;
#34932 = DIRECTION ( 'NONE',  ( -0.000000000000000000, 0.000000000000000000, -1.000000000000000000 ) ) ;
#34933 =( GEOMETRIC_REPRESENTATION_CONTEXT ( 3 ) GLOBAL_UNCERTAINTY_ASSIGNED_CONTEXT ( ( #15482 ) ) GLOBAL_UNIT_ASSIGNED_CONTEXT ( ( #14434, #34058, #13613 ) ) REPRESENTATION_CONTEXT ( 'NONE', 'WORKASPACE' ) );
#34934 = CARTESIAN_POINT ( 'NONE',  ( -46.92362637188625740, 25.23517642483339074, 1.818802264970843519 ) ) ;
#34935 = CARTESIAN_POINT ( 'NONE',  ( 5.435468916198098022, 78.92497954178514874, 5.153742819108977358 ) ) ;
#34936 = CARTESIAN_POINT ( 'NONE',  ( 1.753189578010867056, -15.12811351701386009, 5.597763803460143350 ) ) ;
#34937 = CARTESIAN_POINT ( 'NONE',  ( -46.40591231939538375, 23.70796668624020853, 2.618124260499386402 ) ) ;
#34938 = CARTESIAN_POINT ( 'NONE',  ( -6.552964542248172189E-14, 78.83346620154574680, -6.511376220759049693E-18 ) ) ;
#34939 = EDGE_CURVE ( 'NONE', #28134, #23250, #22194, .T. ) ;
#34940 = TOROIDAL_SURFACE ( 'NONE', #36314, 8.794749999999996959, 0.2540000000000000036 ) ;
#34941 = CARTESIAN_POINT ( 'NONE',  ( -4.751290763676331963, 117.9442343397520290, 0.6305581417652982301 ) ) ;
#34942 = ORIENTED_EDGE ( 'NONE', *, *, #8676, .T. ) ;
#34943 = CARTESIAN_POINT ( 'NONE',  ( -7.772068811996249771, 69.25462295839062676, -1.523999999999995580 ) ) ;
#34944 = CARTESIAN_POINT ( 'NONE',  ( -8.466947760633088294, 119.1862599057703846, -1.332611659245268365 ) ) ;
#34945 = CARTESIAN_POINT ( 'NONE',  ( -3.094730188726814823, 108.9521120498200730, -4.030551393973050622 ) ) ;
#34946 = CARTESIAN_POINT ( 'NONE',  ( 4.590341383356626892, 117.9757822827139222, 0.9229197263701504061 ) ) ;
#34947 = CARTESIAN_POINT ( 'NONE',  ( 3.150244473240279675, -14.07033042043420146, 1.813758411523331393 ) ) ;
#34948 = CARTESIAN_POINT ( 'NONE',  ( -0.4165637647021588341, 124.3520329708341023, 0.05485040398408839307 ) ) ;
#34949 = AXIS2_PLACEMENT_3D ( 'NONE', #21231, #10823, #24018 ) ;
#34950 = SURFACE_STYLE_FILL_AREA ( #18517 ) ;
#34951 = CARTESIAN_POINT ( 'NONE',  ( -58.83227707057486811, -0.08366279997995551554, -1.529465441686574059E-14 ) ) ;
#34952 = LINE ( 'NONE', #28545, #22580 ) ;
#34953 = CARTESIAN_POINT ( 'NONE',  ( 2.055333930833562750, 107.8038693663528278, -4.443139710053165103 ) ) ;
#34954 = CARTESIAN_POINT ( 'NONE',  ( -0.5409540667465209118, 119.9180165495073283, -0.4819738915938376889 ) ) ;
#34955 = CARTESIAN_POINT ( 'NONE',  ( 5.064182118629766194, 117.2683359310143913, -0.4803582174348582923 ) ) ;
#34956 = CARTESIAN_POINT ( 'NONE',  ( -5.682669411112049040, 29.64564914382334138, 2.717066260770635289 ) ) ;
#34957 = CARTESIAN_POINT ( 'NONE',  ( -6.135835944515187101, 77.40800365160224317, -1.523999999999996247 ) ) ;
#34958 = CARTESIAN_POINT ( 'NONE',  ( 2.829288187452689396, 6.340478445469713620, 3.655570690059357197 ) ) ;
#34960 = ORIENTED_EDGE ( 'NONE', *, *, #3230, .T. ) ;
#34959 = CARTESIAN_POINT ( 'NONE',  ( 21.76232006938114694, 151.4242408681541008, 1.019401482499525891 ) ) ;
#34961 = CARTESIAN_POINT ( 'NONE',  ( 3.944319131782805243, 105.1226808459336866, -3.607269903450494919 ) ) ;
#34962 = CARTESIAN_POINT ( 'NONE',  ( 4.174810697594108611, -15.62279056926031728, 2.935701831792822514 ) ) ;
#34963 = CARTESIAN_POINT ( 'NONE',  ( -13.20509474233035263, 123.8872625266795211, 1.378179767694161395 ) ) ;
#34964 = CARTESIAN_POINT ( 'NONE',  ( -0.07513956969218944792, 19.57165678886816096, 0.9711860325417217554 ) ) ;
#34965 = CARTESIAN_POINT ( 'NONE',  ( -0.3507176028818052571, 11.51684809748499028, -0.9106068057588879716 ) ) ;
#34966 = EDGE_CURVE ( 'NONE', #7672, #30817, #37874, .T. ) ;
#34967 = EDGE_LOOP ( 'NONE', ( #38108, #38546, #20907, #8207 ) ) ;
#34968 = VERTEX_POINT ( 'NONE', #26124 ) ;
#34969 = DIRECTION ( 'NONE',  ( 0.1565721916417901483, 0.9876665170007974393, 0.000000000000000000 ) ) ;
#34970 = CARTESIAN_POINT ( 'NONE',  ( 3.448667622495753982, 119.7720183225874138, 0.5479595714127597494 ) ) ;
#34971 = CARTESIAN_POINT ( 'NONE',  ( -15.38818086081976766, 149.0334586719817764, 0.9521378535654884123 ) ) ;
#34972 = LINE ( 'NONE', #21432, #22491 ) ;
#34973 = CARTESIAN_POINT ( 'NONE',  ( 3.154356104639033820, -12.65568165217861818, 0.8785170097314246584 ) ) ;
#34974 = CARTESIAN_POINT ( 'NONE',  ( 11.03120429849336226, 123.2082810311540300, -1.124825114493487321 ) ) ;
#34975 = AXIS2_PLACEMENT_3D ( 'NONE', #29958, #20777, #3790 ) ;
#34976 = CARTESIAN_POINT ( 'NONE',  ( -19.08488522674174703, 150.4642993720107143, -2.434974558521497912 ) ) ;
#34977 = CARTESIAN_POINT ( 'NONE',  ( 9.132817075745611705E-16, 9.026346327358515609, 0.000000000000000000 ) ) ;
#34978 = ADVANCED_FACE ( 'NONE', ( #39126 ), #29539, .T. ) ;
#34979 = CARTESIAN_POINT ( 'NONE',  ( 8.567507150466024513, 118.7110241784669427, 1.177141029754138479 ) ) ;
#34980 = CARTESIAN_POINT ( 'NONE',  ( -5.871471797037544071, 31.01275966357848901, 2.875548327037550589 ) ) ;
#34981 = CARTESIAN_POINT ( 'NONE',  ( 9.115521395012498473, 123.9337093609977529, -0.04715588286475763669 ) ) ;
#34982 = CIRCLE ( 'NONE', #2321, 0.5080000000000000071 ) ;
#34983 = ORIENTED_EDGE ( 'NONE', *, *, #16719, .F. ) ;
#34984 = FACE_OUTER_BOUND ( 'NONE', #1718, .T. ) ;
#34985 = DIRECTION ( 'NONE',  ( 0.1906721105965040186, -0.9816537812491095139, 2.657572025465703189E-16 ) ) ;
#34986 = DIRECTION ( 'NONE',  ( -9.627370216492862708E-17, -1.000000000000000000, 0.000000000000000000 ) ) ;
#34987 = VECTOR ( 'NONE', #22108, 1000.000000000000000 ) ;
#34988 = CARTESIAN_POINT ( 'NONE',  ( -13.17422243436020857, 17.14500000000000668, 5.016499999999999737 ) ) ;
#34989 = CARTESIAN_POINT ( 'NONE',  ( 5.629075615873821548, 21.71503808657377022, 6.277010319805454763 ) ) ;
#34990 = CARTESIAN_POINT ( 'NONE',  ( 2.605661685743386968, 120.2926465633240127, 0.5460719465365780900 ) ) ;
#34991 = DIRECTION ( 'NONE',  ( -4.017660918040594346E-17, 1.000000000000000000, 2.376309959284834438E-19 ) ) ;
#34992 = CARTESIAN_POINT ( 'NONE',  ( 21.64725176087509340, 132.7051459832101443, 0.3678724904816470520 ) ) ;
#34993 = CARTESIAN_POINT ( 'NONE',  ( -5.398477100378502591, 117.1940586887245388, 0.6826447346010612316 ) ) ;
#34994 = VECTOR ( 'NONE', #6776, 1000.000000000000000 ) ;
#34995 = CARTESIAN_POINT ( 'NONE',  ( 3.745621265272091716, -10.50169880513956322, -2.708184146228840294 ) ) ;
#34996 = CARTESIAN_POINT ( 'NONE',  ( 15.76285804746341235, 145.9067145067653541, 0.3149794173055769919 ) ) ;
#34997 = EDGE_CURVE ( 'NONE', #36577, #12023, #10376, .T. ) ;
#34998 = CARTESIAN_POINT ( 'NONE',  ( -8.417729735924666556, -0.9468307554896212563, 0.2322036382352700989 ) ) ;
#34999 = CARTESIAN_POINT ( 'NONE',  ( -2.143513273935226948, 116.5966001900618494, -0.4290450327811727860 ) ) ;
#35000 = CARTESIAN_POINT ( 'NONE',  ( 0.09934209769091897901, 106.7790779034713324, -4.971484795507141285 ) ) ;
#35001 = AXIS2_PLACEMENT_3D ( 'NONE', #33130, #23295, #7773 ) ;
#35002 = DIRECTION ( 'NONE',  ( 4.017660918040594346E-17, -1.000000000000000000, -2.376309959284834438E-19 ) ) ;
#35003 = DIRECTION ( 'NONE',  ( 0.7258741224862652608, -0.6878275643682757456, 8.537024980200906621E-16 ) ) ;
#35004 = CARTESIAN_POINT ( 'NONE',  ( -6.147169039531121371, -7.901875862888119606, -5.777837204501876656 ) ) ;
#35005 = CARTESIAN_POINT ( 'NONE',  ( 3.361427982427648065, 117.3993835122936247, 1.373626019692422817 ) ) ;
#35006 = CARTESIAN_POINT ( 'NONE',  ( -41.26650320839694785, 23.23696823412479873, 1.523999999999994248 ) ) ;
#35007 = FACE_OUTER_BOUND ( 'NONE', #29011, .T. ) ;
#35008 = CARTESIAN_POINT ( 'NONE',  ( 0.1698098321966529933, 106.7790779034713324, -4.970076682467829521 ) ) ;
#35009 = CARTESIAN_POINT ( 'NONE',  ( -3.228502273017121560, 159.4348965051207756, 0.3922148187338913572 ) ) ;
#35010 = ORIENTED_EDGE ( 'NONE', *, *, #16531, .F. ) ;
#35011 = ADVANCED_FACE ( 'NONE', ( #6749 ), #12916, .T. ) ;
#35012 = CARTESIAN_POINT ( 'NONE',  ( -58.73915225836899623, 0.1638436772961326948, -0.01855759196812271222 ) ) ;
#35013 = EDGE_LOOP ( 'NONE', ( #4109, #30212, #6304, #4881 ) ) ;
#35014 = CARTESIAN_POINT ( 'NONE',  ( -41.09676540851936011, 23.04694042099055196, -1.523999999999985588 ) ) ;
#35015 = CARTESIAN_POINT ( 'NONE',  ( -15.78555315239537116, 146.2345694261926496, -0.1810740433878625377 ) ) ;
#35016 = CARTESIAN_POINT ( 'NONE',  ( 6.400388595320081642, -14.10124341269280990, -0.01754875274584842895 ) ) ;
#35017 = CARTESIAN_POINT ( 'NONE',  ( -4.766456943369862920, 158.1906701298835856, 1.576320697809042937 ) ) ;
#35018 = CARTESIAN_POINT ( 'NONE',  ( 0.008308726997667138792, 117.3658353995175503, -0.4158026747930029243 ) ) ;
#35019 = CARTESIAN_POINT ( 'NONE',  ( 2.267534764145236803, 6.115564135048844108, 4.037922524061999141 ) ) ;
#35020 = CARTESIAN_POINT ( 'NONE',  ( -0.9351853929029012580, 116.6346273530297850, -0.2267945756083741271 ) ) ;
#35021 = CARTESIAN_POINT ( 'NONE',  ( -58.15941753978571427, 0.7172703587996687169, -1.185050425798436891 ) ) ;
#35022 = ORIENTED_EDGE ( 'NONE', *, *, #14689, .F. ) ;
#35023 = CARTESIAN_POINT ( 'NONE',  ( 0.3633380039124867733, 121.5961256765096152, 0.3912981906941394028 ) ) ;
#35024 = CYLINDRICAL_SURFACE ( 'NONE', #17508, 2.539999999999996483 ) ;
#35025 = CARTESIAN_POINT ( 'NONE',  ( -7.187319939301759497, 155.7895407640516510, 1.441898956427383416 ) ) ;
#35026 = CARTESIAN_POINT ( 'NONE',  ( -25.97603047661466036, 74.27059221564131519, 1.523999999999992694 ) ) ;
#35027 = ADVANCED_FACE ( 'NONE', ( #3350 ), #25619, .F. ) ;
#35028 = CARTESIAN_POINT ( 'NONE',  ( 18.37903003504434807, 149.1773161885088825, -1.724610598947830198 ) ) ;
#35029 = CARTESIAN_POINT ( 'NONE',  ( -20.82642717637633822, 141.6159226613069109, -2.307662509007912366 ) ) ;
#35030 = CARTESIAN_POINT ( 'NONE',  ( -54.34142964503966056, 9.837102586603037935, -3.694930414371515148 ) ) ;
#35031 = ADVANCED_FACE ( 'NONE', ( #6964, #585 ), #25497, .F. ) ;
#35032 = CARTESIAN_POINT ( 'NONE',  ( 15.71237885704634607, 143.6801599334541208, -0.6671153439278898478 ) ) ;
#35033 = ORIENTED_EDGE ( 'NONE', *, *, #19302, .T. ) ;
#35034 = CARTESIAN_POINT ( 'NONE',  ( 0.01023306027084651924, 119.5380416804913324, -0.5121041807152041381 ) ) ;
#35035 = CARTESIAN_POINT ( 'NONE',  ( 2.255636784185061749, -15.37476536804864580, 5.049411959999403621 ) ) ;
#35036 = CARTESIAN_POINT ( 'NONE',  ( -4.109772556805769028, 118.2429491485453070, -0.3484531805798580795 ) ) ;
#35037 = CARTESIAN_POINT ( 'NONE',  ( -57.97566020452313040, 1.918554019021911916, -1.632400077439718933 ) ) ;
#35038 = CARTESIAN_POINT ( 'NONE',  ( -4.810414185812548205, 117.7356259150898126, 0.8787797982406257979 ) ) ;
#35039 = CARTESIAN_POINT ( 'NONE',  ( 17.71853448156623756, 146.5573550606970628, 2.243325415855148108 ) ) ;
#35040 = CARTESIAN_POINT ( 'NONE',  ( 1.957912617769093311, 35.96399040732271857, -0.5992445403938203574 ) ) ;
#35041 = CARTESIAN_POINT ( 'NONE',  ( 8.428375251627102216, -1.854023157342211903, -0.5381045032988257537 ) ) ;
#35042 = CARTESIAN_POINT ( 'NONE',  ( 9.187421481788707212, 153.8854248570426080, 0.5770480568347668981 ) ) ;
#35043 = DIRECTION ( 'NONE',  ( -0.8572391118119488951, -0.5149185422762135866, 0.000000000000000000 ) ) ;
#35044 = CARTESIAN_POINT ( 'NONE',  ( -41.93982928939168175, 22.21638423992008882, -1.241790202385191666 ) ) ;
#35045 = CARTESIAN_POINT ( 'NONE',  ( -0.7553559341985174314, 117.3993842960191785, 1.459876094933623802 ) ) ;
#35046 = CARTESIAN_POINT ( 'NONE',  ( -58.37241122568488549, -0.2962816677227753104, 0.2416009568453807987 ) ) ;
#35047 = CARTESIAN_POINT ( 'NONE',  ( -54.13734601216691544, 8.984237177898892313, 3.668503415557924363 ) ) ;
#35048 = CARTESIAN_POINT ( 'NONE',  ( -7.967423902850907957, 121.6429398603349057, -1.120207190759914484 ) ) ;
#35049 = LINE ( 'NONE', #35253, #24912 ) ;
#35050 = CARTESIAN_POINT ( 'NONE',  ( -52.46220839783629941, 13.84563717269405458, 4.010158452165631715 ) ) ;
#35051 = EDGE_CURVE ( 'NONE', #40169, #19837, #31058, .T. ) ;
#35052 = CARTESIAN_POINT ( 'NONE',  ( -23.20816695139205166, 149.6253602407241488, -0.3098579641399930029 ) ) ;
#35053 = VERTEX_POINT ( 'NONE', #30160 ) ;
#35054 = CARTESIAN_POINT ( 'NONE',  ( -47.99025707952956310, 21.67807857130912907, -3.596429695783045055 ) ) ;
#35055 = CARTESIAN_POINT ( 'NONE',  ( 6.952013292454969573, 121.9314134082488437, -0.04296861412470696223 ) ) ;
#35056 = CARTESIAN_POINT ( 'NONE',  ( -7.903630729594187443, 122.1168884809555237, 0.5501188935067273800 ) ) ;
#35057 = VERTEX_POINT ( 'NONE', #14168 ) ;
#35058 = CARTESIAN_POINT ( 'NONE',  ( 1.574585577260951386, 115.7027553830524482, -1.670870382018978528 ) ) ;
#35059 = CARTESIAN_POINT ( 'NONE',  ( -15.77366026095721274, 146.5725700477668170, -0.4436318658883099397 ) ) ;
#35060 = CARTESIAN_POINT ( 'NONE',  ( 5.114911232981273592, -13.88689734646693452, 3.682185042294812582 ) ) ;
#35061 = CARTESIAN_POINT ( 'NONE',  ( -2.147481372520724463, 117.7847241295267651, 0.6070331404035438361 ) ) ;
#35062 = CARTESIAN_POINT ( 'NONE',  ( -6.617255152258657249E-14, 94.83546620154572793, -2.708805023911452991E-18 ) ) ;
#35063 = CARTESIAN_POINT ( 'NONE',  ( 23.24214586660302118, 149.3282167461061931, 0.7955682979737043192 ) ) ;
#35064 = CARTESIAN_POINT ( 'NONE',  ( 7.768456763902117146, 154.6794480478109222, 0.2667523075916575781 ) ) ;
#35065 = CARTESIAN_POINT ( 'NONE',  ( 16.60960244842765476, 9.026346327358513832, 0.000000000000000000 ) ) ;
#35066 = CARTESIAN_POINT ( 'NONE',  ( 0.9616503885695291132, 8.288457568681202758, 0.1719041247055087540 ) ) ;
#35067 = CARTESIAN_POINT ( 'NONE',  ( -16.27462974253343830, 121.4070763266325628, -0.3766275504196340829 ) ) ;
#35068 = FACE_OUTER_BOUND ( 'NONE', #27385, .T. ) ;
#35069 = DIRECTION ( 'NONE',  ( 0.3582377630123915746, -0.9336303900108851028, 3.445432962228667069E-16 ) ) ;
#35070 = EDGE_LOOP ( 'NONE', ( #25765, #3947, #3916, #7699 ) ) ;
#35071 = AXIS2_PLACEMENT_3D ( 'NONE', #9106, #9872, #10084 ) ;
#35072 = CARTESIAN_POINT ( 'NONE',  ( 2.308497710762058563, 116.4336050630576267, 0.3288393404144274168 ) ) ;
#35073 = CARTESIAN_POINT ( 'NONE',  ( -0.09930934064637705894, -13.04092083763876175, -4.623607705436294957 ) ) ;
#35074 = CARTESIAN_POINT ( 'NONE',  ( 13.86838617718231603, 121.5005676099359846, 1.565740997395133949 ) ) ;
#35075 = CARTESIAN_POINT ( 'NONE',  ( 19.50252919055201062, 149.6234262069624492, -1.702160239338572412 ) ) ;
#35076 = CARTESIAN_POINT ( 'NONE',  ( -8.331803066987694351, 8.350395779143005015, -1.420432620954584113 ) ) ;
#35077 = CARTESIAN_POINT ( 'NONE',  ( -5.842876937034696461, 117.7475948868982698, -0.8887855332765350891 ) ) ;
#35078 = CARTESIAN_POINT ( 'NONE',  ( 4.881271996281774328, 117.7524462357942099, -0.7532070458226111098 ) ) ;
#35079 = EDGE_CURVE ( 'NONE', #32861, #31901, #41957, .T. ) ;
#35080 = CARTESIAN_POINT ( 'NONE',  ( 6.487065698694983062, 120.6500652548963899, 0.3947850323583861898 ) ) ;
#35081 = CARTESIAN_POINT ( 'NONE',  ( -10.41298992473528351, 153.0987333575537548, -0.09138415589099052605 ) ) ;
#35082 = CARTESIAN_POINT ( 'NONE',  ( -18.91839881582121663, 147.5601278813269914, -2.482394308196493871 ) ) ;
#35083 = CARTESIAN_POINT ( 'NONE',  ( 5.457633994894312224, -14.92472868577397804, 3.194711634204877804 ) ) ;
#35084 = CARTESIAN_POINT ( 'NONE',  ( 4.726645377701876427, 118.5931160184169073, 1.020514608935862544 ) ) ;
#35085 = CARTESIAN_POINT ( 'NONE',  ( -3.969859667707119844, 117.3993838098210745, -1.318277526388289989 ) ) ;
#35086 = EDGE_LOOP ( 'NONE', ( #2684, #6200 ) ) ;
#35087 = CARTESIAN_POINT ( 'NONE',  ( 4.201129436297820874, 119.4047208153655646, 0.9741049750989215772 ) ) ;
#35088 = DIRECTION ( 'NONE',  ( -1.000000000000000000, 1.288607544181256449E-16, 0.000000000000000000 ) ) ;
#35089 = CARTESIAN_POINT ( 'NONE',  ( -46.49070643682303938, 25.85670910372597220, -1.524000000000008459 ) ) ;
#35090 = CARTESIAN_POINT ( 'NONE',  ( -0.7414234751012540592, 107.0594419416054848, 4.828671665556864667 ) ) ;
#35091 = CARTESIAN_POINT ( 'NONE',  ( 3.771486885279011325, -13.69470344665998773, -7.544622693077620568 ) ) ;
#35092 = CARTESIAN_POINT ( 'NONE',  ( 2.711066548582543145, 120.7183352303693340, 0.3631387678457471124 ) ) ;
#35093 = AXIS2_PLACEMENT_3D ( 'NONE', #18053, #18258, #18470 ) ;
#35094 = CARTESIAN_POINT ( 'NONE',  ( 14.85158921512553931, 156.1223461918646933, -0.5575614454322267433 ) ) ;
#35095 = CARTESIAN_POINT ( 'NONE',  ( 5.224225368397438451, 56.51500000000548596, -5.327462281792795906 ) ) ;
#35096 = CARTESIAN_POINT ( 'NONE',  ( -58.02663847586048718, 0.4467317610142895745, 0.8231150145234874538 ) ) ;
#35097 = CARTESIAN_POINT ( 'NONE',  ( -8.796272724451718261, 117.6874569103046184, -0.2327601223367594674 ) ) ;
#35098 = CARTESIAN_POINT ( 'NONE',  ( -5.511275327877945607, 57.14999999999955804, 5.111309965977547165 ) ) ;
#35099 = CARTESIAN_POINT ( 'NONE',  ( -23.21373371908098449, 149.6306211361744829, -0.4638656453230912136 ) ) ;
#35100 = ORIENTED_EDGE ( 'NONE', *, *, #2127, .F. ) ;
#35101 = CARTESIAN_POINT ( 'NONE',  ( -4.581230805175637855, 119.7013507852435907, -0.9162263165478330418 ) ) ;
#35102 = CARTESIAN_POINT ( 'NONE',  ( 4.678875543802746506, 116.0444662015457737, -3.608683038041131663 ) ) ;
#35103 = CARTESIAN_POINT ( 'NONE',  ( -9.301285777573651714, 153.8845013697122965, -0.8210809464416256587 ) ) ;
#35104 = CARTESIAN_POINT ( 'NONE',  ( -29.22735587826698378, 60.46978361828900006, 1.523999999999993804 ) ) ;
#35105 = CARTESIAN_POINT ( 'NONE',  ( 20.69846590548368681, 152.5542719854981044, 0.4384689201006755077 ) ) ;
#35106 = ORIENTED_EDGE ( 'NONE', *, *, #8389, .F. ) ;
#35107 = CARTESIAN_POINT ( 'NONE',  ( 1.616848224653315569, 9.589005055319924864, -4.350374724214612243 ) ) ;
#35108 = CARTESIAN_POINT ( 'NONE',  ( -5.224344491509385513, 105.1221337964526015, 1.129052726857179945 ) ) ;
#35109 = CARTESIAN_POINT ( 'NONE',  ( -4.829025010785088057, 117.4037175691626800, 1.009844946545902733 ) ) ;
#35110 = FACE_OUTER_BOUND ( 'NONE', #19327, .T. ) ;
#35111 = DIRECTION ( 'NONE',  ( -0.9998004120163608288, 0.000000000000000000, -0.01997839162482749342 ) ) ;
#35112 = CARTESIAN_POINT ( 'NONE',  ( 6.069967830169430201, 121.4313382071030958, 0.2855943879085542370 ) ) ;
#35113 = CARTESIAN_POINT ( 'NONE',  ( -4.282102574861781363, 27.11529131024228434, -1.748715980913516876 ) ) ;
#35114 = CARTESIAN_POINT ( 'NONE',  ( 5.389281185859638335, 158.9671755112622122, 1.064713296837521916 ) ) ;
#35115 = CARTESIAN_POINT ( 'NONE',  ( -1.034730806123546287, 104.6144662015457243, -4.723492537174234229 ) ) ;
#35117 = CARTESIAN_POINT ( 'NONE',  ( 21.60128648486314518, 148.1022500232506616, -1.385191265705788100 ) ) ;
#35116 = CARTESIAN_POINT ( 'NONE',  ( 5.450291846086562586, 56.51499999999996504, 4.451173312910839286 ) ) ;
#35118 = CARTESIAN_POINT ( 'NONE',  ( -2.469877670440149942, 119.5064228623769225, 0.6390414609872484553 ) ) ;
#35119 = CARTESIAN_POINT ( 'NONE',  ( -4.621355134897683570, 27.56591289442953041, -0.4301045952606497025 ) ) ;
#35120 = CARTESIAN_POINT ( 'NONE',  ( -17.89857548597121095, 125.1504969321615164, -1.218861057454596830 ) ) ;
#35121 = VERTEX_POINT ( 'NONE', #20341 ) ;
#35122 = CARTESIAN_POINT ( 'NONE',  ( -56.88731995051696089, 2.378615435641953546, 0.1283520312635431648 ) ) ;
#35123 = CIRCLE ( 'NONE', #10628, 14.73199999999999577 ) ;
#35124 = CARTESIAN_POINT ( 'NONE',  ( -9.945677869405052718, 124.8826105625126530, 0.2455395418728892332 ) ) ;
#35125 = CARTESIAN_POINT ( 'NONE',  ( 5.381753124113789255, -12.14417964010665330, 1.193960664996519094 ) ) ;
#35126 = CARTESIAN_POINT ( 'NONE',  ( 1.906664127224543481, 156.5995568990359175, -1.114948187579593020 ) ) ;
#35127 = DIRECTION ( 'NONE',  ( 5.188838149069472160E-16, -1.699382548006136559E-16, -1.000000000000000000 ) ) ;
#35128 = CARTESIAN_POINT ( 'NONE',  ( -4.783699877145565438, 117.7666882364519836, -1.035143524469993359 ) ) ;
#35129 = CARTESIAN_POINT ( 'NONE',  ( 11.03183784343224616, 128.0124916018596650, 0.2204423744267035301 ) ) ;
#35130 = VERTEX_POINT ( 'NONE', #1209 ) ;
#35131 = CARTESIAN_POINT ( 'NONE',  ( 20.09316625820287427, 147.7236477000422497, 2.507557202006583719 ) ) ;
#35132 = CARTESIAN_POINT ( 'NONE',  ( 15.19943428492308080, 148.1072807477730748, 0.3037208696559882681 ) ) ;
#35133 = CARTESIAN_POINT ( 'NONE',  ( 6.057513928997551922, 83.56599999999998829, -1.904999999999999805 ) ) ;
#35134 = CARTESIAN_POINT ( 'NONE',  ( 4.997288873896878592, 117.4043910709748104, -0.8233982764724142589 ) ) ;
#35135 = CARTESIAN_POINT ( 'NONE',  ( 23.34493312772026030, 146.7646281656787437, 0.007662864037405868467 ) ) ;
#35136 =( BOUNDED_CURVE ( )  B_SPLINE_CURVE ( 3, ( #17258, #30249, #36873, #24062 ),
 .UNSPECIFIED., .F., .T. ) 
 B_SPLINE_CURVE_WITH_KNOTS ( ( 4, 4 ),
 ( 0.1539179638657816873, 0.4253411113690419576 ),
 .UNSPECIFIED. ) 
 CURVE ( )  GEOMETRIC_REPRESENTATION_ITEM ( )  RATIONAL_B_SPLINE_CURVE ( ( 0.5738540613416667213, 0.4347666551225499165, 0.4921339822382616580, 0.7459560426888020013 ) ) 
 REPRESENTATION_ITEM ( '' )  );
#35137 = DIRECTION ( 'NONE',  ( -5.188838149069471174E-16, 1.699382548006136313E-16, 1.000000000000000000 ) ) ;
#35138 = CARTESIAN_POINT ( 'NONE',  ( 4.812253369269448022, 118.7629491485453030, 0.6571626099536693744 ) ) ;
#35139 = CARTESIAN_POINT ( 'NONE',  ( -47.53841933257975683, 25.36174273411122115, 0.2940116119274914785 ) ) ;
#35140 = CARTESIAN_POINT ( 'NONE',  ( 1.740236503711715343, -15.12629859915687369, 5.675635612196994195 ) ) ;
#35141 = CARTESIAN_POINT ( 'NONE',  ( -48.16508968810062896, 19.01313136326716347, 5.219744232931976313 ) ) ;
#35142 = CARTESIAN_POINT ( 'NONE',  ( -41.28107547821692691, 23.22158991241129300, -1.523999999999999355 ) ) ;
#35143 = CARTESIAN_POINT ( 'NONE',  ( -4.592121672059828796, 118.0813459264795284, 0.5392318162658802372 ) ) ;
#35144 = VECTOR ( 'NONE', #525, 1000.000000000000000 ) ;
#35145 = ORIENTED_EDGE ( 'NONE', *, *, #26636, .T. ) ;
#35146 = ORIENTED_EDGE ( 'NONE', *, *, #13693, .F. ) ;
#35147 = DIRECTION ( 'NONE',  ( 5.188838149069472160E-16, -1.699382548006136559E-16, -1.000000000000000000 ) ) ;
#35148 = CARTESIAN_POINT ( 'NONE',  ( 3.610368082249861388, 118.7437733682415058, -0.7930644133314173061 ) ) ;
#35149 = CARTESIAN_POINT ( 'NONE',  ( -6.110436517261230271, 121.4157903421748301, -0.3281350463252857286 ) ) ;
#35150 = CARTESIAN_POINT ( 'NONE',  ( 4.682529446909616588, 117.8402053342184530, 1.032763938081705524 ) ) ;
#35151 = CARTESIAN_POINT ( 'NONE',  ( 2.994295736468014280, -14.77441112906794984, 3.968895097548184037 ) ) ;
#35152 = CARTESIAN_POINT ( 'NONE',  ( -0.5861964566937933885, 120.4790399057546182, -0.3305540093316994277 ) ) ;
#35153 = CARTESIAN_POINT ( 'NONE',  ( 3.501419995798253915, -2.955197114699519734, 3.043391175950921568 ) ) ;
#35154 = DIRECTION ( 'NONE',  ( 5.188838149069471174E-16, -1.699382548006136313E-16, -1.000000000000000000 ) ) ;
#35155 = CARTESIAN_POINT ( 'NONE',  ( -5.664977208693890987, 57.14999999999997016, -5.033228321271210781 ) ) ;
#35156 = CARTESIAN_POINT ( 'NONE',  ( 4.753511127315582563, 115.8251506319059843, -1.256829922054841786 ) ) ;
#35157 = CARTESIAN_POINT ( 'NONE',  ( -11.37357585002895810, 124.5424752485109963, -1.510439678823544352 ) ) ;
#35158 = DIRECTION ( 'NONE',  ( 0.9849462604886048966, 0.000000000000000000, -0.1728608224830406881 ) ) ;
#35159 = CARTESIAN_POINT ( 'NONE',  ( -2.876480734726157173, 115.7032361094657631, 1.566537190358891163 ) ) ;
#35160 = CARTESIAN_POINT ( 'NONE',  ( 1.111903444298625754, 15.29877551736591812, 4.515507465039587665 ) ) ;
#35162 = ORIENTED_EDGE ( 'NONE', *, *, #34542, .T. ) ;
#35161 = CARTESIAN_POINT ( 'NONE',  ( 1.889792677999337700, 116.7132768022172797, 0.3078404110637331659 ) ) ;
#35163 = CARTESIAN_POINT ( 'NONE',  ( 3.348477637022819309, 104.6144662015456959, -3.488726040212962953 ) ) ;
#35164 = CARTESIAN_POINT ( 'NONE',  ( 3.716361853963529249, -15.42594482578084403, 2.788391211141477921 ) ) ;
#35165 = CARTESIAN_POINT ( 'NONE',  ( -17.18700207657779089, 151.3967157021085654, 1.745027292404997654 ) ) ;
#35166 = CARTESIAN_POINT ( 'NONE',  ( 0.3309596775784566236, 20.21946177965197222, 0.9160044982600296093 ) ) ;
#35167 = CIRCLE ( 'NONE', #13207, 0.5080000000000000071 ) ;
#35168 = CARTESIAN_POINT ( 'NONE',  ( -0.5393284202071846334, 5.265691905141185458, 0.8139242273222374591 ) ) ;
#35169 = EDGE_CURVE ( 'NONE', #16326, #30173, #7182, .T. ) ;
#35170 = ORIENTED_EDGE ( 'NONE', *, *, #34303, .F. ) ;
#35171 = VERTEX_POINT ( 'NONE', #7802 ) ;
#35172 = DIRECTION ( 'NONE',  ( -0.9876665170007969952, 0.1565721916417935344, -5.390917751951444915E-16 ) ) ;
#35173 = CARTESIAN_POINT ( 'NONE',  ( 3.099458292114882774, 117.0475107411037641, 1.222660999933594672 ) ) ;
#35174 = CARTESIAN_POINT ( 'NONE',  ( -12.34427413551901509, 128.4316967252784991, 0.8534409008407578545 ) ) ;
#35175 = CARTESIAN_POINT ( 'NONE',  ( -12.85860202769644545, 133.7716054015561156, -0.2569454702854386263 ) ) ;
#35176 = CARTESIAN_POINT ( 'NONE',  ( 2.509002420848308823, -14.82469439542799527, 5.007744185041904217 ) ) ;
#35177 = CARTESIAN_POINT ( 'NONE',  ( 17.67426794430086900, 144.4767212251450417, -1.594784396078125166 ) ) ;
#35178 = AXIS2_PLACEMENT_3D ( 'NONE', #41051, #5484, #34243 ) ;
#35179 = CARTESIAN_POINT ( 'NONE',  ( -13.83536887852640440, 154.2684476645699760, -2.291766773079779274 ) ) ;
#35180 = DIRECTION ( 'NONE',  ( 5.188838149069472160E-16, -1.699382548006136559E-16, -1.000000000000000000 ) ) ;
#35181 = CARTESIAN_POINT ( 'NONE',  ( 7.948490438896031129, 121.7395506310447217, 1.077254804507452812 ) ) ;
#35182 = CARTESIAN_POINT ( 'NONE',  ( -2.330492536650612845, 35.40100364009314404, 2.787243435389755941 ) ) ;
#35183 = CARTESIAN_POINT ( 'NONE',  ( 5.918555687551686262, 121.5031286879076902, -0.05579296748036344233 ) ) ;
#35184 = CIRCLE ( 'NONE', #5273, 0.2539999999999997260 ) ;
#35185 = ORIENTED_EDGE ( 'NONE', *, *, #35461, .F. ) ;
#35186 = CARTESIAN_POINT ( 'NONE',  ( -1.615419284005069400, 106.5834530906608819, -5.022566955870309435 ) ) ;
#35187 = FACE_OUTER_BOUND ( 'NONE', #5552, .T. ) ;
#35188 = DIRECTION ( 'NONE',  ( -0.9998004120163608288, 0.000000000000000000, -0.01997839162482749342 ) ) ;
#35189 = DIRECTION ( 'NONE',  ( -5.188838149069471174E-16, 1.699382548006136313E-16, 1.000000000000000000 ) ) ;
#35190 = CARTESIAN_POINT ( 'NONE',  ( -8.047487967707532164, 27.33737370333709649, -2.486188741727015206 ) ) ;
#35191 = CARTESIAN_POINT ( 'NONE',  ( 14.71707226966671023, 150.5114039713088516, 1.846696807168831223 ) ) ;
#35192 = DIRECTION ( 'NONE',  ( -5.206863593109713661E-17, 1.000000000000000000, -1.077750396879097183E-30 ) ) ;
#35193 = CARTESIAN_POINT ( 'NONE',  ( 23.29076518286600361, 149.3500807853454546, 0.3882996703880465250 ) ) ;
#35194 = CARTESIAN_POINT ( 'NONE',  ( -2.658992269297188127, 107.2388417251876547, 4.621886736208384860 ) ) ;
#35195 = AXIS2_PLACEMENT_3D ( 'NONE', #16070, #42092, #38258 ) ;
#35196 = CARTESIAN_POINT ( 'NONE',  ( 18.32410244842765934, 0.6349999999999984546, 2.244055341071511024E-15 ) ) ;
#35197 = CARTESIAN_POINT ( 'NONE',  ( 4.599243292695290641, 121.2024757821991159, 0.09190382657876450256 ) ) ;
#35198 = EDGE_CURVE ( 'NONE', #41686, #33162, #28323, .T. ) ;
#35199 = CARTESIAN_POINT ( 'NONE',  ( 13.73566407960799296, 122.1113760975138263, 1.718532046871276808 ) ) ;
#35200 = CARTESIAN_POINT ( 'NONE',  ( -8.389224625646681588, -1.175411479303250628, -1.011143247504549869 ) ) ;
#35201 = CARTESIAN_POINT ( 'NONE',  ( -5.484251324081573564, 117.2052654494406454, -0.8040846112588506678 ) ) ;
#35202 = CARTESIAN_POINT ( 'NONE',  ( -0.3796903751653987746, 122.8649044353670803, -0.2268226101886973156 ) ) ;
#35203 = DIRECTION ( 'NONE',  ( -1.000000000000000000, -5.463695987328526437E-16, -0.000000000000000000 ) ) ;
#35204 = CARTESIAN_POINT ( 'NONE',  ( 3.524443185806435341, 109.1382852134488104, -3.813950880701249879 ) ) ;
#35205 = CARTESIAN_POINT ( 'NONE',  ( -4.050807963365556930, 30.95410787014092335, -2.229501126309402448 ) ) ;
#35206 = CARTESIAN_POINT ( 'NONE',  ( 1.086073555308449290, 117.3993836040883423, 1.476595440916665058 ) ) ;
#35207 = DIRECTION ( 'NONE',  ( -0.000000000000000000, -0.000000000000000000, -1.000000000000000000 ) ) ;
#35208 = CARTESIAN_POINT ( 'NONE',  ( 1.979956398862833922, -15.17398463081316784, 5.317940750273952411 ) ) ;
#35209 = CARTESIAN_POINT ( 'NONE',  ( 0.7907195946116533092, 120.5370721568272216, -0.4966358104988963240 ) ) ;
#35210 = CARTESIAN_POINT ( 'NONE',  ( -22.56840570087990017, 150.3096427868838987, 0.3971349512683052252 ) ) ;
#35211 = CIRCLE ( 'NONE', #1231, 0.5080000000000002292 ) ;
#35212 = ORIENTED_EDGE ( 'NONE', *, *, #31584, .T. ) ;
#35213 = CARTESIAN_POINT ( 'NONE',  ( 5.475330206976798841, 53.58606249999999704, 5.107412922131463695 ) ) ;
#35214 = ORIENTED_EDGE ( 'NONE', *, *, #29131, .T. ) ;
#35215 = FACE_OUTER_BOUND ( 'NONE', #6285, .T. ) ;
#35216 = CARTESIAN_POINT ( 'NONE',  ( 4.496247062743834455, -15.66418688627994804, 3.575535799018406014 ) ) ;
#35217 = CARTESIAN_POINT ( 'NONE',  ( -9.147047865982875336, 157.1510513929294177, 1.627767162235162601 ) ) ;
#35218 = CARTESIAN_POINT ( 'NONE',  ( 21.39260515875391633, 150.3702682424204511, -1.149856210633945608 ) ) ;
#35219 = CARTESIAN_POINT ( 'NONE',  ( -4.399545650080316506, 2.442302885307133131, -1.471791394725967095 ) ) ;
#35220 = ADVANCED_FACE ( 'NONE', ( #1001 ), #26281, .T. ) ;
#35221 = CARTESIAN_POINT ( 'NONE',  ( -56.87050244847664260, 3.471200836702969195, -2.275408806060764455 ) ) ;
#35222 = EDGE_LOOP ( 'NONE', ( #11923, #20470 ) ) ;
#35223 = CARTESIAN_POINT ( 'NONE',  ( -58.34429324193579447, -0.2380942604817831709, -0.1989150628791391540 ) ) ;
#35224 = CARTESIAN_POINT ( 'NONE',  ( -0.1065646865916383690, 105.8844662015456919, 5.332932678536313809 ) ) ;
#35225 = CARTESIAN_POINT ( 'NONE',  ( -5.946078212987909062, 28.42590610009757413, 0.3016625663984517924 ) ) ;
#35226 = CARTESIAN_POINT ( 'NONE',  ( -10.84039127762421195, 123.6843197456346672, 1.011594478071749847 ) ) ;
#35227 = DIRECTION ( 'NONE',  ( -5.188838149069472160E-16, 1.699382548006136559E-16, 1.000000000000000000 ) ) ;
#35228 = CARTESIAN_POINT ( 'NONE',  ( 16.64003893621117314, 151.1890201267100906, -1.733044620493700672 ) ) ;
#35229 = CARTESIAN_POINT ( 'NONE',  ( -20.86684145051977879, 149.6610172957225586, -2.296701127946504606 ) ) ;
#35230 = CARTESIAN_POINT ( 'NONE',  ( -51.02479983779974049, 14.46739584830851477, -4.600955224801065668 ) ) ;
#35231 = CIRCLE ( 'NONE', #2580, 0.5080000000000002292 ) ;
#35232 = ADVANCED_FACE ( 'NONE', ( #36564 ), #5233, .T. ) ;
#35233 = CARTESIAN_POINT ( 'NONE',  ( 9.814938192569819364, 124.1138826855306831, -0.4990610963926596644 ) ) ;
#35234 = VERTEX_POINT ( 'NONE', #33366 ) ;
#35235 = CARTESIAN_POINT ( 'NONE',  ( -17.88897823598650305, 147.4621342421176848, -2.293131556269223381 ) ) ;
#35236 = CARTESIAN_POINT ( 'NONE',  ( 3.520778385322295811, -15.02221911624387829, 1.583774285062736986 ) ) ;
#35237 = CARTESIAN_POINT ( 'NONE',  ( -4.223640366674269231, 118.2238299684479301, -0.4905063076566205105 ) ) ;
#35238 = FACE_OUTER_BOUND ( 'NONE', #13850, .T. ) ;
#35239 = CARTESIAN_POINT ( 'NONE',  ( -4.981834297919686350, 117.5302800348309518, 0.7676192988303492948 ) ) ;
#35240 = CARTESIAN_POINT ( 'NONE',  ( 13.61432229890752943, 152.4534842159446271, 2.088615715084950697 ) ) ;
#35241 = DIRECTION ( 'NONE',  ( 6.146657985744592735E-16, 3.905054717696927382E-31, 1.000000000000000000 ) ) ;
#35242 =( REPRESENTATION_RELATIONSHIP ('NONE','NONE', #30767, #26424 ) REPRESENTATION_RELATIONSHIP_WITH_TRANSFORMATION ( #24049 )SHAPE_REPRESENTATION_RELATIONSHIP( ) );
#35243 = CARTESIAN_POINT ( 'NONE',  ( 2.163044864548389956, 28.58015952483584954, -4.087059112497700042 ) ) ;
#35244 = CARTESIAN_POINT ( 'NONE',  ( 10.47888833811890130, 153.0637448873655728, 0.6176438153593470926 ) ) ;
#35245 = CARTESIAN_POINT ( 'NONE',  ( -25.56614996202194590, 73.65611136973726047, -1.270000000000005569 ) ) ;
#35246 = EDGE_CURVE ( 'NONE', #11189, #5419, #40186, .T. ) ;
#35247 = ADVANCED_FACE ( 'NONE', ( #4198 ), #468, .T. ) ;
#35248 = CARTESIAN_POINT ( 'NONE',  ( -47.79679003974130325, 17.22715854250130718, -2.282645788202384729 ) ) ;
#35249 = CARTESIAN_POINT ( 'NONE',  ( -5.591535794131392123, 65.03215273817657760, -1.523999999999993804 ) ) ;
#35250 = DIRECTION ( 'NONE',  ( 0.3582377630123915746, -0.9336303900108851028, 3.445432962228667069E-16 ) ) ;
#35251 = CARTESIAN_POINT ( 'NONE',  ( -52.89566005465288612, 11.31963682940546789, 4.132128454502246306 ) ) ;
#35252 = EDGE_CURVE ( 'NONE', #19839, #35748, #26761, .T. ) ;
#35253 = CARTESIAN_POINT ( 'NONE',  ( -16.60960244842765832, 17.14499999999999957, 0.000000000000000000 ) ) ;
#35254 = CARTESIAN_POINT ( 'NONE',  ( -57.93941708942283952, 2.052042089854988483, 1.628789306319508023 ) ) ;
#35255 = CARTESIAN_POINT ( 'NONE',  ( -23.32076472591260341, 148.8446908248229477, -0.1342014517686427599 ) ) ;
#35256 = ORIENTED_EDGE ( 'NONE', *, *, #26310, .F. ) ;
#35257 = CARTESIAN_POINT ( 'NONE',  ( -52.70911355518960306, 14.14937146821753444, -3.349573991549135155 ) ) ;
#35258 = CARTESIAN_POINT ( 'NONE',  ( 7.835216397241184794, 122.4239432713123961, -0.2785063474257676863 ) ) ;
#35259 = CARTESIAN_POINT ( 'NONE',  ( 4.901676919075300454, 117.4083593258483660, -0.9680037761291583331 ) ) ;
#35260 = ORIENTED_EDGE ( 'NONE', *, *, #40233, .F. ) ;
#35261 = CARTESIAN_POINT ( 'NONE',  ( 2.452571136908805016, 115.7029491485453718, -1.604305510785485556 ) ) ;
#35262 = CARTESIAN_POINT ( 'NONE',  ( -7.564868681920799531, 122.4257779438054285, -0.2276018551017723324 ) ) ;
#35263 = CARTESIAN_POINT ( 'NONE',  ( 2.291753010757021869, -15.38865404460348962, 5.937071240476925027 ) ) ;
#35264 = CARTESIAN_POINT ( 'NONE',  ( -21.59954917983698408, 148.3057046726078170, 1.384394358321686669 ) ) ;
#35265 = DIRECTION ( 'NONE',  ( -0.3582377630123966261, 0.9336303900108832154, 0.000000000000000000 ) ) ;
#35266 = CARTESIAN_POINT ( 'NONE',  ( 16.80483327138715310, 155.2524275687165982, 0.6336504121414452406 ) ) ;
#35267 = CARTESIAN_POINT ( 'NONE',  ( 4.201361461317214996, 155.8715872134815754, 0.1795330533319696442 ) ) ;
#35268 = CARTESIAN_POINT ( 'NONE',  ( -17.68910244842765778, 3.329298639413090771E-15, 2.205172805198582110E-15 ) ) ;
#35269 = CARTESIAN_POINT ( 'NONE',  ( -0.4793318477812648082, 11.74037758575859058, -0.8492235504747065455 ) ) ;
#35270 = CARTESIAN_POINT ( 'NONE',  ( -4.732570698819529298, 116.7698466342620378, -0.1749797587976939517 ) ) ;
#35271 = DIRECTION ( 'NONE',  ( -0.8745520943968243532, 0.4849315768086547296, -5.361993529360573944E-16 ) ) ;
#35272 = CARTESIAN_POINT ( 'NONE',  ( 1.650612623617701257E-15, 17.14499999999999957, 0.000000000000000000 ) ) ;
#35273 = VERTEX_POINT ( 'NONE', #7589 ) ;
#35274 = CARTESIAN_POINT ( 'NONE',  ( -8.638482609000943668, 118.5544449468999915, 0.7679241716596895140 ) ) ;
#35275 = EDGE_LOOP ( 'NONE', ( #40067, #16665, #8018, #9641 ) ) ;
#35276 = CARTESIAN_POINT ( 'NONE',  ( -58.32396914991895898, -0.1951167097209117463, -0.2694727270791387186 ) ) ;
#35277 = CARTESIAN_POINT ( 'NONE',  ( 7.226289359486251840, 158.3006260280594404, 1.552328403643545185 ) ) ;
#35278 = CARTESIAN_POINT ( 'NONE',  ( 20.02944843481977699, 148.6304843473828043, -1.700276915703843983 ) ) ;
#35279 = CARTESIAN_POINT ( 'NONE',  ( -7.798946185677827714, 9.198776092563324625, 3.184250115244839030 ) ) ;
#35280 = CARTESIAN_POINT ( 'NONE',  ( -5.309498559578598176, 158.9031408473208273, -1.190161311236993091 ) ) ;
#35281 = CARTESIAN_POINT ( 'NONE',  ( 4.797843704864214409, 117.8843084929736733, -0.6937365112328826022 ) ) ;
#35282 = DIRECTION ( 'NONE',  ( 0.9998004120163609398, 0.000000000000000000, 0.01997839162482749689 ) ) ;
#35283 = CARTESIAN_POINT ( 'NONE',  ( -3.740144479511176900, 121.0798372856833538, -0.007817740762067527244 ) ) ;
#35284 = CARTESIAN_POINT ( 'NONE',  ( -11.41083474541188814, 122.2847249198043471, -1.726555165334429764 ) ) ;
#35285 = CARTESIAN_POINT ( 'NONE',  ( 5.792286216032899837, -14.99041835605292938, 0.9165201714659111376 ) ) ;
#35286 = DIRECTION ( 'NONE',  ( -0.8745520943968235761, 0.4849315768086558398, -5.691349986800547879E-16 ) ) ;
#35287 = CARTESIAN_POINT ( 'NONE',  ( -47.43570116002440784, 20.37060963802031566, -5.342502768866047802 ) ) ;
#35288 = ADVANCED_FACE ( 'NONE', ( #10771 ), #3127, .F. ) ;
#35289 = ORIENTED_EDGE ( 'NONE', *, *, #3821, .T. ) ;
#35290 = CARTESIAN_POINT ( 'NONE',  ( 11.57159210561016138, 122.7176759045101022, 1.727280539041415874 ) ) ;
#35291 = DIRECTION ( 'NONE',  ( -1.011795553208986377E-16, -1.000000000000000000, 0.000000000000000000 ) ) ;
#35292 = AXIS2_PLACEMENT_3D ( 'NONE', #14741, #27951, #27743 ) ;
#35293 = LINE ( 'NONE', #26115, #10300 ) ;
#35294 = CARTESIAN_POINT ( 'NONE',  ( -0.1065646865916159980, 105.8844662015457061, 5.332932678536314697 ) ) ;
#35295 = CARTESIAN_POINT ( 'NONE',  ( 8.391146056172745560, -15.30543149186461527, -0.4349570568239987667 ) ) ;
#35296 = CARTESIAN_POINT ( 'NONE',  ( 15.91132205781015863, 147.3275361421020193, 1.167720536598261027 ) ) ;
#35297 = CARTESIAN_POINT ( 'NONE',  ( 3.862028650946859543, 117.0275016673472663, -0.3788463918649357387 ) ) ;
#35298 = DIRECTION ( 'NONE',  ( -0.5810519254489896479, -0.8138664877804110409, 0.000000000000000000 ) ) ;
#35299 = DIRECTION ( 'NONE',  ( 0.000000000000000000, 0.000000000000000000, -1.000000000000000000 ) ) ;
#35300 = ADVANCED_FACE ( 'NONE', ( #37799 ), #26998, .T. ) ;
#35301 = CARTESIAN_POINT ( 'NONE',  ( -15.97340373827834270, 121.0409387471171101, -0.3191866212789524204 ) ) ;
#35302 = ADVANCED_FACE ( 'NONE', ( #18831 ), #5869, .F. ) ;
#35303 = ORIENTED_EDGE ( 'NONE', *, *, #14638, .T. ) ;
#35304 = CARTESIAN_POINT ( 'NONE',  ( 8.266801410408760376, 120.3999688492377942, -1.106489660158431754 ) ) ;
#35305 = LINE ( 'NONE', #39342, #27166 ) ;
#35306 = CARTESIAN_POINT ( 'NONE',  ( -9.627236290563509158, 124.2480737032941533, -0.7173579674491835645 ) ) ;
#35307 = CARTESIAN_POINT ( 'NONE',  ( -30.15642192025596202, 71.36377005712995469, -1.524000000000007571 ) ) ;
#35308 = CARTESIAN_POINT ( 'NONE',  ( 18.63389541082830192, 154.1203422869290023, 0.3962720605433153187 ) ) ;
#35309 = ORIENTED_EDGE ( 'NONE', *, *, #39114, .T. ) ;
#35310 = CARTESIAN_POINT ( 'NONE',  ( -3.789191232057584902, 13.46218022696137773, 2.646434746401360893 ) ) ;
#35311 = CARTESIAN_POINT ( 'NONE',  ( -29.20122892408340221, 63.96733531827668173, 1.269999999999945617 ) ) ;
#35312 = CARTESIAN_POINT ( 'NONE',  ( -4.854821967544332928, 117.4083635672741366, 0.9981540133063625531 ) ) ;
#35313 = CARTESIAN_POINT ( 'NONE',  ( -6.654617103318593247E-14, 104.6144662015457243, 1.534725424433578570E-31 ) ) ;
#35314 = CARTESIAN_POINT ( 'NONE',  ( -4.468667403750213651, 27.88063884994054220, 0.5133561255362272258 ) ) ;
#35315 = CARTESIAN_POINT ( 'NONE',  ( 7.950778463150458997, 121.7274446046149450, 1.085857570170044140 ) ) ;
#35316 = VECTOR ( 'NONE', #41444, 1000.000000000000000 ) ;
#35317 = CARTESIAN_POINT ( 'NONE',  ( 4.453423564604278795, 13.74662854910535792, -1.294644163995742225 ) ) ;
#35318 = CARTESIAN_POINT ( 'NONE',  ( 3.066799924081360817, 159.2904672602661549, 0.9578552656232323104 ) ) ;
#35319 = DIRECTION ( 'NONE',  ( 0.8572391118119481179, 0.5149185422762151410, 0.000000000000000000 ) ) ;
#35321 = CARTESIAN_POINT ( 'NONE',  ( 4.917623111643079525, 158.3981005702974016, -1.478962986009813463 ) ) ;
#35320 = CARTESIAN_POINT ( 'NONE',  ( 2.768561164044480272, -13.57843041371762460, 0.3119852368007841603 ) ) ;
#35322 = CARTESIAN_POINT ( 'NONE',  ( -15.17272240541839778, 131.2890697635526465, 1.517944203131903258 ) ) ;
#35323 = CARTESIAN_POINT ( 'NONE',  ( 3.087053954869741101, 14.59627045569285286, -3.440871586639639990 ) ) ;
#35324 = CARTESIAN_POINT ( 'NONE',  ( -9.626009506019258311, 118.2334930433176652, -0.7695227696168690512 ) ) ;
#35325 = EDGE_LOOP ( 'NONE', ( #19623, #14220, #6040, #12963 ) ) ;
#35326 = CARTESIAN_POINT ( 'NONE',  ( -14.81827458270682918, 148.8567844064068026, 0.2884810962875102858 ) ) ;
#35327 = CARTESIAN_POINT ( 'NONE',  ( 5.879588643049518559, -13.10657381646278274, 1.873965859954596969 ) ) ;
#35328 = LINE ( 'NONE', #38734, #34994 ) ;
#35329 = CARTESIAN_POINT ( 'NONE',  ( -4.574660132527480272, 118.0200319299317329, -0.8704685883761965615 ) ) ;
#35330 = CARTESIAN_POINT ( 'NONE',  ( 15.26332761227456913, 148.0152273645666980, 0.2540164781927349846 ) ) ;
#35331 = VERTEX_POINT ( 'NONE', #40594 ) ;
#35332 = CARTESIAN_POINT ( 'NONE',  ( 19.80203545474858018, 147.6055923437354238, 2.520003004638577515 ) ) ;
#35333 = DIRECTION ( 'NONE',  ( -0.01731298258488003436, 0.9998501190848634312, 0.000000000000000000 ) ) ;
#35334 = DIRECTION ( 'NONE',  ( -0.3582377630123966261, 0.9336303900108832154, 0.000000000000000000 ) ) ;
#35335 = CARTESIAN_POINT ( 'NONE',  ( -22.38075128446561379, 150.2360280492587776, 0.6257272249761320904 ) ) ;
#35336 = CARTESIAN_POINT ( 'NONE',  ( 0.001367086239699496575, 156.3041635968983485, -0.06841458569046195148 ) ) ;
#35337 = CARTESIAN_POINT ( 'NONE',  ( 0.003550357975883500824, 159.5989787797044812, -0.1776744311461873616 ) ) ;
#35338 = EDGE_CURVE ( 'NONE', #24583, #22830, #15428, .T. ) ;
#35339 = VECTOR ( 'NONE', #32578, 1000.000000000000227 ) ;
#35340 = DIRECTION ( 'NONE',  ( -0.8745520943968347893, 0.4849315768086356893, -6.829619984160681712E-16 ) ) ;
#35341 = CARTESIAN_POINT ( 'NONE',  ( -46.86252819529217106, 25.53111598637714152, 1.612082337883730787 ) ) ;
#35342 = CARTESIAN_POINT ( 'NONE',  ( -46.79514595010191158, 25.77136020477034606, 0.9526608576032333797 ) ) ;
#35344 = EDGE_CURVE ( 'NONE', #18324, #32986, #9326, .T. ) ;
#35343 = CARTESIAN_POINT ( 'NONE',  ( 2.143789057001533660, -15.08792135351709440, 5.678686283222974751 ) ) ;
#35345 = CARTESIAN_POINT ( 'NONE',  ( -44.13308345971568514, 24.21351174012166396, 1.567149544246648762 ) ) ;
#35346 = CARTESIAN_POINT ( 'NONE',  ( -6.111026219684664010E-14, 94.83546620154572793, 9.844778328339670704E-17 ) ) ;
#35347 = CARTESIAN_POINT ( 'NONE',  ( -4.569938957122442247, 118.0881010721686692, 0.5676615755902681970 ) ) ;
#35348 = VERTEX_POINT ( 'NONE', #27793 ) ;
#35349 = DIRECTION ( 'NONE',  ( -0.8745520943968245753, 0.4849315768086539524, -5.691349986800526185E-16 ) ) ;
#35350 = CARTESIAN_POINT ( 'NONE',  ( -8.367821637836184934, 119.6608375418318673, -1.423109165391701847 ) ) ;
#35351 = CARTESIAN_POINT ( 'NONE',  ( -0.1497278248017035740, 105.8844662015457629, -5.338012126719978490 ) ) ;
#35352 = CARTESIAN_POINT ( 'NONE',  ( 4.680159262726512281, 117.9616872321280994, 0.8793832278182402984 ) ) ;
#35353 = CARTESIAN_POINT ( 'NONE',  ( -11.17805678602830355, 77.92260723867444483, 1.269999999999999352 ) ) ;
#35354 = CARTESIAN_POINT ( 'NONE',  ( -2.668671847104423289, 120.5579296053302727, -0.4429723278990744251 ) ) ;
#35355 = CARTESIAN_POINT ( 'NONE',  ( -4.337156242749934165, 111.8943083658765119, 2.742175979689941645 ) ) ;
#35356 = DIRECTION ( 'NONE',  ( 0.9454731675810374991, -0.3256999990547734258, 7.420046207093947887E-15 ) ) ;
#35357 = CARTESIAN_POINT ( 'NONE',  ( 6.321818188556049378, 120.0717973201777511, -0.2011600071967685199 ) ) ;
#35358 = CARTESIAN_POINT ( 'NONE',  ( -9.120583164541152144, 155.0058477609193801, -1.824713877226967762 ) ) ;
#35359 = LINE ( 'NONE', #22128, #19404 ) ;
#35360 = CARTESIAN_POINT ( 'NONE',  ( 19.68500000000000227, 71.11999999999999034, 1.904999999999987592 ) ) ;
#35361 = CARTESIAN_POINT ( 'NONE',  ( -2.370637312493784954, 115.7028718339712867, 1.611039750900896017 ) ) ;
#35362 = CARTESIAN_POINT ( 'NONE',  ( -4.319812470756069445, 11.96289413176386951, -1.686699837767231536 ) ) ;
#35364 = ORIENTED_EDGE ( 'NONE', *, *, #35977, .F. ) ;
#35363 = CARTESIAN_POINT ( 'NONE',  ( 20.48075987368136452, 152.5656283612522657, 1.113479615819600532 ) ) ;
#35365 = CARTESIAN_POINT ( 'NONE',  ( 4.895972490868764737, 105.1214892841856994, -2.148021949592362478 ) ) ;
#35366 = CARTESIAN_POINT ( 'NONE',  ( 3.518836906362542205, -15.09289160254213868, 2.194652486238897193 ) ) ;
#35367 = CARTESIAN_POINT ( 'NONE',  ( -19.53500017296066815, 148.0998626603252148, 1.736236475658778255 ) ) ;
#35368 = CARTESIAN_POINT ( 'NONE',  ( 0.9269407327955943021, 12.00036500698010578, 0.3089908296573128932 ) ) ;
#35369 = CARTESIAN_POINT ( 'NONE',  ( -0.2812775050834619428, 1.806455656379289287, -0.9370761103187740249 ) ) ;
#35370 = ORIENTED_EDGE ( 'NONE', *, *, #29256, .F. ) ;
#35371 = CIRCLE ( 'NONE', #12899, 13.46199999999999619 ) ;
#35372 = ORIENTED_EDGE ( 'NONE', *, *, #11028, .T. ) ;
#35373 = CYLINDRICAL_SURFACE ( 'NONE', #28300, 0.6350000000000014522 ) ;
#35374 = CARTESIAN_POINT ( 'NONE',  ( 6.983605877934210504, 124.9344662015457175, 0.1395490654994195612 ) ) ;
#35375 =( NAMED_UNIT ( * ) PLANE_ANGLE_UNIT ( ) SI_UNIT ( $, .RADIAN. ) );
#35376 = CARTESIAN_POINT ( 'NONE',  ( -16.33963436279749715, 146.4745453488731357, 0.7896242330311489255 ) ) ;
#35377 = CARTESIAN_POINT ( 'NONE',  ( -7.784012322544769269, 122.6313477034873074, -0.1555430911242075831 ) ) ;
#35378 = CARTESIAN_POINT ( 'NONE',  ( 2.626143189074743756, -14.75305764222682647, 4.894789397842846945 ) ) ;
#35379 = CARTESIAN_POINT ( 'NONE',  ( 11.26369337785505742, 123.4744472594011739, -1.139971239082960830 ) ) ;
#35380 = CARTESIAN_POINT ( 'NONE',  ( -19.55492868859755617, 148.8045834396381508, -2.507096624874099344 ) ) ;
#35381 = CARTESIAN_POINT ( 'NONE',  ( 10.92199999999999704, 56.51500000000000057, -4.381499999999999950 ) ) ;
#35382 = CARTESIAN_POINT ( 'NONE',  ( 7.889029732257585081, 122.0453901860990982, 0.9157283810244409850 ) ) ;
#35383 = CARTESIAN_POINT ( 'NONE',  ( -6.004997167832389238, 30.93677315496120173, -0.5383843454024033193 ) ) ;
#35384 = CARTESIAN_POINT ( 'NONE',  ( 15.72482880707709541, 147.2451778420852406, -0.1375710997406973113 ) ) ;
#35385 = ORIENTED_EDGE ( 'NONE', *, *, #15894, .F. ) ;
#35386 = CARTESIAN_POINT ( 'NONE',  ( -24.32950799593924884, 77.42192949967211746, -1.524000000000005572 ) ) ;
#35387 =( BOUNDED_SURFACE ( )  B_SPLINE_SURFACE ( 3, 2, ( 
 ( #12516, #8694, #25082 ),
 ( #2103, #41502, #15067 ),
 ( #2739, #18894, #24875 ),
 ( #34474, #5511, #5308 ),
 ( #6139, #41710, #25507 ),
 ( #5727, #37665, #18682 ),
 ( #11886, #12308, #41078 ),
 ( #21870, #31690, #28701 ),
 ( #12094, #38507, #2532 ),
 ( #18469, #25296, #32112 ),
 ( #9323, #28067, #34896 ),
 ( #15494, #22286, #35311 ),
 ( #2942, #19103, #15906 ),
 ( #31474, #38299, #41921 ),
 ( #24656, #2318, #15279 ),
 ( #28283, #9119, #41290 ) ),
 .UNSPECIFIED., .F., .F., .T. ) 
 B_SPLINE_SURFACE_WITH_KNOTS ( ( 4, 2, 2, 2, 2, 2, 2, 4 ),
 ( 3, 3 ),
 ( 1.734723475976807094E-18, 0.005291144675846519603, 0.007936717013769778103, 0.01058228935169303747, 0.01322786168961629684, 0.01455064785857792739, 0.01587343402753955621, 0.02116457870338607494 ),
 ( 0.000000000000000000, 1.000000000000000000 ),
 .UNSPECIFIED. ) 
 GEOMETRIC_REPRESENTATION_ITEM ( )  RATIONAL_B_SPLINE_SURFACE ( (
 ( 1.000000000000000000, 0.7071067811865519026, 1.000000000000000000),
 ( 1.000000000000000000, 0.7071067811865519026, 1.000000000000000000),
 ( 1.000000000000000000, 0.7071067811865469066, 1.000000000000000000),
 ( 1.000000000000000000, 0.7071067811865469066, 1.000000000000000000),
 ( 1.000000000000000000, 0.7071067811865472397, 1.000000000000000000),
 ( 1.000000000000000000, 0.7071067811865472397, 1.000000000000000000),
 ( 1.000000000000000000, 0.7071067811865491270, 1.000000000000000000),
 ( 1.000000000000000000, 0.7071067811865491270, 1.000000000000000000),
 ( 1.000000000000000000, 0.7071067811865464625, 1.000000000000000000),
 ( 1.000000000000000000, 0.7071067811865464625, 1.000000000000000000),
 ( 1.000000000000000000, 0.7071067811865472397, 1.000000000000000000),
 ( 1.000000000000000000, 0.7071067811865472397, 1.000000000000000000),
 ( 1.000000000000000000, 0.7071067811865472397, 1.000000000000000000),
 ( 1.000000000000000000, 0.7071067811865472397, 1.000000000000000000),
 ( 1.000000000000000000, 0.7071067811865423547, 1.000000000000000000),
 ( 1.000000000000000000, 0.7071067811865423547, 1.000000000000000000) ) ) 
 REPRESENTATION_ITEM ( '' )  SURFACE ( )  );
#35388 = DIRECTION ( 'NONE',  ( -0.9575201071113178530, 0.2883665106726683858, -8.537024980200786319E-16 ) ) ;
#35389 = CARTESIAN_POINT ( 'NONE',  ( 5.007985129730328389, 117.3993836135851438, -0.7769739375564292949 ) ) ;
#35390 = CARTESIAN_POINT ( 'NONE',  ( -3.263082884110522386, 19.99377609092593389, 7.766292582686701529 ) ) ;
#35391 = CARTESIAN_POINT ( 'NONE',  ( 9.075659781537913418, 123.1184971541203055, 0.9241268708344096972 ) ) ;
#35392 = CARTESIAN_POINT ( 'NONE',  ( -17.14500000000466784, 71.11999999999886768, -1.270000000000000684 ) ) ;
#35393 = CARTESIAN_POINT ( 'NONE',  ( 1.421877081889598937, 159.6054662015457666, 0.01472409299311864921 ) ) ;
#35394 = CARTESIAN_POINT ( 'NONE',  ( -5.252825482164497295, 116.2501875120488393, 0.9643948023431454519 ) ) ;
#35395 = AXIS2_PLACEMENT_3D ( 'NONE', #4086, #23854, #13646 ) ;
#35396 = CARTESIAN_POINT ( 'NONE',  ( -8.761523658392190939, 74.56051954986229191, -1.523999999999997135 ) ) ;
#35397 = CARTESIAN_POINT ( 'NONE',  ( 1.104432469574216480, -9.427232690354344413, -4.492858291722996888 ) ) ;
#35398 = CARTESIAN_POINT ( 'NONE',  ( 0.3395595041295305649, 35.30132035414327873, -0.2191788681752833978 ) ) ;
#35399 = ADVANCED_FACE ( 'NONE', ( #1826 ), #31411, .F. ) ;
#35400 = CARTESIAN_POINT ( 'NONE',  ( 20.91256836843372469, 148.0559997909317644, 2.401931445155506939 ) ) ;
#35401 = CARTESIAN_POINT ( 'NONE',  ( -5.887876509958990923, -9.367530720701759961, 6.022233148990229878 ) ) ;
#35402 = CARTESIAN_POINT ( 'NONE',  ( 2.179975478414604595, 116.7279437644658344, -0.4024351897304699333 ) ) ;
#35403 = CARTESIAN_POINT ( 'NONE',  ( -0.3920235582992755985, 123.4679809879532542, -0.1617017839830490744 ) ) ;
#35404 = DIRECTION ( 'NONE',  ( -0.8745520943968235761, 0.4849315768086558398, -5.691349986800547879E-16 ) ) ;
#35405 = DIRECTION ( 'NONE',  ( -0.7770581983690729722, 0.6294287539884164673, -8.537024980200685740E-16 ) ) ;
#35406 = CARTESIAN_POINT ( 'NONE',  ( -3.571940676414631533, 104.6144662015457243, 3.260099874920956431 ) ) ;
#35407 = CARTESIAN_POINT ( 'NONE',  ( -2.923568588381722844, 13.88697512809157786, 3.594856661414283394 ) ) ;
#35408 = LINE ( 'NONE', #6439, #17776 ) ;
#35409 = DIRECTION ( 'NONE',  ( 0.01997839162482760444, 1.040247600000950455E-18, -0.9998004120163609398 ) ) ;
#35410 = CARTESIAN_POINT ( 'NONE',  ( 2.932272473696061255, -14.72556872895393276, 4.151486945341092749 ) ) ;
#35411 = CARTESIAN_POINT ( 'NONE',  ( 2.738288815228959727, 121.4869043954268903, -0.2316524989510642119 ) ) ;
#35412 = CARTESIAN_POINT ( 'NONE',  ( -18.36446446646858632, 154.1536317137893661, 0.4323159980074339215 ) ) ;
#35413 = B_SPLINE_CURVE_WITH_KNOTS ( 'NONE', 3,
 ( #26580, #20802, #7216, #823, #35089, #5912 ),
 .UNSPECIFIED., .F., .F.,
 ( 4, 2, 4 ),
 ( -6.000000000029375625E-08, 0.0006551176351295480036, 0.001310295270259096301 ),
 .UNSPECIFIED. ) ;
#35414 = ORIENTED_EDGE ( 'NONE', *, *, #34455, .T. ) ;
#35415 = CARTESIAN_POINT ( 'NONE',  ( 5.871452009091292723, 88.73331249999999670, 5.016499999999999737 ) ) ;
#35416 = VERTEX_POINT ( 'NONE', #8203 ) ;
#35417 = DIRECTION ( 'NONE',  ( -0.1728608224830406603, 0.000000000000000000, -0.9849462604886047856 ) ) ;
#35418 = CARTESIAN_POINT ( 'NONE',  ( 2.988498945533646367, -15.63929389023541106, 5.494461050752756925 ) ) ;
#35419 = CARTESIAN_POINT ( 'NONE',  ( -20.18403667007074986, 149.6821479856479300, 1.616815787834456231 ) ) ;
#35420 = CIRCLE ( 'NONE', #17043, 0.7620000000000000107 ) ;
#35421 = CARTESIAN_POINT ( 'NONE',  ( 6.877630800715452963, 117.9658002137636856, -0.6876290806823442958 ) ) ;
#35422 = CARTESIAN_POINT ( 'NONE',  ( -4.274281473441157608, 3.541781053574249327, 1.790774723582081451 ) ) ;
#35423 = CARTESIAN_POINT ( 'NONE',  ( -58.28145228256266108, 0.4519758043100738365, -1.031447170180650463 ) ) ;
#35424 = ORIENTED_EDGE ( 'NONE', *, *, #19029, .T. ) ;
#35425 = CARTESIAN_POINT ( 'NONE',  ( -56.57399730107058389, 3.557946380840157463, -2.108622681941325183 ) ) ;
#35426 = CARTESIAN_POINT ( 'NONE',  ( -0.04081796247070307998, 114.7739974199301969, 2.042697753608746059 ) ) ;
#35427 =( NAMED_UNIT ( * ) SI_UNIT ( $, .STERADIAN. ) SOLID_ANGLE_UNIT ( ) );
#35428 = PRODUCT_DEFINITION_SHAPE ( 'NONE', 'NONE',  #42162 ) ;
#35429 = CARTESIAN_POINT ( 'NONE',  ( -17.27635908418611166, 147.1820577694790018, 1.364000445115660876 ) ) ;
#35430 = DIRECTION ( 'NONE',  ( -6.353134868986659519E-16, 1.000000000000000000, 0.000000000000000000 ) ) ;
#35431 = CARTESIAN_POINT ( 'NONE',  ( 1.325863631979435686, 119.1766673560425858, -0.6173222594915835915 ) ) ;
#35432 = CIRCLE ( 'NONE', #1414, 0.2540000000000062208 ) ;
#35433 = CARTESIAN_POINT ( 'NONE',  ( -4.854614700615708323, 158.3981005702974016, -1.674235554132198489 ) ) ;
#35434 = CARTESIAN_POINT ( 'NONE',  ( -57.64973313486724038, 1.352533784701764885, -1.499908592384923134 ) ) ;
#35435 = EDGE_LOOP ( 'NONE', ( #7592, #23667, #1345, #29127 ) ) ;
#35436 = CARTESIAN_POINT ( 'NONE',  ( 4.558037855495248536, 118.1057855763819049, -0.4916461251602846638 ) ) ;
#35437 = CARTESIAN_POINT ( 'NONE',  ( 0.6112472438485718751, 120.6441756478195089, -0.2446543754660636949 ) ) ;
#35438 = ORIENTED_EDGE ( 'NONE', *, *, #22158, .T. ) ;
#35439 = CARTESIAN_POINT ( 'NONE',  ( 0.02874415600660452930, 157.0795416643300939, -1.438475106415293858 ) ) ;
#35440 = CARTESIAN_POINT ( 'NONE',  ( 3.487342509456591522, -15.13654059619573644, 2.575171134517089566 ) ) ;
#35441 = CARTESIAN_POINT ( 'NONE',  ( -4.105768389763392534, 118.2429491485453070, -0.3526141341681313102 ) ) ;
#35442 = CARTESIAN_POINT ( 'NONE',  ( -53.01551111795199489, 8.729259440421063942, -9.365303671399559428E-15 ) ) ;
#35443 = EDGE_CURVE ( 'NONE', #9633, #3167, #2252, .T. ) ;
#35444 = CARTESIAN_POINT ( 'NONE',  ( -4.920305038941537923, 117.6396262227241749, 0.8278391774136714121 ) ) ;
#35445 = CARTESIAN_POINT ( 'NONE',  ( 17.41367791652938735, 147.5992144370567871, 2.159268082968858415 ) ) ;
#35446 = CARTESIAN_POINT ( 'NONE',  ( -1.915954025944994433E-14, 30.83083951148100255, 1.904999999999999805 ) ) ;
#35447 = VECTOR ( 'NONE', #18427, 1000.000000000000227 ) ;
#35448 = EDGE_CURVE ( 'NONE', #39680, #31017, #25149, .T. ) ;
#35449 = CARTESIAN_POINT ( 'NONE',  ( 7.253464168720983096, -10.72948646729439659, -4.330533999219945862 ) ) ;
#35450 = CARTESIAN_POINT ( 'NONE',  ( 4.547323659248075245, 121.1438296405421937, 0.2486498796252668564 ) ) ;
#35451 = CARTESIAN_POINT ( 'NONE',  ( -52.30895062419047292, 13.66434875625866674, -4.401212925246500873 ) ) ;
#35453 = ORIENTED_EDGE ( 'NONE', *, *, #38191, .T. ) ;
#35452 = CARTESIAN_POINT ( 'NONE',  ( -47.83226487260633775, 16.75079348177631999, -1.615774049669077117 ) ) ;
#35454 = CARTESIAN_POINT ( 'NONE',  ( -0.6048974376704769895, 117.3993834314756128, 1.469641059425755403 ) ) ;
#35455 = VECTOR ( 'NONE', #3871, 1000.000000000000114 ) ;
#35456 = CARTESIAN_POINT ( 'NONE',  ( -46.67889021447872011, 26.03274747417083645, -1.323595506759009499 ) ) ;
#35457 = CARTESIAN_POINT ( 'NONE',  ( -52.53650722201378898, 11.97175513791591328, 4.250412846625016172 ) ) ;
#35458 = CARTESIAN_POINT ( 'NONE',  ( -8.362805289807246467, 119.6845456798349829, -1.431079265360458486 ) ) ;
#35459 = DIRECTION ( 'NONE',  ( -0.8745520943968243532, 0.4849315768086547296, -6.829619984160642269E-16 ) ) ;
#35460 = CARTESIAN_POINT ( 'NONE',  ( -54.99893072520226411, 10.64604335972153137, 1.135982259999769983 ) ) ;
#35461 = EDGE_CURVE ( 'NONE', #35130, #18118, #25852, .T. ) ;
#35462 = CARTESIAN_POINT ( 'NONE',  ( -0.003073183581813956986, 116.5806198863164838, 0.1537946732117061455 ) ) ;
#35463 = VERTEX_POINT ( 'NONE', #12866 ) ;
#35464 = CARTESIAN_POINT ( 'NONE',  ( -52.14602366315243387, 18.74265329119796064, -0.7451446608535732263 ) ) ;
#35465 = CARTESIAN_POINT ( 'NONE',  ( 6.919917455521427563, 121.8373941398667313, -0.2187690460202940113 ) ) ;
#35466 = ORIENTED_EDGE ( 'NONE', *, *, #23472, .F. ) ;
#35467 = CARTESIAN_POINT ( 'NONE',  ( 0.7849178055945060795, 115.7029491485453718, -1.726834944265495553 ) ) ;
#35468 = CARTESIAN_POINT ( 'NONE',  ( -5.289698609640079319, 121.3432423864224177, -0.1753557357117458970 ) ) ;
#35469 = CARTESIAN_POINT ( 'NONE',  ( 3.228727248129140026, -15.23899909574484646, 5.612614099740361517 ) ) ;
#35470 = CARTESIAN_POINT ( 'NONE',  ( -21.16640241758172181, 149.7512365312068709, 1.384406599442889352 ) ) ;
#35471 = LINE ( 'NONE', #32273, #2312 ) ;
#35472 = CARTESIAN_POINT ( 'NONE',  ( 10.77008264951268046, 157.9328640892066460, 0.4716003899658740006 ) ) ;
#35473 = CARTESIAN_POINT ( 'NONE',  ( 8.009213594383991719, 122.8488802212246611, 0.2424541544307477758 ) ) ;
#35474 = DIRECTION ( 'NONE',  ( -6.146657985744592735E-16, 3.905054717696928257E-31, 1.000000000000000000 ) ) ;
#35475 = CARTESIAN_POINT ( 'NONE',  ( 0.8487236205744517203, 17.35912690172634143, 0.4866769997786373203 ) ) ;
#35476 = CARTESIAN_POINT ( 'NONE',  ( -15.17534484293440578, 156.1124880001465556, -0.4370721430752772529 ) ) ;
#35477 = CARTESIAN_POINT ( 'NONE',  ( -13.46199999999999264, 13.84300000000000530, 1.648619521012166368E-15 ) ) ;
#35478 = DIRECTION ( 'NONE',  ( 0.000000000000000000, 1.000000000000000000, 0.000000000000000000 ) ) ;
#35479 = EDGE_LOOP ( 'NONE', ( #62, #17164, #13899, #37912, #29566, #32921, #28324, #5448 ) ) ;
#35480 = CARTESIAN_POINT ( 'NONE',  ( 2.603427674266608260, 116.9065387239081701, 0.5777963497691434025 ) ) ;
#35482 = ADVANCED_FACE ( 'NONE', ( #32261 ), #22216, .T. ) ;
#35481 = ORIENTED_EDGE ( 'NONE', *, *, #30451, .F. ) ;
#35483 = CYLINDRICAL_SURFACE ( 'NONE', #26589, 0.2540000000000045000 ) ;
#35484 = CARTESIAN_POINT ( 'NONE',  ( 1.224709079186512728, 159.1407128229522527, 1.247756218451904431 ) ) ;
#35485 = CARTESIAN_POINT ( 'NONE',  ( 13.23674331388971304, 122.5785676075921060, -1.297564987558605498 ) ) ;
#35486 = CARTESIAN_POINT ( 'NONE',  ( -1.555401355773622374, 10.72473834230686762, 8.302158768936594768 ) ) ;
#35487 = CARTESIAN_POINT ( 'NONE',  ( -9.950292893259929272, 157.6892375622926181, -1.550998551202242393 ) ) ;
#35488 = CARTESIAN_POINT ( 'NONE',  ( 4.633276512935547764, 117.9522311679255893, -0.7618818254156639602 ) ) ;
#35489 = AXIS2_PLACEMENT_3D ( 'NONE', #16025, #9645, #22612 ) ;
#35490 = CYLINDRICAL_SURFACE ( 'NONE', #15215, 0.2540000000000000036 ) ;
#35491 = ADVANCED_FACE ( 'NONE', ( #31836 ), #42070, .F. ) ;
#35492 = CARTESIAN_POINT ( 'NONE',  ( -11.06366964751665982, 128.0319838675845290, -0.1805508315534839758 ) ) ;
#35493 = CARTESIAN_POINT ( 'NONE',  ( -19.16322371038640071, 147.9830121424878939, -2.503561316673066361 ) ) ;
#35494 = CARTESIAN_POINT ( 'NONE',  ( 5.898825546834660649, -14.84738759216856785, 0.02597052417917125600 ) ) ;
#35495 = APPLICATION_CONTEXT ( 'automotive_design' ) ;
#35496 = AXIS2_PLACEMENT_3D ( 'NONE', #25901, #41688, #38488 ) ;
#35497 = DIRECTION ( 'NONE',  ( -5.188838149069472160E-16, 1.699382548006136559E-16, 1.000000000000000000 ) ) ;
#35498 = EDGE_CURVE ( 'NONE', #27023, #30178, #35184, .T. ) ;
#35499 = CARTESIAN_POINT ( 'NONE',  ( -42.72397600927682504, 22.83316142988638831, -1.683267422954632275 ) ) ;
#35500 = VERTEX_POINT ( 'NONE', #12660 ) ;
#35501 = CARTESIAN_POINT ( 'NONE',  ( 11.66906004923067641, 122.8035986606355152, 1.736571914056905142 ) ) ;
#35502 = CARTESIAN_POINT ( 'NONE',  ( -15.70103477329412911, 145.5797129992483292, -0.3137440411564564879 ) ) ;
#35503 = TOROIDAL_SURFACE ( 'NONE', #28679, 8.794749999999996959, 0.2540000000000000036 ) ;
#35504 = CARTESIAN_POINT ( 'NONE',  ( -6.631541954483209765E-14, 98.39146620154573952, -1.863789202389766375E-18 ) ) ;
#35505 = CARTESIAN_POINT ( 'NONE',  ( -4.585195778441760517, 124.9344662015457459, -0.09162312381275070083 ) ) ;
#35506 = CARTESIAN_POINT ( 'NONE',  ( 1.249529592346430240, 29.00528243095578063, -8.330927077797271707 ) ) ;
#35507 = CARTESIAN_POINT ( 'NONE',  ( 9.600854460372817201, 124.0356975489027036, 0.7994020406953790125 ) ) ;
#35508 = CARTESIAN_POINT ( 'NONE',  ( 14.24059674577810597, 120.4756499382577886, -0.4587616384891653465 ) ) ;
#35509 = CARTESIAN_POINT ( 'NONE',  ( 5.274109024393328404, 115.7029491485453150, -0.8140283081321303404 ) ) ;
#35510 = DIRECTION ( 'NONE',  ( -0.7770581983690878491, 0.6294287539883980376, -5.101669463485847584E-16 ) ) ;
#35511 = CIRCLE ( 'NONE', #4209, 14.09699999999999420 ) ;
#35512 = CARTESIAN_POINT ( 'NONE',  ( -2.736438259132304207, 116.5290148844309357, -0.04129949523434437580 ) ) ;
#35513 = VERTEX_POINT ( 'NONE', #19250 ) ;
#35514 = CARTESIAN_POINT ( 'NONE',  ( -6.482835885433019030, 120.3696088574302507, -1.155002112961008631 ) ) ;
#35515 = CARTESIAN_POINT ( 'NONE',  ( 2.851877909000272382, -15.42561672255453331, 5.733748130541576060 ) ) ;
#35516 = CARTESIAN_POINT ( 'NONE',  ( -10.72508252498929515, 126.1521286088116369, -0.7954780730053832016 ) ) ;
#35517 = CARTESIAN_POINT ( 'NONE',  ( 3.658150719587269784, -13.97641594243527408, 4.344832359604154703 ) ) ;
#35518 = CARTESIAN_POINT ( 'NONE',  ( 6.059261036834406866, 57.14999999999999858, -5.016499999999999737 ) ) ;
#35519 = CARTESIAN_POINT ( 'NONE',  ( 5.774842806153344554, 116.9337168780244696, 0.1296094601971085336 ) ) ;
#35520 = ORIENTED_EDGE ( 'NONE', *, *, #1445, .T. ) ;
#35521 = CARTESIAN_POINT ( 'NONE',  ( -4.319812470756069445, 11.96289413176387129, -1.686699837767231536 ) ) ;
#35522 = CARTESIAN_POINT ( 'NONE',  ( -15.97340373827834270, 121.0409387471171101, -0.3191866212789525314 ) ) ;
#35523 = CARTESIAN_POINT ( 'NONE',  ( -4.829078608027735697, 117.4024328994306501, 1.010041111858091423 ) ) ;
#35524 = CARTESIAN_POINT ( 'NONE',  ( 20.83467972660109524, 65.95194780259438971, 1.904999999999986704 ) ) ;
#35525 = EDGE_CURVE ( 'NONE', #11643, #19019, #3090, .T. ) ;
#35526 = CARTESIAN_POINT ( 'NONE',  ( -15.42835734045148577, 79.74558783746839197, -1.270000000000001350 ) ) ;
#35527 = CARTESIAN_POINT ( 'NONE',  ( -6.121275585599194713, 121.0364858238823729, 0.5305944776602569135 ) ) ;
#35528 = VECTOR ( 'NONE', #28169, 1000.000000000000227 ) ;
#35529 = CARTESIAN_POINT ( 'NONE',  ( 4.428293322310913993, 12.87204911218450398, 1.319288874004734158 ) ) ;
#35530 = EDGE_CURVE ( 'NONE', #12906, #1598, #3296, .T. ) ;
#35531 = CARTESIAN_POINT ( 'NONE',  ( 16.28621419528960601, 155.1963085991477271, 1.407434501154738671 ) ) ;
#35532 = CARTESIAN_POINT ( 'NONE',  ( -0.1058213901579529159, 105.9761915687834914, 5.295735085524055030 ) ) ;
#35534 = CARTESIAN_POINT ( 'NONE',  ( 4.057542840006381546, 118.1249481555716301, -0.7600096289331683685 ) ) ;
#35533 = CARTESIAN_POINT ( 'NONE',  ( -18.35410564743290607, 77.35382415001784295, 5.016499999999999737 ) ) ;
#35535 = CARTESIAN_POINT ( 'NONE',  ( 4.453423564604278795, 13.74662854910535792, -1.294644163995742225 ) ) ;
#35536 = CARTESIAN_POINT ( 'NONE',  ( -20.83375562662827107, 132.2939277659177151, -1.304325680028331602 ) ) ;
#35537 = ORIENTED_EDGE ( 'NONE', *, *, #14938, .F. ) ;
#35538 = CARTESIAN_POINT ( 'NONE',  ( -10.55375732331629557, 153.0603347025997323, 0.3251829154788382636 ) ) ;
#35539 = EDGE_CURVE ( 'NONE', #40413, #1790, #37904, .T. ) ;
#35540 = CARTESIAN_POINT ( 'NONE',  ( 4.290763117780162617, -14.65756668531598095, 4.875966813445055337 ) ) ;
#35541 = FACE_OUTER_BOUND ( 'NONE', #37601, .T. ) ;
#35542 = CIRCLE ( 'NONE', #19863, 0.5080000000000002292 ) ;
#35543 = ADVANCED_FACE ( 'NONE', ( #19665 ), #64, .T. ) ;
#35544 = CARTESIAN_POINT ( 'NONE',  ( -4.521871022792333328, 118.0719105266109636, -0.8080184913735506402 ) ) ;
#35545 = CARTESIAN_POINT ( 'NONE',  ( 15.78598348091615122, 146.2390805666957192, 0.2639793761055732602 ) ) ;
#35546 = ORIENTED_EDGE ( 'NONE', *, *, #24127, .T. ) ;
#35547 = CARTESIAN_POINT ( 'NONE',  ( 20.07331991451302500, 148.0303212619860744, 2.505472171123445779 ) ) ;
#35548 = CARTESIAN_POINT ( 'NONE',  ( 4.997525182441497016, 56.61525291752807476, 5.184946129310834984 ) ) ;
#35549 = LINE ( 'NONE', #39375, #20477 ) ;
#35550 = CARTESIAN_POINT ( 'NONE',  ( -16.32943869337488962, 155.1963085991477271, 0.7556961354993018132 ) ) ;
#35551 = CARTESIAN_POINT ( 'NONE',  ( 0.008148072696521003327, 156.3406798448389168, -0.4077628766201953359 ) ) ;
#35552 = CIRCLE ( 'NONE', #22598, 0.5080000000000002292 ) ;
#35553 = CARTESIAN_POINT ( 'NONE',  ( 15.95511372484715729, 121.3860667298135070, -0.1093881341078833114 ) ) ;
#35554 = CARTESIAN_POINT ( 'NONE',  ( 12.21488373879588885, 56.36092316367926713, -5.016500000000000625 ) ) ;
#35555 = CARTESIAN_POINT ( 'NONE',  ( -4.883848590450072358, 117.7607009110569862, 0.7127853619805604168 ) ) ;
#35556 = CARTESIAN_POINT ( 'NONE',  ( -47.24381373535820217, 25.63803778330989047, 0.2531820549803469045 ) ) ;
#35557 = CARTESIAN_POINT ( 'NONE',  ( -4.973714125165286326, 117.3984623533981022, -0.9750903916985453890 ) ) ;
#35558 = ORIENTED_EDGE ( 'NONE', *, *, #19352, .T. ) ;
#35559 = CARTESIAN_POINT ( 'NONE',  ( -43.87210973174860129, 22.05421410453335795, 2.454571855453426377 ) ) ;
#35560 = CARTESIAN_POINT ( 'NONE',  ( 2.676630639921374399, -14.70069741876437242, -0.3491543817257181659 ) ) ;
#35561 = CARTESIAN_POINT ( 'NONE',  ( -4.550470251402174426, 118.0718861047856336, 0.6267538730547278503 ) ) ;
#35562 = CARTESIAN_POINT ( 'NONE',  ( -5.583532163260057857, 78.91300747758680245, -5.082153855702578937 ) ) ;
#35563 = ORIENTED_EDGE ( 'NONE', *, *, #37098, .F. ) ;
#35564 = CARTESIAN_POINT ( 'NONE',  ( -0.1669248393526201191, 115.6909491485452435, -1.766429783486955341 ) ) ;
#35565 = CARTESIAN_POINT ( 'NONE',  ( 3.588165399132631883, 118.7223001924098895, -0.7939635985234113624 ) ) ;
#35566 = CARTESIAN_POINT ( 'NONE',  ( 0.1065646865915095692, 105.8844662015456919, -5.332932678536313809 ) ) ;
#35567 = CARTESIAN_POINT ( 'NONE',  ( 4.698333873473698574, 117.8441154341451238, 1.023705869601185814 ) ) ;
#35568 = CARTESIAN_POINT ( 'NONE',  ( 2.829627719599027369, -13.65247383265987757, 0.5238048331051645690 ) ) ;
#35569 = CARTESIAN_POINT ( 'NONE',  ( -7.827001302695666851, 121.9903164032602518, -0.9115841697347603079 ) ) ;
#35570 = AXIS2_PLACEMENT_3D ( 'NONE', #26178, #23758, #30167 ) ;
#35571 = CARTESIAN_POINT ( 'NONE',  ( -1.900728597266289288, 115.7024225971088214, -1.719626108874834580 ) ) ;
#35572 = CARTESIAN_POINT ( 'NONE',  ( -1.769971949791458332, 106.5487674150453046, 4.971549122525432907 ) ) ;
#35573 = CARTESIAN_POINT ( 'NONE',  ( -4.664314973664742681, 117.9253040426969790, -0.9621209789661747669 ) ) ;
#35574 = CARTESIAN_POINT ( 'NONE',  ( 4.828659834973804799, 112.7831754354443348, -2.372633244901563021 ) ) ;
#35575 = CARTESIAN_POINT ( 'NONE',  ( -10.50156301541560211, 123.3532649940754027, -1.413946074136436470 ) ) ;
#35576 = DIRECTION ( 'NONE',  ( 1.011795553208986377E-16, 1.000000000000000000, -0.000000000000000000 ) ) ;
#35577 = DIRECTION ( 'NONE',  ( 1.000000000000000000, 0.000000000000000000, -1.224646799147353947E-16 ) ) ;
#35578 = DIRECTION ( 'NONE',  ( -0.8745520943968243532, 0.4849315768086547296, -5.361993529360573944E-16 ) ) ;
#35579 = ORIENTED_EDGE ( 'NONE', *, *, #19339, .F. ) ;
#35580 = CARTESIAN_POINT ( 'NONE',  ( -4.595132424582489605, -6.828429371805166959, -0.5093739664528403877 ) ) ;
#35582 = ORIENTED_EDGE ( 'NONE', *, *, #27318, .F. ) ;
#35581 = CARTESIAN_POINT ( 'NONE',  ( 6.899218498548927769, 117.3903047926647787, 0.5887349169472964050 ) ) ;
#35583 = CARTESIAN_POINT ( 'NONE',  ( -30.01829664378881546, 60.43850663962886216, 1.523999999999993804 ) ) ;
#35584 = CARTESIAN_POINT ( 'NONE',  ( 2.617865251411226613, -15.35234423845867369, 4.678879665404411803 ) ) ;
#35585 = CARTESIAN_POINT ( 'NONE',  ( -18.75354316333454818, 144.8948545501563103, 1.742436930347202262 ) ) ;
#35586 = CARTESIAN_POINT ( 'NONE',  ( 0.5056692551311988693, 10.92592451650425112, 0.8332994872028685052 ) ) ;
#35587 = CIRCLE ( 'NONE', #13800, 0.5079999999999997851 ) ;
#35588 = CARTESIAN_POINT ( 'NONE',  ( -0.6378939814135665687, 2.446253604616882349, -0.7403349100440516084 ) ) ;
#35589 = ORIENTED_EDGE ( 'NONE', *, *, #28433, .F. ) ;
#35590 = ORIENTED_EDGE ( 'NONE', *, *, #25005, .F. ) ;
#35591 = CARTESIAN_POINT ( 'NONE',  ( -47.64484625134591766, 19.26749830283604936, 4.730721332201270890 ) ) ;
#35592 = CARTESIAN_POINT ( 'NONE',  ( 0.05023876518783839534, 106.0087397856094356, 5.285590276201098447 ) ) ;
#35593 = CARTESIAN_POINT ( 'NONE',  ( -16.45208226155739695, 147.1833543704171348, 0.9460114105336800971 ) ) ;
#35594 = CARTESIAN_POINT ( 'NONE',  ( 4.270589230953349968, -11.85684205577233818, 0.9542379244983925091 ) ) ;
#35595 = CARTESIAN_POINT ( 'NONE',  ( 16.80660261901782704, 149.5530097695598215, -1.582604632240843578 ) ) ;
#35596 = CARTESIAN_POINT ( 'NONE',  ( -3.228607480374549255, 118.8118204130220903, -0.9063605472083390291 ) ) ;
#35597 = DIRECTION ( 'NONE',  ( -0.8745520943968240202, 0.4849315768086553402, -6.829619984160650158E-16 ) ) ;
#35598 = EDGE_CURVE ( 'NONE', #28714, #4082, #39923, .T. ) ;
#35599 = CARTESIAN_POINT ( 'NONE',  ( 8.255953115981643720, 120.2039708552018880, 1.447841472369825189 ) ) ;
#35600 = CARTESIAN_POINT ( 'NONE',  ( -6.009810541787921068, 31.01725040276547674, -0.2975034299463961696 ) ) ;
#35601 = CARTESIAN_POINT ( 'NONE',  ( 9.238523569213899833, 124.0999252189730697, -0.04720364951821272304 ) ) ;
#35602 = ORIENTED_EDGE ( 'NONE', *, *, #24903, .F. ) ;
#35603 = FACE_OUTER_BOUND ( 'NONE', #27916, .T. ) ;
#35604 = COLOUR_RGB ( '', 0.31764706, 0.68627451, 0.89019608) ;
#35605 = FACE_OUTER_BOUND ( 'NONE', #29061, .T. ) ;
#35606 = CARTESIAN_POINT ( 'NONE',  ( -58.64342337384959336, -0.3142157529041483821, 0.3359497956446368394 ) ) ;
#35607 = CARTESIAN_POINT ( 'NONE',  ( 2.639528505629576305, 120.4390018212493914, 0.4929570044210890845 ) ) ;
#35608 = DIRECTION ( 'NONE',  ( -4.017660918040594346E-17, 1.000000000000000000, 2.376309959284834438E-19 ) ) ;
#35609 = CARTESIAN_POINT ( 'NONE',  ( 10.81400209053368755, 157.9177219752764358, 0.09677702710655973484 ) ) ;
#35610 = B_SPLINE_CURVE_WITH_KNOTS ( 'NONE', 3,
 ( #21586, #31192, #27791, #14579, #3826, #23374, #29996, #10609, #14788, #7224, #13810, #40800, #27999, #27584, #4035, #16996, #4247, #17209 ),
 .UNSPECIFIED., .F., .F.,
 ( 4, 2, 2, 2, 2, 2, 2, 2, 4 ),
 ( 0.000000000000000000, 0.0008271074710775116285, 0.001654214942155023257, 0.003308429884310066463, 0.004135537355387588175, 0.004962644826465109453, 0.006616859768620188438, 0.009925289652930347276, 0.01323371953724050698 ),
 .UNSPECIFIED. ) ;
#35611 = CARTESIAN_POINT ( 'NONE',  ( -0.1065646865916160396, 105.8844662015456777, 5.332932678536313809 ) ) ;
#35612 = VECTOR ( 'NONE', #34826, 1000.000000000000000 ) ;
#35613 = CYLINDRICAL_SURFACE ( 'NONE', #34301, 5.588000000000006295 ) ;
#35614 = DIRECTION ( 'NONE',  ( 0.8745520943968235761, -0.4849315768086558398, 0.000000000000000000 ) ) ;
#35615 = CARTESIAN_POINT ( 'NONE',  ( -2.045891073389006554, 34.07700515036425770, 0.6666589014435788663 ) ) ;
#35616 = CARTESIAN_POINT ( 'NONE',  ( 2.160664645061408873, 117.9909145081919917, 0.7315704174731482157 ) ) ;
#35617 = CARTESIAN_POINT ( 'NONE',  ( -3.990024091077861268, 18.91925256873344807, 2.329872802929966902 ) ) ;
#35618 = CARTESIAN_POINT ( 'NONE',  ( -2.878135459294852705, -8.718908198948343014, 7.912908975683875745 ) ) ;
#35619 = CARTESIAN_POINT ( 'NONE',  ( -5.482592266946507031, 117.2336767834907363, -0.8194921820605090002 ) ) ;
#35620 = CARTESIAN_POINT ( 'NONE',  ( -1.907654281882167568, 121.7602717223048501, -0.3165470008995034945 ) ) ;
#35621 = CARTESIAN_POINT ( 'NONE',  ( -22.83540780336928577, 150.4058779721138421, -0.4563057931615319140 ) ) ;
#35622 = CARTESIAN_POINT ( 'NONE',  ( 0.7529411215435434235, 106.0533076082122790, -5.240246454641519946 ) ) ;
#35623 = CARTESIAN_POINT ( 'NONE',  ( 0.09871621327668905765, 104.6144662015456959, 4.835249534459434173 ) ) ;
#35624 = CARTESIAN_POINT ( 'NONE',  ( -4.492784857928645792, 12.16275517495587977, -1.104450737933446725 ) ) ;
#35625 = CARTESIAN_POINT ( 'NONE',  ( -6.019568728095220427E-14, 78.83346620154574680, 1.000738015618740492E-16 ) ) ;
#35626 = CARTESIAN_POINT ( 'NONE',  ( -15.73471677570942262, 120.8416612192442159, -0.3144170877234248596 ) ) ;
#35627 = CARTESIAN_POINT ( 'NONE',  ( 3.205191379615736746, -14.47393913169138102, 3.051678166811226500 ) ) ;
#35628 = CARTESIAN_POINT ( 'NONE',  ( 2.908797093394981381, 122.3314979878274045, -0.1372540494999658078 ) ) ;
#35629 = CARTESIAN_POINT ( 'NONE',  ( -15.62635203013939034, 121.2802728028965475, 0.2997488694636322171 ) ) ;
#35630 = ORIENTED_EDGE ( 'NONE', *, *, #40520, .F. ) ;
#35631 = CARTESIAN_POINT ( 'NONE',  ( 5.305748947172213015, 53.58606249999999704, 5.247078976224250013 ) ) ;
#35632 = VERTEX_POINT ( 'NONE', #33740 ) ;
#35633 = DIRECTION ( 'NONE',  ( -5.188838149069472160E-16, 1.699382548006136559E-16, 1.000000000000000000 ) ) ;
#35634 = AXIS2_PLACEMENT_3D ( 'NONE', #30373, #36375, #23338 ) ;
#35635 = CARTESIAN_POINT ( 'NONE',  ( 4.376329468599289285, -15.53264713215277126, 4.356271056886698467 ) ) ;
#35636 = CARTESIAN_POINT ( 'NONE',  ( -4.101170551582197454, 118.4217611105734846, 0.8082045602434786424 ) ) ;
#35637 = CARTESIAN_POINT ( 'NONE',  ( 22.13784291382268066, 148.5290936231802448, -1.147597636374165342 ) ) ;
#35638 = CARTESIAN_POINT ( 'NONE',  ( 2.522041008973656240, -3.380034811851383214, 3.874746376371965617 ) ) ;
#35639 = CARTESIAN_POINT ( 'NONE',  ( -57.44144277618438110, 2.261329945018465182, -1.861782675839624313 ) ) ;
#35640 = EDGE_LOOP ( 'NONE', ( #6176, #13640, #23807, #29397 ) ) ;
#35641 = CARTESIAN_POINT ( 'NONE',  ( -49.23283723365199904, 17.42967204962654648, -5.014312523173099834 ) ) ;
#35642 = CARTESIAN_POINT ( 'NONE',  ( 9.132817075745611705E-16, 9.026346327358515609, 0.000000000000000000 ) ) ;
#35643 = FILL_AREA_STYLE_COLOUR ( '', #32483 ) ;
#35644 = CARTESIAN_POINT ( 'NONE',  ( -16.48900842742864015, 139.9843038322558186, 1.489460148179643895 ) ) ;
#35645 = CARTESIAN_POINT ( 'NONE',  ( 5.124055468070814356, 116.9398885036888487, 0.3846614261691105874 ) ) ;
#35646 =( BOUNDED_CURVE ( )  B_SPLINE_CURVE ( 3, ( #39324, #20327, #33150, #23522 ),
 .UNSPECIFIED., .F., .T. ) 
 B_SPLINE_CURVE_WITH_KNOTS ( ( 4, 4 ),
 ( 3.141592653589793560, 4.712388980384689674 ),
 .UNSPECIFIED. ) 
 CURVE ( )  GEOMETRIC_REPRESENTATION_ITEM ( )  RATIONAL_B_SPLINE_CURVE ( ( 1.000000000000000000, 0.8047378541243650485, 0.8047378541243650485, 1.000000000000000000 ) ) 
 REPRESENTATION_ITEM ( '' )  );
#35647 = CARTESIAN_POINT ( 'NONE',  ( 16.12483552447390167, 131.4332636412663931, -1.626400019052950396 ) ) ;
#35648 = CARTESIAN_POINT ( 'NONE',  ( -20.63667788919588730, 149.2407879669073054, -2.389545083207230913 ) ) ;
#35649 = CARTESIAN_POINT ( 'NONE',  ( -58.87911280034276018, -0.2081424763510641984, -0.2451831517279998984 ) ) ;
#35650 = AXIS2_PLACEMENT_3D ( 'NONE', #10659, #14474, #40289 ) ;
#35651 = VERTEX_POINT ( 'NONE', #13917 ) ;
#35652 = CARTESIAN_POINT ( 'NONE',  ( 4.482242274157552053, 118.1125264040518061, -0.5758228734123297388 ) ) ;
#35653 = CARTESIAN_POINT ( 'NONE',  ( 9.482824821899882295, 153.9068681542131856, -0.6648444853843684665 ) ) ;
#35654 = VERTEX_POINT ( 'NONE', #36931 ) ;
#35655 = CARTESIAN_POINT ( 'NONE',  ( 0.009931517865179408100, 119.6374844068871397, -0.4970137656763582990 ) ) ;
#35656 = CARTESIAN_POINT ( 'NONE',  ( 3.340243159461592448, -15.49156354636899202, 3.813188716183662397 ) ) ;
#35657 = AXIS2_PLACEMENT_3D ( 'NONE', #10231, #30289, #20902 ) ;
#35658 = CIRCLE ( 'NONE', #22692, 0.6350000000000014522 ) ;
#35659 = CARTESIAN_POINT ( 'NONE',  ( 4.615704859843055452, 105.1215186159430885, -2.696439918938831948 ) ) ;
#35660 = DIRECTION ( 'NONE',  ( -0.000000000000000000, -0.000000000000000000, -1.000000000000000000 ) ) ;
#35661 = CARTESIAN_POINT ( 'NONE',  ( -4.933822780877020087, 117.6566500539053379, 0.7550610955488965548 ) ) ;
#35662 = CARTESIAN_POINT ( 'NONE',  ( 11.01900745353688293, 123.5714170083676748, 1.527874194239944305 ) ) ;
#35663 = FACE_OUTER_BOUND ( 'NONE', #27607, .T. ) ;
#35664 = TOROIDAL_SURFACE ( 'NONE', #31577, 17.68910244842765778, 0.6350000000000000089 ) ;
#35665 = CARTESIAN_POINT ( 'NONE',  ( 4.377640660406503237, 26.40621510375495973, 1.544744264128281364 ) ) ;
#35666 = CARTESIAN_POINT ( 'NONE',  ( 11.96249418807702547, 130.4318746828361100, 0.4433914376541254199 ) ) ;
#35667 = LINE ( 'NONE', #41643, #17403 ) ;
#35669 = VERTEX_POINT ( 'NONE', #20716 ) ;
#35668 = CARTESIAN_POINT ( 'NONE',  ( -45.11192300388034937, 21.16850173503701527, -3.873855239238740200 ) ) ;
#35670 = CARTESIAN_POINT ( 'NONE',  ( -15.37877921309976870, 79.99470228764801050, -1.524000000000001576 ) ) ;
#35671 = CARTESIAN_POINT ( 'NONE',  ( 18.35410564743290607, 77.35382415001784295, 5.016499999999999737 ) ) ;
#35672 = CARTESIAN_POINT ( 'NONE',  ( -51.25515452438769159, 14.22119815747982052, 4.625262746768662225 ) ) ;
#35673 = CARTESIAN_POINT ( 'NONE',  ( -8.798071503382049130, 117.6842349159514640, -0.1758064068840608507 ) ) ;
#35674 = CARTESIAN_POINT ( 'NONE',  ( -5.871452009091403745, 88.73331249999998249, 5.016499999999999737 ) ) ;
#35675 = CARTESIAN_POINT ( 'NONE',  ( -17.22465686008793995, 48.97870818484556565, 1.524000000000002242 ) ) ;
#35676 = CARTESIAN_POINT ( 'NONE',  ( -56.90590057130552282, 4.418898835881354792, 2.427662546266514454 ) ) ;
#35677 = CARTESIAN_POINT ( 'NONE',  ( -58.37934292759150168, 0.9822739792931106662, 1.208960021102198246 ) ) ;
#35678 = CARTESIAN_POINT ( 'NONE',  ( -13.52003375314306055, 119.6474162840860771, 0.03304800104807582156 ) ) ;
#35679 = VERTEX_POINT ( 'NONE', #4564 ) ;
#35680 = CARTESIAN_POINT ( 'NONE',  ( -55.52324119379100864, 8.418761648454426094, -1.955819887484162356 ) ) ;
#35681 = CARTESIAN_POINT ( 'NONE',  ( -6.945483162495717622, 121.9345112681876060, -0.2969950648847965446 ) ) ;
#35682 = VERTEX_POINT ( 'NONE', #1363 ) ;
#35683 = CARTESIAN_POINT ( 'NONE',  ( 3.248299790614018967, 115.7029686237793271, -1.528078099553393798 ) ) ;
#35684 = CARTESIAN_POINT ( 'NONE',  ( -15.74517894787283012, 145.7063497038720925, -0.5455200375299574800 ) ) ;
#35685 = CARTESIAN_POINT ( 'NONE',  ( 4.290763117780162617, -14.65756668531598095, 4.875966813445055337 ) ) ;
#35686 = CARTESIAN_POINT ( 'NONE',  ( -6.834340443517129771, 118.4250403807481575, 0.8562881416378698152 ) ) ;
#35687 = FACE_OUTER_BOUND ( 'NONE', #41733, .T. ) ;
#35688 = CARTESIAN_POINT ( 'NONE',  ( 15.55067499035023815, 120.8127473925414108, 0.5415919938617849150 ) ) ;
#35689 = CARTESIAN_POINT ( 'NONE',  ( -0.001311298634349677191, 120.9974662015458193, 0.06562274578655612201 ) ) ;
#35690 = CARTESIAN_POINT ( 'NONE',  ( 4.831562716854217676, 118.5266822147775940, -0.7494263288004241463 ) ) ;
#35691 = CARTESIAN_POINT ( 'NONE',  ( -0.6941440390767986690, 12.16465383894776409, -0.6855803344193639459 ) ) ;
#35692 = CARTESIAN_POINT ( 'NONE',  ( -14.79880180360901498, 120.3086691715681695, -0.4511713404943135108 ) ) ;
#35693 = LINE ( 'NONE', #2695, #2554 ) ;
#35694 = CARTESIAN_POINT ( 'NONE',  ( -23.62918761621517660, 82.45577215708875940, 1.269999999999993134 ) ) ;
#35695 = ORIENTED_EDGE ( 'NONE', *, *, #10763, .F. ) ;
#35696 = CARTESIAN_POINT ( 'NONE',  ( -8.703195117136894865, 118.2213682157332499, 0.5883247612393129877 ) ) ;
#35697 = EDGE_LOOP ( 'NONE', ( #32013, #23072, #41844, #21551, #6151 ) ) ;
#35698 = LINE ( 'NONE', #19277, #38167 ) ;
#35699 = CARTESIAN_POINT ( 'NONE',  ( 20.80232463633019080, 150.1670661137953289, 2.219268881695795059 ) ) ;
#35700 = CARTESIAN_POINT ( 'NONE',  ( 0.01147819631899514407, 118.5605975114896609, -0.5744158801423953076 ) ) ;
#35701 = CARTESIAN_POINT ( 'NONE',  ( 0.1324238259082184954, -4.506001423838159603, -0.9708255322318050107 ) ) ;
#35702 = CARTESIAN_POINT ( 'NONE',  ( 0.7792876995799051798, 11.14506788600763443, 8.385000233822015758 ) ) ;
#35703 = CARTESIAN_POINT ( 'NONE',  ( -10.85289063249360275, 119.5270080912504653, -1.298249717235596679 ) ) ;
#35704 = CARTESIAN_POINT ( 'NONE',  ( 4.680411924161218096, 117.9630966871662707, -0.7259034715361608603 ) ) ;
#35705 = ADVANCED_FACE ( 'NONE', ( #29688 ), #14321, .F. ) ;
#35706 = CARTESIAN_POINT ( 'NONE',  ( 2.498958912387863940, 107.2142675576569530, 4.733253560342793875 ) ) ;
#35707 = EDGE_CURVE ( 'NONE', #6038, #21896, #27684, .T. ) ;
#35708 = CARTESIAN_POINT ( 'NONE',  ( -3.758730197597831779, 121.0943292417197199, -0.07510837462871998438 ) ) ;
#35709 = EDGE_LOOP ( 'NONE', ( #25834, #12085, #2292, #12630 ) ) ;
#35710 = CARTESIAN_POINT ( 'NONE',  ( -11.66906004923080609, 122.8035986606355152, -1.736571914056904919 ) ) ;
#35711 = CARTESIAN_POINT ( 'NONE',  ( 6.120062074970366695, -14.59381343598747982, -0.2446369611249375742 ) ) ;
#35712 = DIRECTION ( 'NONE',  ( 1.000000000000000000, 0.000000000000000000, -4.553079989440420948E-16 ) ) ;
#35713 = B_SPLINE_CURVE_WITH_KNOTS ( 'NONE', 3,
 ( #5943, #28502, #9332, #2950, #39147, #28914, #18902, #9951, #12524, #31699, #29123, #9534, #25927, #6555, #38726, #15502, #31912, #41929, #22089, #12316 ),
 .UNSPECIFIED., .F., .F.,
 ( 4, 2, 2, 2, 2, 2, 2, 2, 2, 4 ),
 ( -5.999999999773951516E-08, 0.0007881763970578359617, 0.001576412794115669615, 0.002364649191173503161, 0.003152885588231336706, 0.003941121985289170251, 0.004729358382347004230, 0.006305831176462709485, 0.009458776764694155556, 0.01261172235292560423 ),
 .UNSPECIFIED. ) ;
#35714 = CARTESIAN_POINT ( 'NONE',  ( -46.42538233320968288, 20.85422009098716956, -4.815137874471035140 ) ) ;
#35715 = EDGE_LOOP ( 'NONE', ( #36396, #209, #3554, #5668 ) ) ;
#35716 = CARTESIAN_POINT ( 'NONE',  ( 18.24092514812179289, 147.9371514012413229, 2.391122828403475342 ) ) ;
#35717 = CARTESIAN_POINT ( 'NONE',  ( 2.656309428775586845, -12.29155461912079339, 0.4553234995023021647 ) ) ;
#35718 = DIRECTION ( 'NONE',  ( -0.01731298258488073519, 0.9998501190848635423, -1.788962107505278613E-16 ) ) ;
#35719 = CARTESIAN_POINT ( 'NONE',  ( -4.141015252736775842, 122.5143120247930142, 0.07252455213604060147 ) ) ;
#35720 = CARTESIAN_POINT ( 'NONE',  ( 8.390987441844862005, -15.30508105673078667, -0.4368898320763015541 ) ) ;
#35721 = CARTESIAN_POINT ( 'NONE',  ( 9.322631400391582446, 123.9819092696984910, 0.6064563484049506625 ) ) ;
#35722 = CARTESIAN_POINT ( 'NONE',  ( 5.526300601521314526, 159.0395019988757781, -0.6540312330581287137 ) ) ;
#35723 = CARTESIAN_POINT ( 'NONE',  ( 5.177913976931214357, 57.14999999999996305, -5.372099999999997877 ) ) ;
#35724 = CARTESIAN_POINT ( 'NONE',  ( 4.581721556995678846, -15.30239758790170157, -0.5121114949450596976 ) ) ;
#35725 = EDGE_CURVE ( 'NONE', #4992, #31070, #4571, .T. ) ;
#35726 = CARTESIAN_POINT ( 'NONE',  ( -20.50175740331293284, 129.0975500345852822, -0.3894088793431773610 ) ) ;
#35727 = EDGE_LOOP ( 'NONE', ( #23332, #37446, #13606, #25956 ) ) ;
#35728 = CARTESIAN_POINT ( 'NONE',  ( 8.182757305131426406, 120.8045583724933039, -1.052530632093990670 ) ) ;
#35729 = CARTESIAN_POINT ( 'NONE',  ( 2.293129817604454335, -15.49007597679844395, 5.904469655623132418 ) ) ;
#35730 = CARTESIAN_POINT ( 'NONE',  ( -9.269771126213486312, 123.9149913687586064, -0.6034020272129926310 ) ) ;
#35731 = CARTESIAN_POINT ( 'NONE',  ( 3.564576864782785570, -14.06793500455072454, 4.479818044377421593 ) ) ;
#35732 = CARTESIAN_POINT ( 'NONE',  ( -5.091661282192257332, 117.1433449680017276, 0.3971322054743541274 ) ) ;
#35733 = CARTESIAN_POINT ( 'NONE',  ( -6.439805278602227377E-14, 159.6054662015457382, 1.008550168686281963E-16 ) ) ;
#35734 = VERTEX_POINT ( 'NONE', #26706 ) ;
#35735 = CARTESIAN_POINT ( 'NONE',  ( 2.829288187452689396, 6.340478445469713620, 3.655570690059357197 ) ) ;
#35736 = CARTESIAN_POINT ( 'NONE',  ( -0.4952506866058259405, 105.1225159476502711, 5.321743445971568676 ) ) ;
#35737 = CARTESIAN_POINT ( 'NONE',  ( -4.828903201324592942, 117.4062739125616162, 1.009435533365967697 ) ) ;
#35738 = CARTESIAN_POINT ( 'NONE',  ( 3.332917225768783798, 108.2589911827716520, 4.156415063234818241 ) ) ;
#35739 = CARTESIAN_POINT ( 'NONE',  ( -7.010790661031958138, 121.7392789538311462, 0.3431444702839729910 ) ) ;
#35740 = CARTESIAN_POINT ( 'NONE',  ( -0.5832499861179958334, 10.72304255322087307, 4.598074068532726599 ) ) ;
#35741 = CARTESIAN_POINT ( 'NONE',  ( 22.31420326625516637, 142.2114994846844240, 1.760598597564681622 ) ) ;
#35742 = CARTESIAN_POINT ( 'NONE',  ( 15.72385166996613570, 146.8976323831864477, 0.3141999770531622160 ) ) ;
#35744 = CARTESIAN_POINT ( 'NONE',  ( 1.147165779964274046, 117.8708904510121016, -0.5694250185432008227 ) ) ;
#35743 = CARTESIAN_POINT ( 'NONE',  ( -14.73199999999999754, 61.59499999999999886, -5.016499999999999737 ) ) ;
#35745 = CARTESIAN_POINT ( 'NONE',  ( -3.586339569854333664, 7.474549112184490696, -2.913498476264247294 ) ) ;
#35746 = CARTESIAN_POINT ( 'NONE',  ( -9.554367121731717205, 118.3624989119526418, -0.8896461348445368067 ) ) ;
#35747 = EDGE_CURVE ( 'NONE', #26127, #4116, #7301, .T. ) ;
#35748 = VERTEX_POINT ( 'NONE', #31150 ) ;
#35749 = CARTESIAN_POINT ( 'NONE',  ( -5.910930898603252714, 121.4708175001875077, 0.1161132702817544021 ) ) ;
#35750 = CARTESIAN_POINT ( 'NONE',  ( 6.030629465787032295, -12.69248357272054228, 1.053518048143269548 ) ) ;
#35751 = DIRECTION ( 'NONE',  ( 0.9998004120163608288, 0.000000000000000000, 0.01997839162482736852 ) ) ;
#35752 = EDGE_CURVE ( 'NONE', #27898, #34334, #29047, .T. ) ;
#35754 = ORIENTED_EDGE ( 'NONE', *, *, #1518, .F. ) ;
#35753 = CIRCLE ( 'NONE', #17373, 0.2540000000000006142 ) ;
#35755 = CARTESIAN_POINT ( 'NONE',  ( 19.45004534592201040, 148.0998626603252148, 2.515250464377977391 ) ) ;
#35756 = CARTESIAN_POINT ( 'NONE',  ( -10.73808814597608396, 77.14487411131504757, -1.269999999999998241 ) ) ;
#35757 = DIRECTION ( 'NONE',  ( -0.000000000000000000, -0.000000000000000000, -1.000000000000000000 ) ) ;
#35758 = CARTESIAN_POINT ( 'NONE',  ( -22.75813664408071446, 148.5871737753741115, 0.7284712318767733175 ) ) ;
#35759 = CARTESIAN_POINT ( 'NONE',  ( 0.004910662370358530836, 159.5928157220454295, -0.2457496255665020946 ) ) ;
#35760 = ADVANCED_FACE ( 'NONE', ( #30943 ), #37214, .T. ) ;
#35761 = CARTESIAN_POINT ( 'NONE',  ( -5.450291846086723346, 56.51500000000001478, -4.451173312910844615 ) ) ;
#35762 = CARTESIAN_POINT ( 'NONE',  ( -50.94786445731823221, 14.55500684364030661, 4.556750753989597058 ) ) ;
#35763 = CARTESIAN_POINT ( 'NONE',  ( -47.06635113313992491, 25.00568333085942996, 1.230463370088882069 ) ) ;
#35764 = CARTESIAN_POINT ( 'NONE',  ( -4.812557187411091064, 117.4080492109849416, -1.196763905027394159 ) ) ;
#35765 = CARTESIAN_POINT ( 'NONE',  ( -41.88683177698051452, 22.33947639032530219, 1.656270940288490312 ) ) ;
#35766 = CARTESIAN_POINT ( 'NONE',  ( -19.05000000000000782, 71.11999999999999034, 5.714999999999999858 ) ) ;
#35767 = CARTESIAN_POINT ( 'NONE',  ( -4.678425872278161535, 118.0125782974996582, 0.6042734876502935393 ) ) ;
#35768 = CARTESIAN_POINT ( 'NONE',  ( -58.18636467486479091, 0.07352994790495170907, -0.3924542439260719773 ) ) ;
#35769 = PRODUCT ( 'MAS-162', 'MAS-162', '', ( #6825 ) ) ;
#35770 = ORIENTED_EDGE ( 'NONE', *, *, #24850, .F. ) ;
#35771 = ORIENTED_EDGE ( 'NONE', *, *, #6839, .F. ) ;
#35772 = CARTESIAN_POINT ( 'NONE',  ( -3.195518864091055455, 115.6909491485452719, -1.660603084447102917 ) ) ;
#35773 = EDGE_CURVE ( 'NONE', #16976, #5685, #5193, .T. ) ;
#35774 = CARTESIAN_POINT ( 'NONE',  ( 3.370951604764516496, 118.5093630253226280, -0.7873060099658909516 ) ) ;
#35775 = CARTESIAN_POINT ( 'NONE',  ( -5.210481185491613765, 116.4925209815607730, -1.089480302653437871 ) ) ;
#35776 = CARTESIAN_POINT ( 'NONE',  ( 4.611851918533471206, 117.9566237460099103, 0.9391389632551998545 ) ) ;
#35777 = CARTESIAN_POINT ( 'NONE',  ( 2.460727335429193197, -15.06314154744310585, 4.845259171755021299 ) ) ;
#35778 = CARTESIAN_POINT ( 'NONE',  ( -9.075659781538043092, 123.1184971541203055, -0.9241268708344094751 ) ) ;
#35779 = FACE_OUTER_BOUND ( 'NONE', #19101, .T. ) ;
#35780 = EDGE_CURVE ( 'NONE', #332, #19961, #37545, .T. ) ;
#35781 = CARTESIAN_POINT ( 'NONE',  ( -4.129065684684445792, 110.9559963654141228, 3.095242660527065759 ) ) ;
#35782 = CARTESIAN_POINT ( 'NONE',  ( -19.04204117267709506, 56.84332656279845963, 1.524000000000000243 ) ) ;
#35783 = CARTESIAN_POINT ( 'NONE',  ( 7.450817465826167663, 123.6645382909113664, 0.1143006167400528322 ) ) ;
#35784 = CARTESIAN_POINT ( 'NONE',  ( -15.02674521555436371, 134.7883251604851580, -1.951091898071898978 ) ) ;
#35785 =( NAMED_UNIT ( * ) SI_UNIT ( $, .STERADIAN. ) SOLID_ANGLE_UNIT ( ) );
#35786 = CARTESIAN_POINT ( 'NONE',  ( -0.006534887713674904404, 159.5822087645323393, 0.3270325034788581497 ) ) ;
#35787 = VECTOR ( 'NONE', #37939, 1000.000000000000000 ) ;
#35788 = CARTESIAN_POINT ( 'NONE',  ( -2.277020932126007757, 115.7026820661928497, 1.618586367388850533 ) ) ;
#35789 = CARTESIAN_POINT ( 'NONE',  ( -0.001311586712342687876, 120.9974662015458193, 0.06563716238878879172 ) ) ;
#35790 = CARTESIAN_POINT ( 'NONE',  ( -3.426874451426485724, 1.805113900313119357, -3.130497002818263930 ) ) ;
#35792 = VERTEX_POINT ( 'NONE', #40756 ) ;
#35791 = CARTESIAN_POINT ( 'NONE',  ( 4.801439827634202295, 117.0090399748681875, 0.4924919612534520152 ) ) ;
#35793 = CARTESIAN_POINT ( 'NONE',  ( 5.284192421469999346, 104.6144662015304050, -0.8069602218790292714 ) ) ;
#35794 = CARTESIAN_POINT ( 'NONE',  ( 3.866904830252686054, -15.34763638737450542, 1.784481441967298743 ) ) ;
#35795 = CARTESIAN_POINT ( 'NONE',  ( -0.01133701094407592140, 119.0130636887059410, 0.5673503866435173348 ) ) ;
#35796 = CARTESIAN_POINT ( 'NONE',  ( 0.9260135661551653907, 3.379156789086214197, -0.3022368940483516897 ) ) ;
#35797 = CARTESIAN_POINT ( 'NONE',  ( -0.9473015597126430709, 116.7004868406603322, -0.2634242240387510980 ) ) ;
#35798 = CARTESIAN_POINT ( 'NONE',  ( -0.1566604602083998543, 5.914057227930348049, 0.9647682902456425902 ) ) ;
#35799 = VERTEX_POINT ( 'NONE', #21334 ) ;
#35800 = ORIENTED_EDGE ( 'NONE', *, *, #32307, .F. ) ;
#35801 = CARTESIAN_POINT ( 'NONE',  ( -41.41491986784952672, 22.70581808553410497, 0.08466666666666171348 ) ) ;
#35802 = EDGE_CURVE ( 'NONE', #36618, #20434, #10878, .T. ) ;
#35803 = CARTESIAN_POINT ( 'NONE',  ( 4.774443427420539621, 116.8297769931967309, 1.047991251433075366 ) ) ;
#35804 = CARTESIAN_POINT ( 'NONE',  ( -15.77383231466701297, 147.9505201145231865, 0.6473862450635484711 ) ) ;
#35805 = CARTESIAN_POINT ( 'NONE',  ( 2.629318991877339418, -14.82094413389492615, 5.549789958447211013 ) ) ;
#35806 = CARTESIAN_POINT ( 'NONE',  ( 7.333780486663145304, 155.8804291298944236, -1.515250586328038773 ) ) ;
#35807 = CARTESIAN_POINT ( 'NONE',  ( -19.78444808418236178, 147.9128418260961837, -2.517891032746078839 ) ) ;
#35808 = CARTESIAN_POINT ( 'NONE',  ( -47.90792207059400454, 19.42479681086476617, -5.305186633237529037 ) ) ;
#35809 = CARTESIAN_POINT ( 'NONE',  ( 2.931439949929583122, -14.82325452411255640, 4.117531814738872420 ) ) ;
#35810 = CARTESIAN_POINT ( 'NONE',  ( -5.164545546852735036, 32.23602039546388909, 1.233576701498339201 ) ) ;
#35811 = CARTESIAN_POINT ( 'NONE',  ( 1.609565093910530154, 156.2658572007470639, -0.2453390865415086830 ) ) ;
#35812 = ORIENTED_EDGE ( 'NONE', *, *, #10812, .T. ) ;
#35813 = CARTESIAN_POINT ( 'NONE',  ( -0.01009854879487165520, 117.2429491485453070, 0.5053730761602109878 ) ) ;
#35814 = FACE_OUTER_BOUND ( 'NONE', #22914, .T. ) ;
#35815 = VECTOR ( 'NONE', #24659, 1000.000000000000114 ) ;
#35816 = EDGE_CURVE ( 'NONE', #18326, #41007, #40858, .T. ) ;
#35817 = CARTESIAN_POINT ( 'NONE',  ( -58.41257333834132481, 0.1697474083129230094, 0.8453419536833289838 ) ) ;
#35818 = ADVANCED_FACE ( 'NONE', ( #37756 ), #31769, .T. ) ;
#35819 = AXIS2_PLACEMENT_3D ( 'NONE', #3781, #35510, #3568 ) ;
#35820 = CARTESIAN_POINT ( 'NONE',  ( -8.473844426907703564, 67.77203500197072117, 1.270000000000003570 ) ) ;
#35821 = CARTESIAN_POINT ( 'NONE',  ( 21.60220573293482715, 132.6646020023713959, 0.2978857061057722522 ) ) ;
#35822 = CONICAL_SURFACE ( 'NONE', #12002, 14.73199999999999577, 0.7853981633974488341 ) ;
#35823 = CARTESIAN_POINT ( 'NONE',  ( -7.694720906311372843, 124.7202454748262710, -0.1538800020430350635 ) ) ;
#35824 = DIRECTION ( 'NONE',  ( -0.8745520943968241312, 0.4849315768086548406, -5.691349986800536046E-16 ) ) ;
#35825 = CARTESIAN_POINT ( 'NONE',  ( -2.646443841375008432, -8.127818987380491578, -3.789199236247322133 ) ) ;
#35826 = CARTESIAN_POINT ( 'NONE',  ( -4.834802360910630981, 32.27718159487177729, 0.9856153350916389000 ) ) ;
#35827 = CARTESIAN_POINT ( 'NONE',  ( 4.930931983215351977, 118.2512723699127832, 1.012396356527061725 ) ) ;
#35828 = CARTESIAN_POINT ( 'NONE',  ( -3.618988008572157522, 19.14412854911201123, 2.900346660497036044 ) ) ;
#35829 = CARTESIAN_POINT ( 'NONE',  ( 1.420544585151703343, -13.23898594424576203, -8.332176651214544094 ) ) ;
#35830 = CARTESIAN_POINT ( 'NONE',  ( 8.756088789680248397, 117.9414872320107435, -0.3631643394575467809 ) ) ;
#35831 = CARTESIAN_POINT ( 'NONE',  ( -1.302594956492468370, 113.6455945353133643, -2.391525302099168027 ) ) ;
#35832 = CARTESIAN_POINT ( 'NONE',  ( -23.36555825341177339, 148.7788340588663800, -0.4668994608413308267 ) ) ;
#35833 = CARTESIAN_POINT ( 'NONE',  ( 4.129667044122415476, 110.9560305189546767, -3.095181893054258282 ) ) ;
#35834 = CARTESIAN_POINT ( 'NONE',  ( -2.260567382777518119, 105.1242543621358436, 4.832464655412169741 ) ) ;
#35835 = CARTESIAN_POINT ( 'NONE',  ( -0.8080508600641240768, 24.25718022715097888, 4.550674767031389401 ) ) ;
#35836 = ADVANCED_FACE ( 'NONE', ( #34573 ), #41998, .T. ) ;
#35837 = CARTESIAN_POINT ( 'NONE',  ( -17.14500000000466784, 71.11999999999886768, -1.524000000000000909 ) ) ;
#35838 = CARTESIAN_POINT ( 'NONE',  ( -21.68875320759065062, 132.7412702629105468, -0.4333929054516006962 ) ) ;
#35839 = CARTESIAN_POINT ( 'NONE',  ( 2.770737963896511946, -14.84290363635286347, 4.452025088638788652 ) ) ;
#35840 = CARTESIAN_POINT ( 'NONE',  ( 2.292460607442518672, 118.3648483361698851, -0.7949187631362102380 ) ) ;
#35841 = CARTESIAN_POINT ( 'NONE',  ( -15.03447867299186669, 120.7699597703182945, 0.2997422626971647519 ) ) ;
#35842 = EDGE_CURVE ( 'NONE', #36653, #28149, #18825, .T. ) ;
#35843 = ORIENTED_EDGE ( 'NONE', *, *, #26054, .F. ) ;
#35844 = CARTESIAN_POINT ( 'NONE',  ( 5.177913976931209916, 65.30181249999998272, 5.372099999999993436 ) ) ;
#35845 = TOROIDAL_SURFACE ( 'NONE', #3898, 16.60960244842765832, 1.396999999999998909 ) ;
#35846 = ORIENTED_EDGE ( 'NONE', *, *, #36996, .F. ) ;
#35847 = CARTESIAN_POINT ( 'NONE',  ( -14.39766717389551864, 57.78499999999998948, 1.905000000000000471 ) ) ;
#35848 = CARTESIAN_POINT ( 'NONE',  ( 4.231574481101612051, -15.55479495760878095, 4.522910428756792278 ) ) ;
#35849 = CARTESIAN_POINT ( 'NONE',  ( -19.16692462419661425, 150.4642993720107143, 1.670612363451736249 ) ) ;
#35850 = CARTESIAN_POINT ( 'NONE',  ( 16.54768821719722993, 125.2933801378020888, -1.124873388181685030 ) ) ;
#35851 = CARTESIAN_POINT ( 'NONE',  ( 1.398650104629075797, 0.06838872207683838189, -4.420329592304430122 ) ) ;
#35852 = CARTESIAN_POINT ( 'NONE',  ( 5.901202670473767675, 78.88741954747038676, 5.016800487701043920 ) ) ;
#35853 = ORIENTED_EDGE ( 'NONE', *, *, #5023, .F. ) ;
#35854 = LINE ( 'NONE', #33287, #34059 ) ;
#35855 = VECTOR ( 'NONE', #38706, 1000.000000000000227 ) ;
#35856 = CARTESIAN_POINT ( 'NONE',  ( 0.3796903751652699888, 122.8649044353670803, 0.2268226101886974821 ) ) ;
#35857 = CARTESIAN_POINT ( 'NONE',  ( -4.678029067978729749, 117.8847919582286465, 0.8180832583663835145 ) ) ;
#35858 = CARTESIAN_POINT ( 'NONE',  ( -2.030192889891393460, 156.8313070664539168, 1.335154060002984311 ) ) ;
#35859 = CARTESIAN_POINT ( 'NONE',  ( -11.32337086946255056, 78.46996359545325106, 1.270000000000000018 ) ) ;
#35860 = CARTESIAN_POINT ( 'NONE',  ( 15.17663987144297266, 128.5586215118215705, -1.546218023206676229 ) ) ;
#35861 = CARTESIAN_POINT ( 'NONE',  ( -18.42009423903802556, 151.8926627062091086, -2.314360763190140169 ) ) ;
#35862 = CARTESIAN_POINT ( 'NONE',  ( -58.43690671596436914, -0.4125963578781866037, -0.2423173958219211055 ) ) ;
#35863 = ORIENTED_EDGE ( 'NONE', *, *, #20652, .F. ) ;
#35864 = CARTESIAN_POINT ( 'NONE',  ( 4.580295709240714608, 118.0857834188402791, -0.5549505832812218209 ) ) ;
#35865 = CARTESIAN_POINT ( 'NONE',  ( 16.03056103447425684, 147.0154580547469152, -0.5309802628845385897 ) ) ;
#35866 = ORIENTED_EDGE ( 'NONE', *, *, #38882, .T. ) ;
#35867 = CARTESIAN_POINT ( 'NONE',  ( -13.61432229890765733, 152.4534842159446271, -2.088615715084950253 ) ) ;
#35868 = CARTESIAN_POINT ( 'NONE',  ( 3.614876661864775187, -15.45153451277975165, 3.150551394879585132 ) ) ;
#35869 = CARTESIAN_POINT ( 'NONE',  ( 0.5023112062301228198, 105.1225718423296343, -5.320799118487369306 ) ) ;
#35870 = TOROIDAL_SURFACE ( 'NONE', #29720, 3.683000000000000718, 0.5080000000000000071 ) ;
#35871 = CIRCLE ( 'NONE', #18174, 17.68910244842765778 ) ;
#35872 = CARTESIAN_POINT ( 'NONE',  ( -23.43300365160792964, 82.12916405548841681, -1.524000000000006017 ) ) ;
#35873 = CARTESIAN_POINT ( 'NONE',  ( -4.896827542163006974, 117.7233055579753938, 0.7633307427583084781 ) ) ;
#35874 = CARTESIAN_POINT ( 'NONE',  ( 10.91091678335008552, 123.4376579628654014, 1.516229561143084714 ) ) ;
#35875 = LINE ( 'NONE', #9453, #39639 ) ;
#35876 = AXIS2_PLACEMENT_3D ( 'NONE', #30153, #16732, #29942 ) ;
#35877 = CARTESIAN_POINT ( 'NONE',  ( -0.9950013725589796909, 29.65466048987409309, -4.513790593961638287 ) ) ;
#35878 = CARTESIAN_POINT ( 'NONE',  ( 2.908234975202448780, 156.0868537499222839, 0.2102064236019249022 ) ) ;
#35879 = DIRECTION ( 'NONE',  ( -0.01997839162482761832, -1.040247600000950455E-18, 0.9998004120163610509 ) ) ;
#35880 = AXIS2_PLACEMENT_3D ( 'NONE', #6855, #30474, #29851 ) ;
#35881 = CARTESIAN_POINT ( 'NONE',  ( -47.61549956331939626, 19.66157307908737195, -5.197827534590571119 ) ) ;
#35882 = CARTESIAN_POINT ( 'NONE',  ( -2.183929936140839523, 116.1876165027943273, -0.08882796894186900660 ) ) ;
#35883 = CARTESIAN_POINT ( 'NONE',  ( -5.078986093043186045, 78.83346620154574680, -0.1014902294541237815 ) ) ;
#35884 = CARTESIAN_POINT ( 'NONE',  ( -46.98348089488082735, 24.79145570443871449, 2.118842393845961070 ) ) ;
#35885 = CARTESIAN_POINT ( 'NONE',  ( -28.09515292912719175, 77.51021392068167870, 1.269999999999991580 ) ) ;
#35886 = DIRECTION ( 'NONE',  ( -0.01997839162482761832, -1.040247600000950455E-18, 0.9998004120163610509 ) ) ;
#35887 = CARTESIAN_POINT ( 'NONE',  ( -5.871452009091383317, 53.58606250000000415, 5.016499999999999737 ) ) ;
#35888 = CARTESIAN_POINT ( 'NONE',  ( -4.074955089416341991, 118.2429491485453354, 0.1454234154749719787 ) ) ;
#35889 = DIRECTION ( 'NONE',  ( -4.017660918040594346E-17, 1.000000000000000000, 2.376309959284834438E-19 ) ) ;
#35890 = CARTESIAN_POINT ( 'NONE',  ( -57.34105142390578891, 4.241571993195719870, -1.063007725424832192E-14 ) ) ;
#35891 = CARTESIAN_POINT ( 'NONE',  ( -57.93941708942283952, 2.052042089854988483, 1.628789306319508245 ) ) ;
#35892 = CARTESIAN_POINT ( 'NONE',  ( -21.48671512862192756, 132.5742979909900328, -0.1330572995313747120 ) ) ;
#35893 = ORIENTED_EDGE ( 'NONE', *, *, #19283, .T. ) ;
#35894 = CARTESIAN_POINT ( 'NONE',  ( -53.84631020981186822, 15.55534180636754193, -1.120024938224189362E-14 ) ) ;
#35895 = CARTESIAN_POINT ( 'NONE',  ( -6.964740248879998319, 121.9459328161491385, -0.2343094465020360562 ) ) ;
#35896 = ORIENTED_EDGE ( 'NONE', *, *, #6536, .T. ) ;
#35897 = CYLINDRICAL_SURFACE ( 'NONE', #28748, 0.5080000000000002292 ) ;
#35898 = CARTESIAN_POINT ( 'NONE',  ( -9.115475939616176859, 153.9201329141909866, -0.2944159349489392508 ) ) ;
#35899 = CARTESIAN_POINT ( 'NONE',  ( 4.815776949948430641, -14.65450223259012752, 4.385166865640996114 ) ) ;
#35900 = CARTESIAN_POINT ( 'NONE',  ( -21.17963693554089488, 147.9292434580435724, 1.516351520135284847 ) ) ;
#35901 = DIRECTION ( 'NONE',  ( -5.206863593109713661E-17, 1.000000000000000000, -1.077750396879097183E-30 ) ) ;
#35902 = CARTESIAN_POINT ( 'NONE',  ( 6.905604733424301145, 117.2797055272990292, 0.4577529590079177368 ) ) ;
#35903 = CIRCLE ( 'NONE', #19538, 0.6350000000000014522 ) ;
#35904 = CARTESIAN_POINT ( 'NONE',  ( 12.79726118125660150, 133.7150753560844976, 0.3789659047097265199 ) ) ;
#35905 = DIRECTION ( 'NONE',  ( 1.000000000000000000, 0.000000000000000000, 0.000000000000000000 ) ) ;
#35906 = CARTESIAN_POINT ( 'NONE',  ( -0.2932310942476468174, 5.691741097161698626, 0.9303163870417268111 ) ) ;
#35907 = CARTESIAN_POINT ( 'NONE',  ( -22.96225337745244488, 150.1545470440437953, -0.6883021358963677949 ) ) ;
#35908 = CARTESIAN_POINT ( 'NONE',  ( -13.85159022459153988, 16.51000000000000156, 5.016499999999999737 ) ) ;
#35909 = DIRECTION ( 'NONE',  ( 0.5149185422762211362, -0.8572391118119444542, 0.000000000000000000 ) ) ;
#35910 = VERTEX_POINT ( 'NONE', #41174 ) ;
#35911 = CARTESIAN_POINT ( 'NONE',  ( -8.625020111792197852, 118.6230397979781799, 0.7981352872006625132 ) ) ;
#35912 = VERTEX_POINT ( 'NONE', #7956 ) ;
#35913 = CARTESIAN_POINT ( 'NONE',  ( -15.02280320640473121, 73.03244360434628391, -1.269999999999999796 ) ) ;
#35914 = CARTESIAN_POINT ( 'NONE',  ( -0.009513433763583356226, 117.6614778598761291, 0.4760911276077179899 ) ) ;
#35915 = CARTESIAN_POINT ( 'NONE',  ( 17.73303733098136448, 151.6044147853587845, -1.711203799303050666 ) ) ;
#35916 = CARTESIAN_POINT ( 'NONE',  ( 0.9260135661551653907, 3.379156789086214197, -0.3022368940483516897 ) ) ;
#35917 = CARTESIAN_POINT ( 'NONE',  ( -2.144872632962109726, 6.596990873201863614, -8.179991544870226505 ) ) ;
#35918 = CARTESIAN_POINT ( 'NONE',  ( -21.77023485109867451, 148.7205309135917730, -2.145821470179948509 ) ) ;
#35919 = CARTESIAN_POINT ( 'NONE',  ( 4.677687236059855813, 117.8847412557266239, -0.8181935875056758345 ) ) ;
#35920 = CARTESIAN_POINT ( 'NONE',  ( 7.499048524200883747, 123.6595150816924047, 0.1842243911843320370 ) ) ;
#35921 = CARTESIAN_POINT ( 'NONE',  ( 11.17088054096560334, 124.6236798342360856, -0.9649352710901085706 ) ) ;
#35922 = CARTESIAN_POINT ( 'NONE',  ( -9.145901261935915016, 124.1724329610943300, -0.1484858654357238128 ) ) ;
#35923 = VERTEX_POINT ( 'NONE', #33947 ) ;
#35924 = CARTESIAN_POINT ( 'NONE',  ( -3.977359857055012604, 157.1622345443605582, -1.793852766001656329 ) ) ;
#35925 = CARTESIAN_POINT ( 'NONE',  ( 3.918620257527314799, -15.59263167233598857, 4.836928646374421881 ) ) ;
#35926 = LINE ( 'NONE', #22889, #14256 ) ;
#35927 = CARTESIAN_POINT ( 'NONE',  ( -48.56815661899837977, 19.24492339269602681, -5.224590812749990931 ) ) ;
#35928 = EDGE_LOOP ( 'NONE', ( #20944, #9473, #23833, #10022 ) ) ;
#35929 = CARTESIAN_POINT ( 'NONE',  ( 3.364155546990415857, 119.5845705363850442, 0.8331338896180615627 ) ) ;
#35930 = CARTESIAN_POINT ( 'NONE',  ( 3.606404759574667995, -11.68799792153887296, 0.6759542868570080909 ) ) ;
#35931 = CARTESIAN_POINT ( 'NONE',  ( 5.165779723667151657, 115.7029491485453008, 1.236970719217007408 ) ) ;
#35932 = CARTESIAN_POINT ( 'NONE',  ( -3.175984444280743446, 117.6701293611589278, 0.8859276027576485912 ) ) ;
#35933 = CARTESIAN_POINT ( 'NONE',  ( -8.304712878168881929, 22.30428017260781459, 1.495267265505846765 ) ) ;
#35934 = CARTESIAN_POINT ( 'NONE',  ( 1.557716402914177012, 120.7946061759640486, 0.2396963980366531854 ) ) ;
#35935 = CARTESIAN_POINT ( 'NONE',  ( 9.582280438405291534, 118.3624989119526418, -0.5072503739029415870 ) ) ;
#35936 = CARTESIAN_POINT ( 'NONE',  ( -5.010144981628188887, 117.3993855238222608, -0.7522679339500687457 ) ) ;
#35937 = DIRECTION ( 'NONE',  ( -5.188838149069471174E-16, 1.699382548006136313E-16, 1.000000000000000000 ) ) ;
#35938 = CARTESIAN_POINT ( 'NONE',  ( -8.078287538471746743, 158.6595088495342338, -0.1614234102745197019 ) ) ;
#35939 = ORIENTED_EDGE ( 'NONE', *, *, #22903, .T. ) ;
#35940 = CARTESIAN_POINT ( 'NONE',  ( 6.747353831446265104, 120.9730903663792247, -0.7368456446025557494 ) ) ;
#35941 = CARTESIAN_POINT ( 'NONE',  ( 5.253579998758207914, -14.72808323979572442, 3.743261050348050123 ) ) ;
#35942 = CARTESIAN_POINT ( 'NONE',  ( -15.39048793250127289, 143.5427300040290106, -0.9094471879209007348 ) ) ;
#35943 = CARTESIAN_POINT ( 'NONE',  ( 3.464659682708206123, -14.15734315221130224, 4.609430909834149048 ) ) ;
#35944 = DIRECTION ( 'NONE',  ( -4.017660918040594346E-17, 1.000000000000000000, 2.376309959284834438E-19 ) ) ;
#35945 = CARTESIAN_POINT ( 'NONE',  ( 22.75563279970854325, 137.3797884758947703, 0.4783205966563214839 ) ) ;
#35946 = ORIENTED_EDGE ( 'NONE', *, *, #24320, .F. ) ;
#35947 = CARTESIAN_POINT ( 'NONE',  ( -4.478778176974228309, 3.316883148187759645, 1.141857468124592101 ) ) ;
#35948 = CARTESIAN_POINT ( 'NONE',  ( 1.511522926053362248, 105.1238775886715047, 5.125126382528155666 ) ) ;
#35949 = CARTESIAN_POINT ( 'NONE',  ( -5.008842170714641107, 117.3975374489157133, 0.7756408261732131715 ) ) ;
#35950 = CARTESIAN_POINT ( 'NONE',  ( 7.213960532363565825, 86.35999999999998522, 1.904999999999995364 ) ) ;
#35951 = CARTESIAN_POINT ( 'NONE',  ( -6.092137319721709687, 121.3195672157765728, 0.2700191901338648282 ) ) ;
#35952 = CARTESIAN_POINT ( 'NONE',  ( -2.651420880294951488, 7.049774601622781134, -3.792306073587544901 ) ) ;
#35953 = CARTESIAN_POINT ( 'NONE',  ( -0.01443894962469085066, 159.4760848062415732, 0.7225840825867287931 ) ) ;
#35954 = CARTESIAN_POINT ( 'NONE',  ( -48.44802435120097783, 18.63281525352669021, -5.198089189982387559 ) ) ;
#35956 = CARTESIAN_POINT ( 'NONE',  ( 0.02768730785345232051, 158.9256195073445213, -1.385586103196075447 ) ) ;
#35955 = DIRECTION ( 'NONE',  ( -0.8745520943968235761, 0.4849315768086558398, -4.268512490100410909E-16 ) ) ;
#35957 = CARTESIAN_POINT ( 'NONE',  ( -1.220754042303205500, 16.12054255322086860, -4.471266627502475721 ) ) ;
#35958 = CARTESIAN_POINT ( 'NONE',  ( -14.73023064483748712, 156.1040168620350244, -1.249499669456201500 ) ) ;
#35959 = ORIENTED_EDGE ( 'NONE', *, *, #20866, .T. ) ;
#35960 = CARTESIAN_POINT ( 'NONE',  ( -1.630522158633651797, 156.2764358050213787, 0.3353572448990094768 ) ) ;
#35962 = CARTESIAN_POINT ( 'NONE',  ( 6.287662417442902552, -13.15673151805442309, 0.9153646538742283845 ) ) ;
#35961 = VECTOR ( 'NONE', #35718, 999.9999999999998863 ) ;
#35963 = CARTESIAN_POINT ( 'NONE',  ( -2.742874663339857744, 107.9144754008248981, -4.446420073853355248 ) ) ;
#35964 = ORIENTED_EDGE ( 'NONE', *, *, #15232, .F. ) ;
#35965 = CARTESIAN_POINT ( 'NONE',  ( -0.03245814172817947096, 158.1186941186938952, 1.624338139048501439 ) ) ;
#35966 = FACE_OUTER_BOUND ( 'NONE', #1909, .T. ) ;
#35967 = CARTESIAN_POINT ( 'NONE',  ( 8.935197197525127422, 123.9063447689825779, 0.1785465045940572426 ) ) ;
#35968 = AXIS2_PLACEMENT_3D ( 'NONE', #16001, #32416, #3246 ) ;
#35969 = CARTESIAN_POINT ( 'NONE',  ( -10.39199171643970665, 157.8614378686282862, 0.7539791864280581679 ) ) ;
#35970 = CARTESIAN_POINT ( 'NONE',  ( 20.08431799972932907, 128.8637844977697569, -0.1093955315764415515 ) ) ;
#35971 = DIRECTION ( 'NONE',  ( 5.463695987328526437E-16, 1.000000000000000000, 1.672774450599033775E-31 ) ) ;
#35972 = LINE ( 'NONE', #25738, #16769 ) ;
#35973 = CARTESIAN_POINT ( 'NONE',  ( -47.68734114412297487, 23.26096984540084023, 2.152999274035547472 ) ) ;
#35974 = DIRECTION ( 'NONE',  ( -0.000000000000000000, 1.000000000000000000, 0.000000000000000000 ) ) ;
#35975 = CARTESIAN_POINT ( 'NONE',  ( -56.26318288983030413, 4.268071985104968213, 2.480832006587838645 ) ) ;
#35976 = CARTESIAN_POINT ( 'NONE',  ( -58.74214995731320244, -0.3112433815685096139, 0.2392860922412864966 ) ) ;
#35977 = EDGE_CURVE ( 'NONE', #39412, #35748, #20924, .T. ) ;
#35978 = CARTESIAN_POINT ( 'NONE',  ( -4.662175683825617867, 118.0285603771968965, 0.5801233676060106870 ) ) ;
#35979 = DIRECTION ( 'NONE',  ( -0.8745520943968663197, 0.4849315768085789013, -5.691349986800499561E-16 ) ) ;
#35980 = EDGE_LOOP ( 'NONE', ( #21435, #16101, #40202, #9014 ) ) ;
#35981 = VERTEX_POINT ( 'NONE', #1579 ) ;
#35982 = CARTESIAN_POINT ( 'NONE',  ( -2.766040590020705903, 118.7629491485426172, -1.199722955718958151 ) ) ;
#35983 = VECTOR ( 'NONE', #3681, 1000.000000000000227 ) ;
#35984 = CARTESIAN_POINT ( 'NONE',  ( -8.379299793194181945, 119.6055850948818886, -1.415703317849449361 ) ) ;
#35985 = CARTESIAN_POINT ( 'NONE',  ( -5.227922695814451792, 116.4790307410953289, -1.091139864702252327 ) ) ;
#35986 = CARTESIAN_POINT ( 'NONE',  ( 4.571649082125946784, 118.0412581531131906, 0.8381018338667312051 ) ) ;
#35987 = AXIS2_PLACEMENT_3D ( 'NONE', #9072, #5048, #41239 ) ;
#35988 = CARTESIAN_POINT ( 'NONE',  ( -47.22545206610593027, 24.52529105818055655, -1.461865184087826286 ) ) ;
#35989 = CARTESIAN_POINT ( 'NONE',  ( -16.45678414710234350, 146.8700648836752691, -1.605370559133787900 ) ) ;
#35990 =( NAMED_UNIT ( * ) PLANE_ANGLE_UNIT ( ) SI_UNIT ( $, .RADIAN. ) );
#35991 = DIRECTION ( 'NONE',  ( 0.000000000000000000, 1.000000000000000000, 0.000000000000000000 ) ) ;
#35992 = CARTESIAN_POINT ( 'NONE',  ( 2.169980103648475378, 106.6933082031156772, -4.882050113528205948 ) ) ;
#35993 = CARTESIAN_POINT ( 'NONE',  ( -17.05487166051804593, 147.7912591418244403, -2.046378512860587584 ) ) ;
#35994 = EDGE_CURVE ( 'NONE', #23884, #19740, #2535, .T. ) ;
#35995 = CARTESIAN_POINT ( 'NONE',  ( -9.909999474182708212, 76.95545850745379823, 1.270000000000001350 ) ) ;
#35996 = CARTESIAN_POINT ( 'NONE',  ( -0.01645572339173941370, 159.4324016994384010, 0.8235116888278194436 ) ) ;
#35997 = CARTESIAN_POINT ( 'NONE',  ( 8.343164213270776841, 120.0286413096534233, -1.117317573728690894 ) ) ;
#35998 = CARTESIAN_POINT ( 'NONE',  ( -13.59213104125035265, 150.2515543379227267, -0.2066863870687406513 ) ) ;
#35999 = CARTESIAN_POINT ( 'NONE',  ( 3.746277899330032302, -0.8937244826341392834, -2.755274729908455900 ) ) ;
#36001 = VERTEX_POINT ( 'NONE', #15794 ) ;
#36000 = CARTESIAN_POINT ( 'NONE',  ( 22.98914810635003647, 149.5377445326608665, 1.186953142822410490 ) ) ;
#36002 = DIRECTION ( 'NONE',  ( 4.017660918040594346E-17, -1.000000000000000000, -2.376309959284834438E-19 ) ) ;
#36003 = CARTESIAN_POINT ( 'NONE',  ( 3.303734845180175128, -14.82389436555148166, -0.08037074644983704941 ) ) ;
#36004 = CARTESIAN_POINT ( 'NONE',  ( -4.252934711844699400, 157.4559852174668322, 1.675102021473321878 ) ) ;
#36005 = CARTESIAN_POINT ( 'NONE',  ( 0.04477287412000752198, 14.82196177864132380, -0.9729305925282246692 ) ) ;
#36006 = CARTESIAN_POINT ( 'NONE',  ( 0.004355829920540938045, 116.7171338949676738, -0.2179835409713597183 ) ) ;
#36007 = CARTESIAN_POINT ( 'NONE',  ( 0.03652159268533760467, -3.380040448513521589, 0.9750733386546841519 ) ) ;
#36008 = ORIENTED_EDGE ( 'NONE', *, *, #39378, .F. ) ;
#36009 = CARTESIAN_POINT ( 'NONE',  ( -45.11192300388035648, 21.16850173503701527, 3.873855239238726433 ) ) ;
#36010 = CARTESIAN_POINT ( 'NONE',  ( 4.757567707637461396, 116.6039038697339549, 1.126183464948452784 ) ) ;
#36011 = DIRECTION ( 'NONE',  ( 0.000000000000000000, 0.000000000000000000, 1.000000000000000000 ) ) ;
#36012 = CARTESIAN_POINT ( 'NONE',  ( -0.7306116569920545478, 156.4221767039705071, 0.6844267650493707222 ) ) ;
#36013 = CARTESIAN_POINT ( 'NONE',  ( 4.292324012607982908, -12.68181061970326340, 2.304565294163185118 ) ) ;
#36014 = CARTESIAN_POINT ( 'NONE',  ( 10.46700094992492680, 122.9580799906392343, -1.049763322952065536 ) ) ;
#36015 = CARTESIAN_POINT ( 'NONE',  ( -2.271387047179101337, 118.5910164976458532, -0.7981300483413859004 ) ) ;
#36016 = CARTESIAN_POINT ( 'NONE',  ( 2.781118144868611974, -14.77119122201073154, 4.489572933734862659 ) ) ;
#36017 = CARTESIAN_POINT ( 'NONE',  ( -3.328555392133317525, 33.88165127674241717, 1.160568618710268174 ) ) ;
#36018 = EDGE_CURVE ( 'NONE', #14494, #8692, #1860, .T. ) ;
#36019 = CARTESIAN_POINT ( 'NONE',  ( 0.003550340867663489587, 156.3099534201614631, -0.1776735749810080811 ) ) ;
#36020 = ORIENTED_EDGE ( 'NONE', *, *, #8709, .T. ) ;
#36021 = FACE_OUTER_BOUND ( 'NONE', #5909, .T. ) ;
#36022 = DIRECTION ( 'NONE',  ( -5.188838149069472160E-16, 1.699382548006136559E-16, 1.000000000000000000 ) ) ;
#36023 = EDGE_CURVE ( 'NONE', #20064, #4948, #4183, .T. ) ;
#36024 = TOROIDAL_SURFACE ( 'NONE', #19001, 5.080000000000005400, 0.5080000000000000071 ) ;
#36025 = DIRECTION ( 'NONE',  ( 0.9998004120163608288, 5.205824365704081956E-17, 0.01997839162482748995 ) ) ;
#36026 = ADVANCED_FACE ( 'NONE', ( #39023 ), #25644, .F. ) ;
#36027 = CARTESIAN_POINT ( 'NONE',  ( 10.28897677580358128, 57.14999999999999858, 5.016499999999999737 ) ) ;
#36028 = B_SPLINE_CURVE_WITH_KNOTS ( 'NONE', 3,
 ( #10236, #29630, #19810, #17044 ),
 .UNSPECIFIED., .F., .F.,
 ( 4, 4 ),
 ( -5.999999999756005006E-08, 0.0002276942339102930096 ),
 .UNSPECIFIED. ) ;
#36029 = CARTESIAN_POINT ( 'NONE',  ( 0.0008202526017140943961, 159.6052337359418800, -0.04104879434819951045 ) ) ;
#36030 = CARTESIAN_POINT ( 'NONE',  ( -5.774381877465555313, 118.4424948052634647, 0.4329097047088600325 ) ) ;
#36031 = CARTESIAN_POINT ( 'NONE',  ( -0.7418435039310978807, 115.6909491485452435, 1.732013647045983928 ) ) ;
#36032 = DIRECTION ( 'NONE',  ( 0.000000000000000000, 0.000000000000000000, 1.000000000000000000 ) ) ;
#36033 = CARTESIAN_POINT ( 'NONE',  ( 1.934221275448955391, 38.68736563468869605, -1.199403792597403706 ) ) ;
#36034 = CARTESIAN_POINT ( 'NONE',  ( 14.93032553133218521, 154.7288491705591866, 2.132398917750006895 ) ) ;
#36035 = CARTESIAN_POINT ( 'NONE',  ( -2.714482067202859561, 26.26591195808746448, -3.750338772627290762 ) ) ;
#36036 = CARTESIAN_POINT ( 'NONE',  ( -5.435345482397000438, 30.30303275347894854, -6.432456514813170045 ) ) ;
#36037 = CARTESIAN_POINT ( 'NONE',  ( 5.511471034203434094, 117.2322532230211749, -0.5987457750600796436 ) ) ;
#36038 = CARTESIAN_POINT ( 'NONE',  ( -1.549819036667766659, 118.0223913815010377, -1.039293717761402336 ) ) ;
#36039 = DIRECTION ( 'NONE',  ( 5.188838149069471174E-16, -1.699382548006136313E-16, -1.000000000000000000 ) ) ;
#36040 = CARTESIAN_POINT ( 'NONE',  ( -2.697694248221544022, 107.8416071541323049, -4.476792151442584355 ) ) ;
#36041 = CARTESIAN_POINT ( 'NONE',  ( 2.764046652421120243, 104.6144662015456959, 3.957270357869250521 ) ) ;
#36042 = CARTESIAN_POINT ( 'NONE',  ( 4.458631606973747274, 16.91056413504885825, 1.251853190366734259 ) ) ;
#36043 = CARTESIAN_POINT ( 'NONE',  ( -11.04921058900168873, 56.51499999999998636, -4.436160551868583823 ) ) ;
#36044 = CARTESIAN_POINT ( 'NONE',  ( -23.16987411132078734, 77.52691185402750307, 1.269999999999994245 ) ) ;
#36045 = CARTESIAN_POINT ( 'NONE',  ( 3.220330141560203696, -14.30903721375789317, 2.546581355196453345 ) ) ;
#36046 = B_SPLINE_CURVE_WITH_KNOTS ( 'NONE', 3,
 ( #34212, #17785, #37602, #36990 ),
 .UNSPECIFIED., .F., .F.,
 ( 4, 4 ),
 ( 0.000000000000000000, 1.000000000000000000 ),
 .UNSPECIFIED. ) ;
#36047 = CARTESIAN_POINT ( 'NONE',  ( 1.490732016122372716, 115.2915405621345144, -1.797152713846302818 ) ) ;
#36048 = CARTESIAN_POINT ( 'NONE',  ( -15.74805233917012437, 121.4292885696920621, 0.3002298764450370694 ) ) ;
#36049 = CARTESIAN_POINT ( 'NONE',  ( 4.922922108635476413, 117.4088122501876796, -0.9491512982636605145 ) ) ;
#36050 = ORIENTED_EDGE ( 'NONE', *, *, #3924, .F. ) ;
#36051 = DIRECTION ( 'NONE',  ( -5.463695987328526437E-16, -1.000000000000000000, -1.672774450599033775E-31 ) ) ;
#36052 = VECTOR ( 'NONE', #39787, 1000.000000000000000 ) ;
#36053 = ORIENTED_EDGE ( 'NONE', *, *, #36079, .T. ) ;
#36054 = DIRECTION ( 'NONE',  ( -1.000000000000000000, -6.353134868986659519E-16, 0.000000000000000000 ) ) ;
#36055 = CARTESIAN_POINT ( 'NONE',  ( 2.008732664060286055, -15.70244684250787870, 5.701976698490775597 ) ) ;
#36056 = CARTESIAN_POINT ( 'NONE',  ( -17.46960851010923577, 131.6241255656270255, 1.599527815159631938 ) ) ;
#36057 = CARTESIAN_POINT ( 'NONE',  ( 13.98214753592664827, 155.8415165211600595, -1.292431576881028832 ) ) ;
#36058 = CARTESIAN_POINT ( 'NONE',  ( 0.03997419820544263758, 30.08235846857972007, -0.9743396344490610206 ) ) ;
#36059 = CARTESIAN_POINT ( 'NONE',  ( -58.66492368201303975, -0.3142542598142069044, -0.3213541728213932802 ) ) ;
#36060 = EDGE_CURVE ( 'NONE', #26454, #500, #23596, .T. ) ;
#36061 = ORIENTED_EDGE ( 'NONE', *, *, #28465, .T. ) ;
#36062 = DIRECTION ( 'NONE',  ( 0.6825627711659039143, 0.7308269722843582228, 2.299753143848015941E-16 ) ) ;
#36063 = CARTESIAN_POINT ( 'NONE',  ( -0.1065646865916383690, 105.8844662015456919, 5.332932678536313809 ) ) ;
#36064 = SURFACE_SIDE_STYLE ('',( #26035 ) ) ;
#36065 = CARTESIAN_POINT ( 'NONE',  ( -0.008308630153272997601, 120.0570981805881559, 0.4157978282972241701 ) ) ;
#36066 = CARTESIAN_POINT ( 'NONE',  ( -18.27007371177421291, 83.88799758123168715, 1.269999999999994689 ) ) ;
#36067 = ADVANCED_FACE ( 'NONE', ( #25599 ), #41323, .T. ) ;
#36068 = CARTESIAN_POINT ( 'NONE',  ( 6.644289941094775109, 120.1594786313440011, -0.9502652795725030632 ) ) ;
#36069 = CARTESIAN_POINT ( 'NONE',  ( -2.160664645061537215, 117.9909145081919917, -0.7315704174731481046 ) ) ;
#36070 = CARTESIAN_POINT ( 'NONE',  ( -57.81953393267934160, 1.609514594907199392, -1.636666387507151432 ) ) ;
#36071 = VERTEX_POINT ( 'NONE', #54 ) ;
#36072 = CARTESIAN_POINT ( 'NONE',  ( 4.554969932097885810, 118.0892972403241430, -0.5841261413086886733 ) ) ;
#36073 = CARTESIAN_POINT ( 'NONE',  ( 13.80952258003148181, 150.2278160098252329, -0.4282869786672486856 ) ) ;
#36074 = EDGE_LOOP ( 'NONE', ( #39465, #35946, #9583, #6707 ) ) ;
#36075 = CARTESIAN_POINT ( 'NONE',  ( -6.563805965709591739, 120.5225452898634728, -1.124017915699711878 ) ) ;
#36076 = CARTESIAN_POINT ( 'NONE',  ( 3.373996639098103323, -14.83046237366941789, 1.396824179944331723 ) ) ;
#36077 = EDGE_CURVE ( 'NONE', #33817, #16319, #10688, .T. ) ;
#36078 = DIRECTION ( 'NONE',  ( 0.9998004120163610509, 4.016384292689131511E-17, 0.01997839162482749689 ) ) ;
#36079 = EDGE_CURVE ( 'NONE', #2275, #35679, #24272, .T. ) ;
#36080 = CARTESIAN_POINT ( 'NONE',  ( -43.13073682054402269, 20.84535665847938546, -6.630667737810475277E-15 ) ) ;
#36081 = CIRCLE ( 'NONE', #38779, 0.7620000000000000107 ) ;
#36082 = CARTESIAN_POINT ( 'NONE',  ( -2.972019672840211513, 9.848453565018933986, 3.538668892428941781 ) ) ;
#36083 = CARTESIAN_POINT ( 'NONE',  ( -0.009513407573742645174, 119.7614543879625586, 0.4760898169610157660 ) ) ;
#36084 = CARTESIAN_POINT ( 'NONE',  ( -2.651199864046426491, 30.19476482558288311, -0.03810942705075580361 ) ) ;
#36085 = EDGE_CURVE ( 'NONE', #12743, #24610, #20528, .T. ) ;
#36086 = CARTESIAN_POINT ( 'NONE',  ( 4.037907715354051241, 27.70556447992504445, -2.267523456217593214 ) ) ;
#36087 = CARTESIAN_POINT ( 'NONE',  ( 7.814053207647945420, 154.6216606121152495, 0.3474563751001367162 ) ) ;
#36088 = CARTESIAN_POINT ( 'NONE',  ( -2.959623698042840534, 107.4064645821210462, 4.429364252002888414 ) ) ;
#36089 = CARTESIAN_POINT ( 'NONE',  ( -56.36488200494262202, 4.056002992322685685, -2.423683632884288564 ) ) ;
#36090 = CARTESIAN_POINT ( 'NONE',  ( -5.562407735369682804, 116.6996333467663050, -0.1111501472963696002 ) ) ;
#36091 = CARTESIAN_POINT ( 'NONE',  ( -4.801770124281918406, 117.3993836135855133, 1.016061139389656587 ) ) ;
#36092 = CARTESIAN_POINT ( 'NONE',  ( -46.81779053729648865, 25.68675045694219250, -1.510149268906148867 ) ) ;
#36093 = DIRECTION ( 'NONE',  ( -0.8745520943968243532, 0.4849315768086547296, -6.829619984160642269E-16 ) ) ;
#36094 = CARTESIAN_POINT ( 'NONE',  ( -8.261285051657653256, 120.1778800549205073, -1.448705368892842849 ) ) ;
#36095 = CIRCLE ( 'NONE', #21857, 0.6350000000000008971 ) ;
#36096 = CARTESIAN_POINT ( 'NONE',  ( -25.97603047661466036, 74.27059221564131519, 1.269999999999992912 ) ) ;
#36097 = CARTESIAN_POINT ( 'NONE',  ( -4.074955089416341991, 118.2429491485453354, 0.1454234154749719787 ) ) ;
#36098 = CARTESIAN_POINT ( 'NONE',  ( -18.35410564743290962, 77.35382415001784295, -5.392902600000144986 ) ) ;
#36099 = CARTESIAN_POINT ( 'NONE',  ( -54.68578128246380743, 13.03233524003756472, 0.2705950194912850604 ) ) ;
#36100 = CARTESIAN_POINT ( 'NONE',  ( -56.21344593158320180, 5.939860726778031896, 2.828251681716853927 ) ) ;
#36101 = CARTESIAN_POINT ( 'NONE',  ( -21.87358050093881090, 151.4416708234707301, -0.1116233529550398618 ) ) ;
#36102 = EDGE_LOOP ( 'NONE', ( #20271, #8401, #27677, #6630, #24723 ) ) ;
#36103 = CARTESIAN_POINT ( 'NONE',  ( -51.68408071790322822, 18.36713515631302585, -1.546689197337258737 ) ) ;
#36104 = CARTESIAN_POINT ( 'NONE',  ( -6.979245073245229136, 121.9493068413915040, -0.1922076700199186194 ) ) ;
#36105 = EDGE_LOOP ( 'NONE', ( #21585, #40499, #5571, #24804 ) ) ;
#36106 = FACE_OUTER_BOUND ( 'NONE', #1997, .T. ) ;
#36108 = CARTESIAN_POINT ( 'NONE',  ( -15.37864313207211175, 147.8292851303062321, -0.3583584359702443045 ) ) ;
#36107 = CIRCLE ( 'NONE', #27247, 0.6349999999999971223 ) ;
#36109 = CARTESIAN_POINT ( 'NONE',  ( 2.081461833008368512, -15.42522581128935499, 5.972092850182497692 ) ) ;
#36110 = CARTESIAN_POINT ( 'NONE',  ( -13.46025642088320673, 121.5866728338796463, 1.110021706884414483 ) ) ;
#36111 = CARTESIAN_POINT ( 'NONE',  ( 4.300553167417687561, 27.50566818391071422, -1.719522505244270860 ) ) ;
#36112 = CARTESIAN_POINT ( 'NONE',  ( 7.991309159113032301, 158.6817341734954425, 0.4848270063548279496 ) ) ;
#36113 = CARTESIAN_POINT ( 'NONE',  ( 2.262096742913059622, -15.42953798115688535, 5.841406647620562609 ) ) ;
#36114 = DIRECTION ( 'NONE',  ( -1.000000000000000000, 0.000000000000000000, -5.975917486140574681E-16 ) ) ;
#36115 = CARTESIAN_POINT ( 'NONE',  ( 0.3393679441828953980, -8.777600141791896959, -0.9147772600509928020 ) ) ;
#36116 = CARTESIAN_POINT ( 'NONE',  ( -18.71175911766657762, 125.2636347375217838, -0.5504587009833170619 ) ) ;
#36117 = CYLINDRICAL_SURFACE ( 'NONE', #38598, 3.175000000000001155 ) ;
#36118 = DIRECTION ( 'NONE',  ( -1.000000000000000000, 1.893378931774809890E-16, 0.000000000000000000 ) ) ;
#36119 = ORIENTED_EDGE ( 'NONE', *, *, #27666, .F. ) ;
#36120 = CARTESIAN_POINT ( 'NONE',  ( -5.560790277979172025, 116.7475871101181895, 0.1053522238722745114 ) ) ;
#36121 = ORIENTED_EDGE ( 'NONE', *, *, #40493, .T. ) ;
#36122 = CARTESIAN_POINT ( 'NONE',  ( -7.412650754288892863, 120.7277362223577768, 0.9451843054385556941 ) ) ;
#36123 = CARTESIAN_POINT ( 'NONE',  ( -5.451267667241070720E-14, 85.80437499999999318, 0.000000000000000000 ) ) ;
#36124 = CARTESIAN_POINT ( 'NONE',  ( 14.96081243412104200, 123.1914926142276130, 1.724312424550131784 ) ) ;
#36125 = CARTESIAN_POINT ( 'NONE',  ( 15.81176147471969529, 128.5598958631237565, -1.562949982248214242 ) ) ;
#36126 = CARTESIAN_POINT ( 'NONE',  ( 0.9435450883166688341, 2.505659174922684418, 0.2465458143858453577 ) ) ;
#36127 = CARTESIAN_POINT ( 'NONE',  ( -21.97492997894005029, 149.1257232373000647, -2.026018130409337648 ) ) ;
#36128 = CARTESIAN_POINT ( 'NONE',  ( 4.678169868823534472, 118.0125419685739416, -0.6044271497212726496 ) ) ;
#36129 = CARTESIAN_POINT ( 'NONE',  ( 5.487604538598316317, 117.4962825466697467, 0.8290304003371103958 ) ) ;
#36130 = CARTESIAN_POINT ( 'NONE',  ( 16.34996387626492620, 143.9496486471311698, -1.129508837753296469 ) ) ;
#36131 = CARTESIAN_POINT ( 'NONE',  ( -7.044606587285223931, 122.0729346620515088, -0.1407680048458704314 ) ) ;
#36132 = ORIENTED_EDGE ( 'NONE', *, *, #16999, .T. ) ;
#36133 = CARTESIAN_POINT ( 'NONE',  ( -1.321503922127654551, 119.3298839580929638, -0.6528639922554045905 ) ) ;
#36134 = CARTESIAN_POINT ( 'NONE',  ( 3.743762692837560468, -15.60843739440008449, 4.988928788737716502 ) ) ;
#36135 = FACE_OUTER_BOUND ( 'NONE', #30077, .T. ) ;
#36136 = CIRCLE ( 'NONE', #40864, 0.5080000000000002292 ) ;
#36137 = EDGE_CURVE ( 'NONE', #20165, #11776, #22919, .T. ) ;
#36138 = CARTESIAN_POINT ( 'NONE',  ( -44.40534991575952972, 23.82367036525651116, -1.730788704199199834 ) ) ;
#36139 = CARTESIAN_POINT ( 'NONE',  ( 16.38646240326715287, 135.1966315799913900, 2.295807278541857954 ) ) ;
#36140 = CARTESIAN_POINT ( 'NONE',  ( -5.176850267262477878, 31.60528704468920580, -0.07969122161898606338 ) ) ;
#36141 = EDGE_CURVE ( 'NONE', #24583, #25879, #12410, .T. ) ;
#36142 = CIRCLE ( 'NONE', #2113, 5.588000000000006295 ) ;
#36143 = DIRECTION ( 'NONE',  ( -6.853480209240093652E-32, -1.000000000000000000, 3.905054717696927820E-31 ) ) ;
#36144 = CARTESIAN_POINT ( 'NONE',  ( -5.582679110870683026, 119.7830797108918688, 0.2735363082852449446 ) ) ;
#36145 = CARTESIAN_POINT ( 'NONE',  ( 2.403447530314441583, 28.79142288871172539, -8.109455235164826803 ) ) ;
#36146 = CARTESIAN_POINT ( 'NONE',  ( 5.883037304650295063, 121.3687970875902806, 0.4830333308872108433 ) ) ;
#36147 = CARTESIAN_POINT ( 'NONE',  ( 11.36388202081341170, 118.9804978796424706, -0.4533785775503093030 ) ) ;
#36148 = CARTESIAN_POINT ( 'NONE',  ( 5.339080835687772364, 115.7029491485453150, -0.2011480626654460757 ) ) ;
#36149 = CARTESIAN_POINT ( 'NONE',  ( -25.83700401581416983, 71.09321415394998667, -1.270000000000005347 ) ) ;
#36150 = CARTESIAN_POINT ( 'NONE',  ( -13.43647848967396818, 156.9186530619738562, -0.2471310363275582567 ) ) ;
#36151 = ORIENTED_EDGE ( 'NONE', *, *, #7690, .T. ) ;
#36152 = CARTESIAN_POINT ( 'NONE',  ( 8.061888348283327232, 121.3793065287195958, -0.9018960436474696696 ) ) ;
#36153 = CARTESIAN_POINT ( 'NONE',  ( 6.309668351831440702, -13.80474515357695076, 1.045049453412914664 ) ) ;
#36154 = CARTESIAN_POINT ( 'NONE',  ( -7.919085485410461089, 154.5997988942315260, -0.6546929905378091608 ) ) ;
#36155 = CARTESIAN_POINT ( 'NONE',  ( 2.780001287168888613, -14.74817992026429536, 5.465600930587551254 ) ) ;
#36156 = CARTESIAN_POINT ( 'NONE',  ( -3.950580610161007922, 117.4679918459733585, 0.5815556119072164964 ) ) ;
#36157 = CARTESIAN_POINT ( 'NONE',  ( -10.93398011767285283, 82.89560043784887000, -1.269999999999999352 ) ) ;
#36158 = AXIS2_PLACEMENT_3D ( 'NONE', #40527, #8557, #21729 ) ;
#36159 = CARTESIAN_POINT ( 'NONE',  ( 8.215520591712387244, 117.5015518944296247, 0.2087872862963604248 ) ) ;
#36160 = ORIENTED_EDGE ( 'NONE', *, *, #8614, .F. ) ;
#36161 = CARTESIAN_POINT ( 'NONE',  ( -2.424025297795170619, -5.104216246930970868, 3.935102955759355758 ) ) ;
#36162 = CARTESIAN_POINT ( 'NONE',  ( -22.76738278397264281, 137.3906169244638136, -0.4549464913834382340 ) ) ;
#36163 = CARTESIAN_POINT ( 'NONE',  ( 3.682264917456193221, 78.32546620154573702, 0.07358041635424013294 ) ) ;
#36164 = DIRECTION ( 'NONE',  ( -5.188838149069472160E-16, 1.699382548006136559E-16, 1.000000000000000000 ) ) ;
#36165 = CARTESIAN_POINT ( 'NONE',  ( 7.799194557895424929, 122.5298883528417662, 0.4369513083720456548 ) ) ;
#36166 = CARTESIAN_POINT ( 'NONE',  ( 4.099978103716023448, 4.450953565018914482, -2.131961072590273343 ) ) ;
#36167 = CARTESIAN_POINT ( 'NONE',  ( 13.61640385012393928, 120.8017016962898396, 1.366196570323218396 ) ) ;
#36168 = DIRECTION ( 'NONE',  ( -4.017660918040594346E-17, 1.000000000000000000, 2.376309959284834438E-19 ) ) ;
#36170 = CARTESIAN_POINT ( 'NONE',  ( 20.47035330145901000, 150.0074677946399504, -1.517022030030164892 ) ) ;
#36169 = CARTESIAN_POINT ( 'NONE',  ( 6.059261036834406866, 56.51500000000000057, 4.381500000000000838 ) ) ;
#36171 = TOROIDAL_SURFACE ( 'NONE', #27308, 8.794749999999996959, 0.2540000000000000036 ) ;
#36172 = CARTESIAN_POINT ( 'NONE',  ( 0.7003524534433175353, 11.14785949628657669, 4.567531960304466843 ) ) ;
#36173 = CARTESIAN_POINT ( 'NONE',  ( -13.03166249679917321, 119.8917521002241955, -1.045815086349644707 ) ) ;
#36174 = ORIENTED_EDGE ( 'NONE', *, *, #37572, .T. ) ;
#36175 = CARTESIAN_POINT ( 'NONE',  ( -8.112862105099743815, 122.9271997657465931, -0.1621142923986426398 ) ) ;
#36176 = CARTESIAN_POINT ( 'NONE',  ( -6.492420186392395820, 121.7431354732680973, 0.05225946255319178363 ) ) ;
#36177 = CARTESIAN_POINT ( 'NONE',  ( 4.721559244837001401, -14.40436002768456802, 4.408607674763740825 ) ) ;
#36178 = CARTESIAN_POINT ( 'NONE',  ( -46.76714659696573051, 20.35889133747190272, 4.890039387020951089 ) ) ;
#36179 = CARTESIAN_POINT ( 'NONE',  ( -1.187539700871899528, 106.2993931590553274, -5.152244660853054548 ) ) ;
#36180 = EDGE_LOOP ( 'NONE', ( #31711, #30321, #36902, #39982 ) ) ;
#36181 = CARTESIAN_POINT ( 'NONE',  ( 7.606098120226983283, 119.7866739149480253, 1.386975461113101771 ) ) ;
#36182 = CARTESIAN_POINT ( 'NONE',  ( -18.35410564743290962, 77.35382415001784295, 5.392902600000138769 ) ) ;
#36183 = CARTESIAN_POINT ( 'NONE',  ( 11.82813386268891165, 130.3161362890850512, 0.2363542639706544268 ) ) ;
#36184 = VECTOR ( 'NONE', #205, 1000.000000000000000 ) ;
#36185 = EDGE_CURVE ( 'NONE', #6464, #11324, #28592, .T. ) ;
#36186 = CARTESIAN_POINT ( 'NONE',  ( -14.76838793310970388, 156.1040168620350244, 0.6600470674582795683 ) ) ;
#36187 = CARTESIAN_POINT ( 'NONE',  ( -7.601118931484537100, 27.11072341857771306, -3.643763446188946542 ) ) ;
#36188 = CARTESIAN_POINT ( 'NONE',  ( 7.966904459259814608, 158.6775731370129279, -0.2701962758350452964 ) ) ;
#36189 = CARTESIAN_POINT ( 'NONE',  ( -5.511339492779010030, 57.15000000000000568, -5.111277471990291588 ) ) ;
#36190 = CARTESIAN_POINT ( 'NONE',  ( -50.89935680924180161, 14.64024222003797426, 4.571006890225723929 ) ) ;
#36191 = CARTESIAN_POINT ( 'NONE',  ( -49.70354155341430413, 23.42381788805148091, -9.364162196477891358E-15 ) ) ;
#36192 = CARTESIAN_POINT ( 'NONE',  ( 2.026452703349827633, -15.26483848100516916, 5.365780487320932934 ) ) ;
#36193 = CARTESIAN_POINT ( 'NONE',  ( -50.78166962549567387, 16.07998339508975860, 4.893817234114164805 ) ) ;
#36194 = DIRECTION ( 'NONE',  ( -0.6850534820564617711, 0.7284927773988681965, -8.537024980200850414E-16 ) ) ;
#36195 = CARTESIAN_POINT ( 'NONE',  ( -4.414199990641388460, 118.1799141087742555, 0.3933343983828669899 ) ) ;
#36196 = CARTESIAN_POINT ( 'NONE',  ( -6.059261036834082681, 78.87450423423038615, -5.016499999999999737 ) ) ;
#36197 = ORIENTED_EDGE ( 'NONE', *, *, #40973, .F. ) ;
#36198 = CARTESIAN_POINT ( 'NONE',  ( -46.31144060707497090, 24.05480373873685451, 2.308638262703916588 ) ) ;
#36199 = CARTESIAN_POINT ( 'NONE',  ( -8.302816400183525403, 119.9753945280262712, -1.448211312683703955 ) ) ;
#36200 = CARTESIAN_POINT ( 'NONE',  ( -6.287821989302600834, 120.0808430858776887, -0.4528678087849540845 ) ) ;
#36201 = CARTESIAN_POINT ( 'NONE',  ( 4.512686109237062482, 118.0696626847395976, 0.8150047576444854336 ) ) ;
#36202 = CARTESIAN_POINT ( 'NONE',  ( -15.88363809060984799, 147.6644253265642135, -1.281895537487840464 ) ) ;
#36203 = CARTESIAN_POINT ( 'NONE',  ( -2.438095677481897816, 115.7029724308332277, -1.698769770220674102 ) ) ;
#36204 = DIRECTION ( 'NONE',  ( 5.188838149069472160E-16, -1.699382548006136559E-16, -1.000000000000000000 ) ) ;
#36205 = CARTESIAN_POINT ( 'NONE',  ( 1.576215671565278864, 106.2483430537416638, -5.109971884176318646 ) ) ;
#36206 = CARTESIAN_POINT ( 'NONE',  ( -16.09426298050584947, 139.8573806175465961, -2.037321532313223660 ) ) ;
#36207 = CARTESIAN_POINT ( 'NONE',  ( -24.32950799593924884, 77.42192949967211746, 1.269999999999993578 ) ) ;
#36208 = CARTESIAN_POINT ( 'NONE',  ( -0.03212618750959882197, 158.2819368290249713, 1.607725792532325393 ) ) ;
#36209 = CARTESIAN_POINT ( 'NONE',  ( 8.036149603167988431, 121.5005262100066830, -0.8572904197356677747 ) ) ;
#36210 = CARTESIAN_POINT ( 'NONE',  ( -15.26612506134334524, 148.0236973083020473, -0.1719504695324379495 ) ) ;
#36211 = EDGE_CURVE ( 'NONE', #24610, #3481, #12915, .T. ) ;
#36212 = CARTESIAN_POINT ( 'NONE',  ( 1.686640475165922748, -9.627085671684914914, -4.319569293544198274 ) ) ;
#36213 = CARTESIAN_POINT ( 'NONE',  ( 0.3250403508452471835, 116.7787044104018861, 0.2632219653755004107 ) ) ;
#36214 = CARTESIAN_POINT ( 'NONE',  ( -6.474089935681887051E-14, 69.94346620154573202, 3.752704589293910110E-29 ) ) ;
#36215 = CARTESIAN_POINT ( 'NONE',  ( 3.406014632911877893, -14.97454077108105430, 2.395711393442250259 ) ) ;
#36216 = CARTESIAN_POINT ( 'NONE',  ( -18.78250995143904234, 149.1225091032880528, 1.736135053443003784 ) ) ;
#36217 = CARTESIAN_POINT ( 'NONE',  ( 0.8366737682863060188, 2.078006455476229419, 0.4978880095337852585 ) ) ;
#36218 = CARTESIAN_POINT ( 'NONE',  ( -11.50728102546042031, 118.8226552325407397, -0.6924515317502045741 ) ) ;
#36219 = CIRCLE ( 'NONE', #37571, 0.2540000000000015579 ) ;
#36220 = CARTESIAN_POINT ( 'NONE',  ( -0.1630216852218501489, 24.74361041950371032, -0.9604350664704873752 ) ) ;
#36221 = ORIENTED_EDGE ( 'NONE', *, *, #10010, .T. ) ;
#36222 = CARTESIAN_POINT ( 'NONE',  ( -46.36222913602040308, 19.75614878210438263, 3.583538483381419670 ) ) ;
#36223 = CARTESIAN_POINT ( 'NONE',  ( 5.210481185491484979, 116.4925209815607730, 1.089480302653437871 ) ) ;
#36224 = CARTESIAN_POINT ( 'NONE',  ( -15.65625195688312843, 148.1291547725267037, 0.6483782694814675951 ) ) ;
#36225 = CARTESIAN_POINT ( 'NONE',  ( 3.965039388734942882, -13.93407386435618989, 4.333124597978631698 ) ) ;
#36226 = CARTESIAN_POINT ( 'NONE',  ( 11.97328186178008380, 153.4554508723442439, -1.471200310048991433 ) ) ;
#36227 = CARTESIAN_POINT ( 'NONE',  ( -5.837434872615095749, 119.2401804501882197, -1.198870938642750739 ) ) ;
#36228 = CARTESIAN_POINT ( 'NONE',  ( -6.529493367164978770E-14, 72.99146620154573384, -7.899616498973244731E-18 ) ) ;
#36229 = ADVANCED_FACE ( 'NONE', ( #33056, #10880 ), #13661, .F. ) ;
#36230 = CARTESIAN_POINT ( 'NONE',  ( 2.904419875024614850, -13.46177902185440090, 0.8499660341922408158 ) ) ;
#36231 = CARTESIAN_POINT ( 'NONE',  ( -6.444213031565760197, 30.20499910742390881, -0.3026784529137391822 ) ) ;
#36232 = CARTESIAN_POINT ( 'NONE',  ( 8.581106358026191927, 123.3373102669514765, 0.01935445114830166430 ) ) ;
#36233 = CIRCLE ( 'NONE', #33519, 0.7620000000000015650 ) ;
#36234 = ORIENTED_EDGE ( 'NONE', *, *, #31090, .F. ) ;
#36235 = CARTESIAN_POINT ( 'NONE',  ( -3.041852915713540551, 107.5205933461800640, 4.373098560481015085 ) ) ;
#36236 = CARTESIAN_POINT ( 'NONE',  ( -0.1058213901579904276, 105.9761915687788587, 5.295735085525931751 ) ) ;
#36237 = CARTESIAN_POINT ( 'NONE',  ( 18.35410564743290607, 77.35382415001784295, 5.016499999999999737 ) ) ;
#36238 = B_SPLINE_CURVE_WITH_KNOTS ( 'NONE', 3,
 ( #35533, #9128, #12730, #25719 ),
 .UNSPECIFIED., .F., .F.,
 ( 4, 4 ),
 ( 0.000000000000000000, 0.5643836377221552736 ),
 .UNSPECIFIED. ) ;
#36239 = CYLINDRICAL_SURFACE ( 'NONE', #13650, 6.350000000000004974 ) ;
#36240 = EDGE_CURVE ( 'NONE', #4992, #30709, #23650, .T. ) ;
#36241 = CARTESIAN_POINT ( 'NONE',  ( 0.9075203043613222498, 116.4850453793277865, -0.07935580435194640458 ) ) ;
#36242 = CARTESIAN_POINT ( 'NONE',  ( -2.177262389793364061, 106.6864334246082961, 4.884315812310542348 ) ) ;
#36243 = AXIS2_PLACEMENT_3D ( 'NONE', #20559, #35356, #33588 ) ;
#36244 = CARTESIAN_POINT ( 'NONE',  ( -0.8426312062438860995, 115.6909491485452435, 1.724999377526929889 ) ) ;
#36245 = CARTESIAN_POINT ( 'NONE',  ( -1.217056272985401533, 34.90614901474430098, 0.2337217464280959833 ) ) ;
#36246 = CARTESIAN_POINT ( 'NONE',  ( 16.44465323483251495, 153.5550899668227203, 2.240181424793372678 ) ) ;
#36247 = CARTESIAN_POINT ( 'NONE',  ( 4.064150447026247726, 23.66704930264554818, -2.198397014704132513 ) ) ;
#36248 = CARTESIAN_POINT ( 'NONE',  ( 8.243228241119590294, 17.55835651096333194, -1.765626013165721320 ) ) ;
#36249 = CARTESIAN_POINT ( 'NONE',  ( 2.354862059299378085, 117.2183826610675652, -0.5773916514328522043 ) ) ;
#36250 = CARTESIAN_POINT ( 'NONE',  ( 0.1065646865915095137, 105.8844662015456777, -5.332932678536313809 ) ) ;
#36251 = DIRECTION ( 'NONE',  ( 5.188838149069472160E-16, -1.699382548006136559E-16, -1.000000000000000000 ) ) ;
#36252 = CARTESIAN_POINT ( 'NONE',  ( -10.63219908769152866, 56.50600268266023107, -5.016499999999338932 ) ) ;
#36253 = CARTESIAN_POINT ( 'NONE',  ( -1.940427529279133090, 104.6144662015434648, 4.971597247601878600 ) ) ;
#36254 = CIRCLE ( 'NONE', #2931, 0.2539999999999998925 ) ;
#36255 = CARTESIAN_POINT ( 'NONE',  ( 2.584458374606236841, 15.83607344512877368, 3.832284875798456447 ) ) ;
#36256 = CARTESIAN_POINT ( 'NONE',  ( -47.02779878473986486, 24.11651466984139702, -2.637840241488492943 ) ) ;
#36257 = CARTESIAN_POINT ( 'NONE',  ( -23.42514220145546133, 142.8382549600663083, -0.4680900899251589919 ) ) ;
#36258 = CARTESIAN_POINT ( 'NONE',  ( 3.171691571413298050, -13.57474810710837509, 1.775319381694977716 ) ) ;
#36259 = EDGE_CURVE ( 'NONE', #13978, #2010, #3227, .T. ) ;
#36260 = CARTESIAN_POINT ( 'NONE',  ( 1.603046668355785132, 118.6366899268033279, -0.8036507178775275095 ) ) ;
#36261 = CARTESIAN_POINT ( 'NONE',  ( -18.27977197196865689, 154.1370782493726210, 0.5456809356757471585 ) ) ;
#36262 = CIRCLE ( 'NONE', #23308, 0.3810000000000015041 ) ;
#36263 = CARTESIAN_POINT ( 'NONE',  ( 4.854507468356392685, 117.4057973178051526, -0.9983053292619181729 ) ) ;
#36264 = ORIENTED_EDGE ( 'NONE', *, *, #16689, .F. ) ;
#36265 = DIRECTION ( 'NONE',  ( -0.01731298258488772612, 0.9998501190848633202, -1.788962107505314604E-16 ) ) ;
#36266 =( BOUNDED_CURVE ( )  B_SPLINE_CURVE ( 3, ( #2647, #28824, #28405, #35225 ),
 .UNSPECIFIED., .F., .F. ) 
 B_SPLINE_CURVE_WITH_KNOTS ( ( 4, 4 ),
 ( 0.6038647612415126709, 0.6486116422890977340 ),
 .UNSPECIFIED. ) 
 CURVE ( )  GEOMETRIC_REPRESENTATION_ITEM ( )  RATIONAL_B_SPLINE_CURVE ( ( 0.6708440640561601498, 0.6359688846130079343, 0.6064331274724894527, 0.5822367926346048161 ) ) 
 REPRESENTATION_ITEM ( '' )  );
#36267 = ORIENTED_EDGE ( 'NONE', *, *, #38941, .F. ) ;
#36268 = CARTESIAN_POINT ( 'NONE',  ( 1.957912617769093755, 35.96399040732271857, -0.5992445403938203574 ) ) ;
#36269 = CARTESIAN_POINT ( 'NONE',  ( 2.867278011408870064, -15.71882806570827640, 4.918777663456151750 ) ) ;
#36270 = CARTESIAN_POINT ( 'NONE',  ( -13.96578288426892911, 123.5874490550988014, 1.342688313448305637 ) ) ;
#36271 = CARTESIAN_POINT ( 'NONE',  ( 16.82967018813376825, 125.2521365416322254, -1.031881933595589995 ) ) ;
#36272 = CARTESIAN_POINT ( 'NONE',  ( 3.315635589170360831, -10.27688868798473720, -3.234826238065521053 ) ) ;
#36273 = CARTESIAN_POINT ( 'NONE',  ( -58.63359593288674887, -0.2965917858236741256, -0.3663021125533588163 ) ) ;
#36274 = VERTEX_POINT ( 'NONE', #16851 ) ;
#36275 = DIRECTION ( 'NONE',  ( -5.188838149069472160E-16, 1.699382548006136559E-16, 1.000000000000000000 ) ) ;
#36276 = CARTESIAN_POINT ( 'NONE',  ( 0.9836305199213740691, 123.5966405200008325, 0.1412250206608575975 ) ) ;
#36277 = CARTESIAN_POINT ( 'NONE',  ( -6.842818979164508875, 155.5980657034081105, 1.215443052661050682 ) ) ;
#36278 = CARTESIAN_POINT ( 'NONE',  ( -6.069968983247740368, 28.54777132941064721, 0.2584723001727267100 ) ) ;
#36279 = CARTESIAN_POINT ( 'NONE',  ( 18.38987645279111405, 147.6341482083243761, -1.661003423535650336 ) ) ;
#36280 = AXIS2_PLACEMENT_3D ( 'NONE', #9940, #29550, #32526 ) ;
#36281 = CARTESIAN_POINT ( 'NONE',  ( -10.46214381725873288, 120.0128241960130424, -1.483189230905844536 ) ) ;
#36282 = CARTESIAN_POINT ( 'NONE',  ( 4.854633716284414646, 115.7029491485453292, -1.279498648767039448 ) ) ;
#36283 = CIRCLE ( 'NONE', #17881, 3.683000000000001162 ) ;
#36284 = ORIENTED_EDGE ( 'NONE', *, *, #15270, .F. ) ;
#36285 = CARTESIAN_POINT ( 'NONE',  ( 4.401957988103021968, 118.1614069291599520, -0.4937243125134848087 ) ) ;
#36286 = CARTESIAN_POINT ( 'NONE',  ( 0.004350076772657346554, 120.7058980590201429, -0.2176956299261766647 ) ) ;
#36287 = VERTEX_POINT ( 'NONE', #7704 ) ;
#36288 = CARTESIAN_POINT ( 'NONE',  ( -11.20916139128205025, 123.4744472594011739, -1.589032359792267535 ) ) ;
#36289 = CARTESIAN_POINT ( 'NONE',  ( 3.154745640343158630, -14.88448557395780014, 3.454683184413806174 ) ) ;
#36290 = CARTESIAN_POINT ( 'NONE',  ( -5.332935397695336199, 105.1224662015457199, -0.1065647409268299373 ) ) ;
#36291 = AXIS2_PLACEMENT_3D ( 'NONE', #23378, #33214, #17001 ) ;
#36292 = CARTESIAN_POINT ( 'NONE',  ( -58.34514637059943709, -0.2398883667947132592, 0.1955437934783506304 ) ) ;
#36293 = EDGE_CURVE ( 'NONE', #16976, #5996, #14093, .T. ) ;
#36294 = CARTESIAN_POINT ( 'NONE',  ( -1.441504266290200897, 6.599927940091079748, -4.410093354674724964 ) ) ;
#36295 = CARTESIAN_POINT ( 'NONE',  ( 7.123980356063992048, 155.7895407640516510, 1.727872795330590128 ) ) ;
#36296 = CARTESIAN_POINT ( 'NONE',  ( -2.965274000540799815, 30.81687845933373637, 0.1006152140846759829 ) ) ;
#36297 = CARTESIAN_POINT ( 'NONE',  ( 0.6590154617207463206, 19.50938314818779062, -4.574821423538240950 ) ) ;
#36298 = CARTESIAN_POINT ( 'NONE',  ( 9.673174862101884486, 124.8500477395539576, 0.3609973675953366268 ) ) ;
#36299 = DIRECTION ( 'NONE',  ( -5.188838149069472160E-16, 1.699382548006136559E-16, 1.000000000000000000 ) ) ;
#36300 = ADVANCED_FACE ( 'NONE', ( #19825 ), #33269, .T. ) ;
#36301 = CARTESIAN_POINT ( 'NONE',  ( -54.22787649382022579, 6.886497292746652121, -0.2709450413641087407 ) ) ;
#36302 = CARTESIAN_POINT ( 'NONE',  ( 5.554579209606487211, 116.7832337216378562, -0.2016058634275091077 ) ) ;
#36303 = CARTESIAN_POINT ( 'NONE',  ( 5.757472737270592944, 159.1136035536173097, 0.1150480073142623738 ) ) ;
#36304 = CIRCLE ( 'NONE', #10448, 6.350000000000004974 ) ;
#36305 = CARTESIAN_POINT ( 'NONE',  ( -23.36555825341177339, 148.7788340588663800, -0.4668994608413308267 ) ) ;
#36306 = DIRECTION ( 'NONE',  ( 4.017660918040594346E-17, -1.000000000000000000, -2.376309959284832031E-19 ) ) ;
#36307 = CARTESIAN_POINT ( 'NONE',  ( -33.42971872652992005, 49.93539301574497102, -1.270000000000005569 ) ) ;
#36308 = FACE_OUTER_BOUND ( 'NONE', #19675, .T. ) ;
#36309 = DIRECTION ( 'NONE',  ( 5.188838149069472160E-16, -1.699382548006136559E-16, -1.000000000000000000 ) ) ;
#36310 = CARTESIAN_POINT ( 'NONE',  ( -6.373576640880495633E-14, 50.63946620154572997, 5.832708929232124832E-29 ) ) ;
#36311 = CARTESIAN_POINT ( 'NONE',  ( -57.90853684698416259, 2.514838786807804816, -1.057700776740060064E-14 ) ) ;
#36312 = CARTESIAN_POINT ( 'NONE',  ( -57.85534701229748578, 0.8496279762696679061, 1.203237356453206619 ) ) ;
#36313 = CARTESIAN_POINT ( 'NONE',  ( -14.60357043488722439, 120.3300541288867862, 0.1192926189779472401 ) ) ;
#36314 = AXIS2_PLACEMENT_3D ( 'NONE', #5069, #2072, #18022 ) ;
#36315 = ORIENTED_EDGE ( 'NONE', *, *, #40967, .F. ) ;
#36316 = CARTESIAN_POINT ( 'NONE',  ( -56.03617394834085985, 6.499552843647532718, -2.676235688315271588 ) ) ;
#36317 = CARTESIAN_POINT ( 'NONE',  ( -7.790776616239916130, 122.5816380323567927, -0.3271574360425709704 ) ) ;
#36318 = ADVANCED_FACE ( 'NONE', ( #39230 ), #41293, .F. ) ;
#36319 = ORIENTED_EDGE ( 'NONE', *, *, #40180, .T. ) ;
#36320 = CARTESIAN_POINT ( 'NONE',  ( 4.854633716284414646, 115.7029491485453292, -1.279498648767039448 ) ) ;
#36321 = CARTESIAN_POINT ( 'NONE',  ( -11.85559104777375872, 130.3381101163291760, -0.2804367443601420984 ) ) ;
#36322 = CARTESIAN_POINT ( 'NONE',  ( 5.858142917232623148, -13.84584594667595603, 2.526540219170608115 ) ) ;
#36323 = CARTESIAN_POINT ( 'NONE',  ( -21.36781924117701337, 148.2102652567764380, 1.461444809879598239 ) ) ;
#36324 = CARTESIAN_POINT ( 'NONE',  ( -1.648064503646425649, 29.87956589480163316, -4.325937074807028715 ) ) ;
#36325 = AXIS2_PLACEMENT_3D ( 'NONE', #15726, #35137, #40899 ) ;
#36326 = CARTESIAN_POINT ( 'NONE',  ( 22.45364888651499768, 150.7739627601066275, 0.8979154079963821422 ) ) ;
#36327 = EDGE_CURVE ( 'NONE', #22227, #25505, #33180, .T. ) ;
#36328 = CARTESIAN_POINT ( 'NONE',  ( 2.000623374115709563, -15.62324522779390179, 5.905393795144921576 ) ) ;
#36329 = DIRECTION ( 'NONE',  ( -0.8745520943968354555, 0.4849315768086345235, -6.829619984160664949E-16 ) ) ;
#36330 = CARTESIAN_POINT ( 'NONE',  ( 0.5759086045921885111, -9.199343823100290862, -0.7873135961421041662 ) ) ;
#36331 = CARTESIAN_POINT ( 'NONE',  ( -15.84538651563812195, 121.0146182718019645, -0.4760991727851860977 ) ) ;
#36332 = CARTESIAN_POINT ( 'NONE',  ( -11.04921058900168873, 56.51499999999998636, 4.436160551868583823 ) ) ;
#36333 = FACE_OUTER_BOUND ( 'NONE', #34164, .T. ) ;
#36334 = CARTESIAN_POINT ( 'NONE',  ( -2.230307283400940310, 116.2698154044227294, 0.08777694382101131065 ) ) ;
#36335 = EDGE_LOOP ( 'NONE', ( #40060, #41528 ) ) ;
#36336 = CARTESIAN_POINT ( 'NONE',  ( -7.451643811072202084, 155.9567503867590972, 1.565497431107724102 ) ) ;
#36337 = CARTESIAN_POINT ( 'NONE',  ( -57.93467410668397122, 0.6461773018132880297, -0.9430256072699126912 ) ) ;
#36338 = CARTESIAN_POINT ( 'NONE',  ( 20.57609261220299501, 150.0789294893613999, 2.287104906598478316 ) ) ;
#36339 = CARTESIAN_POINT ( 'NONE',  ( 17.13393749618825268, 131.5760549582342094, -1.627836260134054580 ) ) ;
#36340 = AXIS2_PLACEMENT_3D ( 'NONE', #17085, #23893, #10695 ) ;
#36341 = CARTESIAN_POINT ( 'NONE',  ( -0.1338072975148606736, -13.68656151007796495, -0.9662261747338762863 ) ) ;
#36342 = CARTESIAN_POINT ( 'NONE',  ( -22.03849170948991443, 148.8299554149626260, -2.028895537808247607 ) ) ;
#36343 = CARTESIAN_POINT ( 'NONE',  ( 4.643821608714259419, 118.0368167649473747, -0.6067757769337593921 ) ) ;
#36344 = CARTESIAN_POINT ( 'NONE',  ( -3.009276887026424152, 50.42904571186020490, 1.210121013456479933 ) ) ;
#36345 = CARTESIAN_POINT ( 'NONE',  ( 11.42136869062004756, 126.1532465342912985, -0.7903108812046735210 ) ) ;
#36346 = EDGE_CURVE ( 'NONE', #19493, #9538, #35211, .T. ) ;
#36347 = CARTESIAN_POINT ( 'NONE',  ( -15.78598348091628267, 146.2390805666957192, -0.2639793761055730381 ) ) ;
#36348 = ORIENTED_EDGE ( 'NONE', *, *, #28571, .F. ) ;
#36349 = CARTESIAN_POINT ( 'NONE',  ( -14.78649082109382640, 128.5561590274816126, -2.111834004041170498 ) ) ;
#36350 = CARTESIAN_POINT ( 'NONE',  ( 4.512673509771836677, -15.64532105467335299, 2.834742450761120303 ) ) ;
#36351 = AXIS2_PLACEMENT_3D ( 'NONE', #38801, #12804, #35824 ) ;
#36352 = CARTESIAN_POINT ( 'NONE',  ( -58.83227707057486811, -0.08366279997995551554, -1.529465441686574059E-14 ) ) ;
#36353 = CARTESIAN_POINT ( 'NONE',  ( -4.648568650443571926, 118.0134285438809911, -0.7934044273710590955 ) ) ;
#36354 = CARTESIAN_POINT ( 'NONE',  ( -55.03109054507046238, 6.816801101491506643, -3.135084751894932076 ) ) ;
#36355 = DIRECTION ( 'NONE',  ( 0.9816537812491076265, 0.1906721105965138718, 4.769617732184456426E-16 ) ) ;
#36356 = CARTESIAN_POINT ( 'NONE',  ( 18.34612162485796460, 147.3262642721504960, 2.396769171045068703 ) ) ;
#36357 = CARTESIAN_POINT ( 'NONE',  ( -4.975175664203050907, 32.06598106186588382, 0.7459204072935275986 ) ) ;
#36358 = CARTESIAN_POINT ( 'NONE',  ( 22.98488057257191741, 150.1591296352320910, 0.4592926148156237232 ) ) ;
#36359 = CARTESIAN_POINT ( 'NONE',  ( 7.690436415270363923, 8.290658626076512050, -3.468142284020285793 ) ) ;
#36360 = CARTESIAN_POINT ( 'NONE',  ( 15.56637720654300061, 147.8873989650969918, 1.033077377765619920 ) ) ;
#36361 = ADVANCED_FACE ( 'NONE', ( #4515 ), #37619, .T. ) ;
#36362 = CARTESIAN_POINT ( 'NONE',  ( 11.23106549681877020, 119.1264784044212632, -0.5965447130870017434 ) ) ;
#36363 = DIRECTION ( 'NONE',  ( 0.9998004120163608288, 5.205824365704082573E-17, 0.01997839162482760098 ) ) ;
#36364 = AXIS2_PLACEMENT_3D ( 'NONE', #36394, #29777, #4023 ) ;
#36365 = EDGE_LOOP ( 'NONE', ( #18959, #21214 ) ) ;
#36366 = CARTESIAN_POINT ( 'NONE',  ( 1.580596280061897341, 115.6909491485452719, 1.732191492244595565 ) ) ;
#36367 = CARTESIAN_POINT ( 'NONE',  ( -15.19466275752374251, 156.0906695176550443, -0.2814020119901240458 ) ) ;
#36368 = ORIENTED_EDGE ( 'NONE', *, *, #10027, .F. ) ;
#36369 = CARTESIAN_POINT ( 'NONE',  ( 7.973790791625233965, 121.7927018305182827, -0.7354518077562433032 ) ) ;
#36370 = CARTESIAN_POINT ( 'NONE',  ( -14.64596739026573857, 69.73430801926814127, -1.269999999999999130 ) ) ;
#36371 = CIRCLE ( 'NONE', #10503, 0.7620000000000036744 ) ;
#36372 = CARTESIAN_POINT ( 'NONE',  ( -12.12200908156761336, 130.5412724693565849, -0.6534646642625603352 ) ) ;
#36373 = CARTESIAN_POINT ( 'NONE',  ( 3.088592312018083152, -14.58504802601380490, 5.263618629775349333 ) ) ;
#36374 = CARTESIAN_POINT ( 'NONE',  ( -12.81731082034063363, 120.0678233105195716, 0.7045657984066410195 ) ) ;
#36375 = DIRECTION ( 'NONE',  ( 4.017660918040594346E-17, -1.000000000000000000, -2.376309959284834438E-19 ) ) ;
#36376 = CARTESIAN_POINT ( 'NONE',  ( 14.87533653215386131, 120.3210621052586475, 0.3471466443384770284 ) ) ;
#36377 = EDGE_CURVE ( 'NONE', #6797, #32761, #3255, .T. ) ;
#36378 = EDGE_LOOP ( 'NONE', ( #32476, #19726, #3750, #26713 ) ) ;
#36379 = CARTESIAN_POINT ( 'NONE',  ( 1.104432469574216480, -9.427232690354344413, -4.492858291722996888 ) ) ;
#36380 = CARTESIAN_POINT ( 'NONE',  ( -23.36121599382910219, 148.8756354988261990, -0.4668126921608655722 ) ) ;
#36381 = DIRECTION ( 'NONE',  ( 9.627370216492862708E-17, 1.000000000000000000, -0.000000000000000000 ) ) ;
#36382 = CARTESIAN_POINT ( 'NONE',  ( -20.83467972660109524, 65.95194780259438971, 1.904999999999986704 ) ) ;
#36383 = CARTESIAN_POINT ( 'NONE',  ( -4.589236464118411796, 118.7495122949379294, 0.8846585347348726591 ) ) ;
#36384 = CARTESIAN_POINT ( 'NONE',  ( 0.6256056815405413030, -8.068247431453825058, 4.577905309659676014 ) ) ;
#36385 = CARTESIAN_POINT ( 'NONE',  ( 20.05503673871676540, 132.0867704272472452, 1.718978086785435178 ) ) ;
#36386 = CARTESIAN_POINT ( 'NONE',  ( -56.80696390459748102, 3.604343092604253673, -2.316781442554163739 ) ) ;
#36388 = CARTESIAN_POINT ( 'NONE',  ( 14.47132921234235958, 123.3930721568691382, -1.260850717050815861 ) ) ;
#36387 = CARTESIAN_POINT ( 'NONE',  ( 5.638212235186404797, 57.14999999999997016, 5.060089761242341666 ) ) ;
#36389 = CARTESIAN_POINT ( 'NONE',  ( -4.070821798575407158, -9.904843093959119216, 2.245307785351264407 ) ) ;
#36390 = CARTESIAN_POINT ( 'NONE',  ( -12.99089357651424770, 156.9259531928012734, -1.181820989919032616 ) ) ;
#36391 = ORIENTED_EDGE ( 'NONE', *, *, #40491, .F. ) ;
#36392 = CARTESIAN_POINT ( 'NONE',  ( -9.191362964798114987, 123.9301100385560943, 0.1344743934557743881 ) ) ;
#36393 = CARTESIAN_POINT ( 'NONE',  ( 2.665431962039443992, -15.40910046105366327, 5.814861676232141008 ) ) ;
#36394 = CARTESIAN_POINT ( 'NONE',  ( -17.64290547347870941, 83.78857423953914463, -1.524000000000003130 ) ) ;
#36395 = CARTESIAN_POINT ( 'NONE',  ( -3.275932770776605274, 108.4907222760759282, -4.202228437981203157 ) ) ;
#36396 = ORIENTED_EDGE ( 'NONE', *, *, #20631, .F. ) ;
#36397 = CARTESIAN_POINT ( 'NONE',  ( 14.48730688186159199, 125.6573275863457866, 2.042335292678053360 ) ) ;
#36398 = DIRECTION ( 'NONE',  ( -5.188838149069472160E-16, 1.699382548006136559E-16, 1.000000000000000000 ) ) ;
#36399 = CARTESIAN_POINT ( 'NONE',  ( -29.27763062208790856, 65.70811510315778037, -1.270000000000006013 ) ) ;
#36400 = CARTESIAN_POINT ( 'NONE',  ( -21.20416308100202585, 151.2337125027825095, 0.8636963275675618723 ) ) ;
#36401 = CARTESIAN_POINT ( 'NONE',  ( 0.04286443493920111952, 25.39157861068392208, -8.424000189867014043 ) ) ;
#36402 = CARTESIAN_POINT ( 'NONE',  ( 13.09552101555870784, 130.8944540161131442, 1.428626934261719272 ) ) ;
#36403 = CARTESIAN_POINT ( 'NONE',  ( 18.44111676445463388, 125.1790410860780298, -0.1047302884851512295 ) ) ;
#36404 = LINE ( 'NONE', #20597, #3639 ) ;
#36405 = CARTESIAN_POINT ( 'NONE',  ( -52.44164295988605318, 11.83295133839460611, 4.069468471668873377 ) ) ;
#36406 = CARTESIAN_POINT ( 'NONE',  ( -47.08352113710599696, 24.38425570713750190, 2.219725161937576630 ) ) ;
#36407 = CARTESIAN_POINT ( 'NONE',  ( 13.85159022459153988, 59.63164443796365077, 5.016499999999999737 ) ) ;
#36408 = CARTESIAN_POINT ( 'NONE',  ( -55.60486134785667645, 7.243031971518515633, 3.140198620020484110 ) ) ;
#36409 = CARTESIAN_POINT ( 'NONE',  ( -58.18695740882700562, 0.6575158937857172869, 1.151667878608726214 ) ) ;
#36410 = CARTESIAN_POINT ( 'NONE',  ( -4.456310623878905197, 118.1611138379835779, 0.4358899058150005335 ) ) ;
#36411 = CARTESIAN_POINT ( 'NONE',  ( -58.12768216001780530, 0.1527613808938732554, -0.09815255304910418255 ) ) ;
#36412 = ORIENTED_EDGE ( 'NONE', *, *, #38386, .T. ) ;
#36413 = CARTESIAN_POINT ( 'NONE',  ( -44.40534991575952972, 23.82367036525651116, 1.730788704199185624 ) ) ;
#36414 = CARTESIAN_POINT ( 'NONE',  ( 3.767507399439959936, 118.8938511920684107, -0.7849653907999185609 ) ) ;
#36415 = CARTESIAN_POINT ( 'NONE',  ( -3.930440796539918402, 109.7948460773305897, -3.685213129881072192 ) ) ;
#36416 = CARTESIAN_POINT ( 'NONE',  ( 4.571841262500583980, 118.0790968600936424, 0.7158236320836997013 ) ) ;
#36417 = CARTESIAN_POINT ( 'NONE',  ( -15.82363114525499981, 143.7482200480382346, -1.443160993194752217 ) ) ;
#36418 = CARTESIAN_POINT ( 'NONE',  ( -1.253177666489279973, 115.7029074776113191, -1.740281551268416216 ) ) ;
#36419 = CARTESIAN_POINT ( 'NONE',  ( 4.005922464918031167, 117.9496054017496789, -1.072511926687662376 ) ) ;
#36420 = CARTESIAN_POINT ( 'NONE',  ( 0.3646759018190506851, 105.8822825325953261, -5.328619312200441271 ) ) ;
#36421 = CARTESIAN_POINT ( 'NONE',  ( -16.93203274801149405, 148.0818255213264365, -2.041866944467892520 ) ) ;
#36422 = CARTESIAN_POINT ( 'NONE',  ( 5.336581877858352030, 116.0444662015457595, -0.07592003752709637621 ) ) ;
#36423 = CARTESIAN_POINT ( 'NONE',  ( -0.01133107913651526001, 156.3792106723807649, 0.5670535347366658652 ) ) ;
#36424 = CARTESIAN_POINT ( 'NONE',  ( 8.022816897867139474, 121.5631586913658140, -0.8332660241015871216 ) ) ;
#36425 = CARTESIAN_POINT ( 'NONE',  ( -7.046335199868481780, 122.0731595262481051, -0.02430996038715024440 ) ) ;
#36426 = CARTESIAN_POINT ( 'NONE',  ( 2.294499597581835193, -9.852027417895397932, -4.012603411698490774 ) ) ;
#36427 = CARTESIAN_POINT ( 'NONE',  ( 14.96245403159064047, 120.9606250904355704, 1.059951836595168118 ) ) ;
#36428 = CARTESIAN_POINT ( 'NONE',  ( -26.29578028364076658, 73.87584665086983193, -1.524000000000006017 ) ) ;
#36429 = CARTESIAN_POINT ( 'NONE',  ( 3.315889604118840150, -14.76599673617913488, 0.9486971755708663023 ) ) ;
#36430 = CARTESIAN_POINT ( 'NONE',  ( -19.07204494652747329, 148.5750135429820205, 1.735237764431467822 ) ) ;
#36431 = CARTESIAN_POINT ( 'NONE',  ( 0.7131539557513479899, -7.844638678481905103, 0.6656887750258669856 ) ) ;
#36432 = CARTESIAN_POINT ( 'NONE',  ( -22.52188062635582710, 150.6069110094195764, -1.039808695286016160 ) ) ;
#36433 = CARTESIAN_POINT ( 'NONE',  ( -0.9409916986186561694, 26.46864381685040257, -0.2619748070941995688 ) ) ;
#36434 = ORIENTED_EDGE ( 'NONE', *, *, #11385, .T. ) ;
#36435 = CARTESIAN_POINT ( 'NONE',  ( -45.43219756685621036, 19.09711438432238495, 1.200471166368901166 ) ) ;
#36436 = CARTESIAN_POINT ( 'NONE',  ( -0.1065646865916381608, 105.8844662015456777, 5.332932678536313809 ) ) ;
#36437 = COLOUR_RGB ( '', 0.72549020, 0.75294118, 0.79215686) ;
#36438 = CARTESIAN_POINT ( 'NONE',  ( -0.004916276843202750484, 120.6356583033945782, 0.2460305967400717997 ) ) ;
#36439 = CARTESIAN_POINT ( 'NONE',  ( 4.222548444470398010, -13.63200092856201096, 3.862739453107805421 ) ) ;
#36440 = CARTESIAN_POINT ( 'NONE',  ( 17.11529127082739521, 148.4623951536435698, -1.463161431351220454 ) ) ;
#36441 = CARTESIAN_POINT ( 'NONE',  ( -4.285767465938752352, 157.6046910967438066, -1.850878756276731263 ) ) ;
#36442 = CARTESIAN_POINT ( 'NONE',  ( 1.477727405461724555E-15, 14.60500000000000220, 0.000000000000000000 ) ) ;
#36443 = CARTESIAN_POINT ( 'NONE',  ( 3.221527947697278904, -14.19553219070161809, 2.775880300951635071 ) ) ;
#36444 = CYLINDRICAL_SURFACE ( 'NONE', #5485, 0.6350000000000014522 ) ;
#36445 = CARTESIAN_POINT ( 'NONE',  ( 15.74722489594608454, 146.9052959264698757, 0.08484200870240335424 ) ) ;
#36446 = EDGE_LOOP ( 'NONE', ( #1480, #6201, #26530, #11821 ) ) ;
#36447 = LINE ( 'NONE', #33463, #34292 ) ;
#36448 = CARTESIAN_POINT ( 'NONE',  ( -6.059261036834475256, 57.15000000000000568, 5.016499999999999737 ) ) ;
#36449 = LINE ( 'NONE', #9606, #35455 ) ;
#36450 = CARTESIAN_POINT ( 'NONE',  ( 22.69744207413518922, 137.3157656003441787, 0.3098006952201959319 ) ) ;
#36451 = CARTESIAN_POINT ( 'NONE',  ( -5.292163649236576894, 116.0761519159950552, 1.031159682278862455 ) ) ;
#36452 = CARTESIAN_POINT ( 'NONE',  ( 2.160577569948397780, -15.38714209653413434, 5.933462479304245640 ) ) ;
#36453 = CARTESIAN_POINT ( 'NONE',  ( 14.95453923199683111, 61.75387968257833649, -5.016499999999999737 ) ) ;
#36454 = CARTESIAN_POINT ( 'NONE',  ( -3.294745019374083039, 31.35739020231596896, 0.3090114964385932139 ) ) ;
#36455 = CARTESIAN_POINT ( 'NONE',  ( 3.119203903361051911, 118.1710492231644736, 0.8508709904442465222 ) ) ;
#36456 = AXIS2_PLACEMENT_3D ( 'NONE', #8273, #21871, #17847 ) ;
#36457 = CARTESIAN_POINT ( 'NONE',  ( -4.628372119175923949, 18.04465247731148381, -0.2036312542868722320 ) ) ;
#36458 = CARTESIAN_POINT ( 'NONE',  ( 0.2611430735369592582, 24.48315862702271417, 8.432237392808469068 ) ) ;
#36459 = CARTESIAN_POINT ( 'NONE',  ( -5.540182818362195505, 118.0041147760924076, -1.099220559926700647 ) ) ;
#36460 = CARTESIAN_POINT ( 'NONE',  ( -0.7702483762746622498, 120.5370721568272216, -0.5278276654545120961 ) ) ;
#36461 = CARTESIAN_POINT ( 'NONE',  ( 1.167505706004672243E-15, 11.53894877578617084, 0.000000000000000000 ) ) ;
#36462 = CARTESIAN_POINT ( 'NONE',  ( -10.45888906141536268, 56.51499999999998636, -4.393716635381741398 ) ) ;
#36463 = CARTESIAN_POINT ( 'NONE',  ( -4.383044586904778050, 104.6144662015500870, 3.059726520723942134 ) ) ;
#36464 = CARTESIAN_POINT ( 'NONE',  ( 0.05711764529616595448, 0.5181683540770932739, -4.631227783250111862 ) ) ;
#36465 = DIRECTION ( 'NONE',  ( 5.188838149069472160E-16, -1.699382548006136559E-16, -1.000000000000000000 ) ) ;
#36466 = CARTESIAN_POINT ( 'NONE',  ( -16.31694223957266843, 121.4173703750124531, -0.3260513381110076714 ) ) ;
#36467 = CARTESIAN_POINT ( 'NONE',  ( 3.250423480262735421, -14.11372661294146802, 3.006569077614236196 ) ) ;
#36468 = CARTESIAN_POINT ( 'NONE',  ( 3.173429932894971106, 117.8122656274855871, -0.8370585861429156171 ) ) ;
#36469 = CARTESIAN_POINT ( 'NONE',  ( -14.99285373232509322, 120.9606250904355704, 0.4613734978017341448 ) ) ;
#36470 = CARTESIAN_POINT ( 'NONE',  ( 6.657354856306101354, 117.1094500246672538, 0.1330297933348817407 ) ) ;
#36471 = DIRECTION ( 'NONE',  ( 0.000000000000000000, 0.000000000000000000, 1.000000000000000000 ) ) ;
#36472 = ORIENTED_EDGE ( 'NONE', *, *, #38882, .F. ) ;
#36473 = DIRECTION ( 'NONE',  ( 0.9816537812491089587, 0.1906721105965065444, 4.769617732184475162E-16 ) ) ;
#36474 = CARTESIAN_POINT ( 'NONE',  ( 4.776532240430319654, -15.60394515218366251, 2.960345780779299663 ) ) ;
#36475 = CARTESIAN_POINT ( 'NONE',  ( -18.54838064703208644, 135.7714211226372640, 1.677382267734012666 ) ) ;
#36476 = CARTESIAN_POINT ( 'NONE',  ( 2.121647970409600514, 117.6567184779878232, -0.5798693372496743770 ) ) ;
#36477 = CARTESIAN_POINT ( 'NONE',  ( -0.7497900579835341528, 31.49133049583988608, -0.6186479539722394838 ) ) ;
#36478 = CARTESIAN_POINT ( 'NONE',  ( -58.59553834934886396, -0.2237177117754586830, -0.4722778291337721424 ) ) ;
#36479 = ORIENTED_EDGE ( 'NONE', *, *, #39925, .F. ) ;
#36480 = CARTESIAN_POINT ( 'NONE',  ( -19.33375693323417366, 80.42273151551299293, 1.269999999999995577 ) ) ;
#36481 = CARTESIAN_POINT ( 'NONE',  ( 2.328338358121097240, 124.8000875644994068, 0.05398387088914125692 ) ) ;
#36482 = SURFACE_STYLE_USAGE ( .BOTH. , #30699 ) ;
#36483 = CARTESIAN_POINT ( 'NONE',  ( -7.262759831279749001, 121.2980461901665308, 0.7361999724971877157 ) ) ;
#36484 = CARTESIAN_POINT ( 'NONE',  ( -0.01822531903872333034, 118.1564764849152738, 0.9120692297075591037 ) ) ;
#36485 = CARTESIAN_POINT ( 'NONE',  ( 18.72287149482784230, 147.1333978507680627, -1.701234099286256019 ) ) ;
#36486 = CARTESIAN_POINT ( 'NONE',  ( -20.66962185543556529, 147.7542213611591535, -2.445644978772824718 ) ) ;
#36487 = DIRECTION ( 'NONE',  ( 0.7548010569845216011, 0.6559537821943317581, 2.801824109679581255E-16 ) ) ;
#36488 = AXIS2_PLACEMENT_3D ( 'NONE', #5146, #40911, #24284 ) ;
#36489 = CARTESIAN_POINT ( 'NONE',  ( 4.116435971365464574, 118.2429491485453354, -0.1883497800502350605 ) ) ;
#36490 = CARTESIAN_POINT ( 'NONE',  ( 14.97557080935131779, 148.8997249754567349, -0.5399649533830230830 ) ) ;
#36491 = AXIS2_PLACEMENT_3D ( 'NONE', #2248, #18614, #21373 ) ;
#36492 = ORIENTED_EDGE ( 'NONE', *, *, #1985, .F. ) ;
#36493 = CARTESIAN_POINT ( 'NONE',  ( 2.572675278006325339, -15.15086880438208716, 4.677806725582212444 ) ) ;
#36494 = CARTESIAN_POINT ( 'NONE',  ( 5.285208019315508210, 105.1224194135358090, -0.7957335705207263521 ) ) ;
#36495 = DIRECTION ( 'NONE',  ( 0.000000000000000000, 0.000000000000000000, 1.000000000000000000 ) ) ;
#36496 = CARTESIAN_POINT ( 'NONE',  ( 4.198131962423935271, 12.64715247731088787, 1.959332076845688553 ) ) ;
#36497 = CARTESIAN_POINT ( 'NONE',  ( -0.02400040557479750369, 156.7459281804771365, 1.201078436782489600 ) ) ;
#36498 = CARTESIAN_POINT ( 'NONE',  ( 0.7097672177479600331, 33.90743241353141713, 1.308455980856628731 ) ) ;
#36499 = CARTESIAN_POINT ( 'NONE',  ( -0.01876340930523686876, 19.73428105357427853, -4.634220987317214657 ) ) ;
#36500 = CARTESIAN_POINT ( 'NONE',  ( 9.231158399652199975, 124.2544328994657405, 0.2701740761454697326 ) ) ;
#36501 = LINE ( 'NONE', #3930, #38545 ) ;
#36502 =( BOUNDED_SURFACE ( )  B_SPLINE_SURFACE ( 3, 2, ( 
 ( #14130, #8379, #24768 ),
 ( #27132, #40145, #2002 ),
 ( #33751, #10937, #27555 ),
 ( #7763, #37352, #27966 ),
 ( #21344, #4577, #37766 ),
 ( #17535, #30953, #40975 ),
 ( #1588, #8170, #34370 ),
 ( #17952, #30536, #40562 ),
 ( #31161, #5203, #14332 ),
 ( #7967, #27343, #21137 ),
 ( #20511, #37145, #40355 ),
 ( #11150, #33539, #24137 ),
 ( #1793, #33960, #4789 ),
 ( #40767, #17739, #34167 ),
 ( #11360, #4993, #11565 ),
 ( #14756, #27756, #29012 ),
 ( #28813, #3056, #5834 ),
 ( #31801, #18366, #38415 ),
 ( #9018, #18582, #21981 ),
 ( #41400, #32223, #24983 ),
 ( #15806, #12827, #18788 ),
 ( #6041, #19214, #9424 ),
 ( #8807, #34791, #31591 ),
 ( #2428, #35014, #6244 ) ),
 .UNSPECIFIED., .F., .F., .F. ) 
 B_SPLINE_SURFACE_WITH_KNOTS ( ( 4, 2, 2, 2, 2, 2, 2, 2, 2, 2, 2, 4 ),
 ( 3, 3 ),
 ( 0.000000000000000000, 0.0005614604826172228322, 0.001122920965234445664, 0.001684381447851668497, 0.002245841930468891329, 0.003368762895703336993, 0.004491683860937782657, 0.005614604826172228322, 0.006737525791406673986, 0.007298986274023896818, 0.007860446756641119651, 0.008983367721875565315 ),
 ( 0.000000000000000000, 1.000000000000000000 ),
 .UNSPECIFIED. ) 
 GEOMETRIC_REPRESENTATION_ITEM ( )  RATIONAL_B_SPLINE_SURFACE ( (
 ( 1.000000000000000000, 0.9987193938133342996, 1.000000000000000000),
 ( 1.000000000000000000, 0.9982000373971027241, 1.000000000000000000),
 ( 1.000000000000000000, 0.9975619604953736008, 1.000000000000000000),
 ( 1.000000000000000000, 0.9916939477464365993, 1.000000000000000000),
 ( 1.000000000000000000, 0.9861209039935189269, 1.000000000000000000),
 ( 1.000000000000000000, 0.9617740169780845116, 1.000000000000000000),
 ( 1.000000000000000000, 0.9448443023889108172, 1.000000000000000000),
 ( 1.000000000000000000, 0.9146158020808421441, 1.000000000000000000),
 ( 1.000000000000000000, 0.9004045293487663582, 1.000000000000000000),
 ( 1.000000000000000000, 0.8619933248317470653, 1.000000000000000000),
 ( 1.000000000000000000, 0.8427343359422859725, 1.000000000000000000),
 ( 1.000000000000000000, 0.8121850874637416284, 1.000000000000000000),
 ( 1.000000000000000000, 0.8005416906217645012, 1.000000000000000000),
 ( 1.000000000000000000, 0.7821458849528583057, 1.000000000000000000),
 ( 1.000000000000000000, 0.7751654015759510408, 1.000000000000000000),
 ( 1.000000000000000000, 0.7626205617104924173, 1.000000000000000000),
 ( 1.000000000000000000, 0.7574054414911801647, 1.000000000000000000),
 ( 1.000000000000000000, 0.7453179101192215494, 1.000000000000000000),
 ( 1.000000000000000000, 0.7405197175285387345, 1.000000000000000000),
 ( 1.000000000000000000, 0.7299770405551697650, 1.000000000000000000),
 ( 1.000000000000000000, 0.7243132446522438928, 1.000000000000000000),
 ( 1.000000000000000000, 0.7087302219173966522, 1.000000000000000000),
 ( 1.000000000000000000, 0.7007553748469402821, 1.000000000000000000),
 ( 1.000000000000000000, 0.7072256012393058899, 1.000000000000000000) ) ) 
 REPRESENTATION_ITEM ( '' )  SURFACE ( )  );
#36503 = CARTESIAN_POINT ( 'NONE',  ( -52.76126113563441322, 10.11686208896574257, -1.835409310531190163 ) ) ;
#36504 = CARTESIAN_POINT ( 'NONE',  ( 5.559215554539349569, 116.7531585254012327, -0.1425236539881735154 ) ) ;
#36505 = CARTESIAN_POINT ( 'NONE',  ( -1.627181853488509411, 117.3993836203756302, 1.397816796450546128 ) ) ;
#36506 = CARTESIAN_POINT ( 'NONE',  ( -11.32337086946255056, 78.46996359545325106, -1.523999999999999133 ) ) ;
#36507 = LINE ( 'NONE', #39922, #7779 ) ;
#36508 = CARTESIAN_POINT ( 'NONE',  ( -29.30569680556072498, 61.36914094226862204, -1.524000000003056243 ) ) ;
#36509 = DIRECTION ( 'NONE',  ( -5.188838149069471174E-16, 1.699382548006136313E-16, 1.000000000000000000 ) ) ;
#36510 = CARTESIAN_POINT ( 'NONE',  ( 5.237379388564934679, 115.7029491485453292, 1.024072862575109655 ) ) ;
#36511 = CARTESIAN_POINT ( 'NONE',  ( -9.094996104468901166, 78.64197151092922411, -1.904999999999999583 ) ) ;
#36512 = CARTESIAN_POINT ( 'NONE',  ( -57.97744691355249813, 2.174673694799844625, 0.6577596567055979948 ) ) ;
#36513 = EDGE_CURVE ( 'NONE', #28134, #10936, #8741, .T. ) ;
#36514 = CARTESIAN_POINT ( 'NONE',  ( -58.75009580408200094, 0.1057190229620807997, 0.6617493214610802310 ) ) ;
#36515 = CARTESIAN_POINT ( 'NONE',  ( -22.47159541194106680, 150.7739627601066275, 0.0002021107738997875169 ) ) ;
#36516 = AXIS2_PLACEMENT_3D ( 'NONE', #19092, #32098, #28896 ) ;
#36517 = ORIENTED_EDGE ( 'NONE', *, *, #14611, .T. ) ;
#36518 = CARTESIAN_POINT ( 'NONE',  ( -57.35225397299146977, 4.112755766825001658, -0.3099640861128369895 ) ) ;
#36519 = CARTESIAN_POINT ( 'NONE',  ( -7.787852718269741459, 122.6010352751677033, -0.2744241607441815223 ) ) ;
#36520 = ORIENTED_EDGE ( 'NONE', *, *, #22183, .T. ) ;
#36521 = CARTESIAN_POINT ( 'NONE',  ( -12.69999999999999574, 14.60500000000000398, 0.000000000000000000 ) ) ;
#36522 = CARTESIAN_POINT ( 'NONE',  ( -1.562757238090153988, 156.2577446057484281, -0.06075558507430124655 ) ) ;
#36523 = CARTESIAN_POINT ( 'NONE',  ( 2.466063760571058250, -15.50753052345275940, 5.840068263025540496 ) ) ;
#36524 = CARTESIAN_POINT ( 'NONE',  ( -9.140851504705459263, 119.2843051134756536, 0.9831809102843883652 ) ) ;
#36525 = CARTESIAN_POINT ( 'NONE',  ( 4.377640660406503237, 26.40621510375495973, 1.544744264128281364 ) ) ;
#36526 = CARTESIAN_POINT ( 'NONE',  ( 5.687008767712439017, 159.1209727096294273, 0.4156250475054877880 ) ) ;
#36527 = CARTESIAN_POINT ( 'NONE',  ( 14.11204817291316083, 138.8091675146647788, 0.4809352338920104275 ) ) ;
#36528 = CARTESIAN_POINT ( 'NONE',  ( 3.400481176189167343, 25.78150505744974552, 3.158589348000393482 ) ) ;
#36529 = CARTESIAN_POINT ( 'NONE',  ( 0.6613080194379835630, -2.301230296243127693, 0.7179688673762391060 ) ) ;
#36530 = CARTESIAN_POINT ( 'NONE',  ( -5.799544261406411216, 116.9771394561422539, -0.2896453145609860225 ) ) ;
#36531 = EDGE_CURVE ( 'NONE', #10259, #24258, #22258, .T. ) ;
#36532 = CARTESIAN_POINT ( 'NONE',  ( 4.962080476404062246, 117.4056796065936368, 1.029808796348710143 ) ) ;
#36533 = ORIENTED_EDGE ( 'NONE', *, *, #5534, .T. ) ;
#36534 = CARTESIAN_POINT ( 'NONE',  ( 2.201628648472980121, 116.2290761738841525, 0.1197410424596312972 ) ) ;
#36535 = CARTESIAN_POINT ( 'NONE',  ( -0.9295719194793629070, 157.1975648536147787, 1.475660455335214838 ) ) ;
#36536 = CARTESIAN_POINT ( 'NONE',  ( -57.85882094617455351, 0.8103094007012910938, -1.033824511878239871 ) ) ;
#36537 = CARTESIAN_POINT ( 'NONE',  ( 21.19397400757779337, 145.8710773725474610, 2.320968965272669937 ) ) ;
#36538 = CARTESIAN_POINT ( 'NONE',  ( 13.45896140341249847, 123.7870877700634509, -1.380644293323453065 ) ) ;
#36539 = CARTESIAN_POINT ( 'NONE',  ( 0.3265437062995015238, -4.820036860806069967, -0.9201843903956486992 ) ) ;
#36540 = CARTESIAN_POINT ( 'NONE',  ( -1.196040046930182399, 159.0162744061759099, -1.350631977726330479 ) ) ;
#36541 = AXIS2_PLACEMENT_3D ( 'NONE', #4335, #7308, #24105 ) ;
#36542 = CARTESIAN_POINT ( 'NONE',  ( 4.690458750227413987, 118.0052497351821756, -0.5846114136641620274 ) ) ;
#36543 = CARTESIAN_POINT ( 'NONE',  ( -46.82679756180435504, 21.08486709759267086, -4.907624977305287572 ) ) ;
#36544 = CARTESIAN_POINT ( 'NONE',  ( 5.262496720419017393, 105.1224535734649663, 0.9374057647381621727 ) ) ;
#36545 = CARTESIAN_POINT ( 'NONE',  ( 1.787077659700166077, 156.4219299504922844, -0.8362026816545214958 ) ) ;
#36546 = CARTESIAN_POINT ( 'NONE',  ( 7.799334277748505961, 122.5403225720764908, 0.4385505410406168036 ) ) ;
#36547 = ORIENTED_EDGE ( 'NONE', *, *, #33964, .F. ) ;
#36548 = CARTESIAN_POINT ( 'NONE',  ( -0.4867666382967937300, 119.1670848682014281, -0.5956043695837970331 ) ) ;
#36549 = CARTESIAN_POINT ( 'NONE',  ( 2.719191112037562252, -15.71471113085404170, 5.040136806425350002 ) ) ;
#36550 = CARTESIAN_POINT ( 'NONE',  ( -4.575234526219186471, 118.0705373586567646, -0.7555243366678462413 ) ) ;
#36551 = EDGE_CURVE ( 'NONE', #1729, #3642, #1251, .T. ) ;
#36552 = CARTESIAN_POINT ( 'NONE',  ( -49.56090548067184898, 17.87959676410238430, -5.165259844110624776 ) ) ;
#36553 = AXIS2_PLACEMENT_3D ( 'NONE', #23271, #27746, #14536 ) ;
#36554 = CARTESIAN_POINT ( 'NONE',  ( -24.10666987309389597, 82.16896248603319464, -1.270000000000006235 ) ) ;
#36555 = CARTESIAN_POINT ( 'NONE',  ( 9.942133252021193357, 155.4362223408194836, 2.105659105541914045 ) ) ;
#36556 = CYLINDRICAL_SURFACE ( 'NONE', #29437, 0.5080000000000000071 ) ;
#36557 = ADVANCED_FACE ( 'NONE', ( #33897 ), #18181, .F. ) ;
#36558 = CARTESIAN_POINT ( 'NONE',  ( 15.54847974360315099, 120.7212560704218589, 0.2938029371637450038 ) ) ;
#36559 = ADVANCED_FACE ( 'NONE', ( #37289 ), #27498, .F. ) ;
#36560 = CARTESIAN_POINT ( 'NONE',  ( 7.942258639034435852, 16.71227948022357523, 2.857158061122382353 ) ) ;
#36561 = CARTESIAN_POINT ( 'NONE',  ( 15.83096054209195991, 147.2950763206921181, 1.041347660067663439 ) ) ;
#36562 = CARTESIAN_POINT ( 'NONE',  ( 16.32943869337475817, 155.1963085991477271, -0.7556961354993015911 ) ) ;
#36563 = FACE_OUTER_BOUND ( 'NONE', #35435, .T. ) ;
#36564 = FACE_OUTER_BOUND ( 'NONE', #19233, .T. ) ;
#36565 = AXIS2_PLACEMENT_3D ( 'NONE', #15653, #9285, #32065 ) ;
#36566 = CARTESIAN_POINT ( 'NONE',  ( -18.76910502294238370, 125.2887878443791294, -0.2589991215523649304 ) ) ;
#36567 = ORIENTED_EDGE ( 'NONE', *, *, #13594, .F. ) ;
#36568 = CARTESIAN_POINT ( 'NONE',  ( 7.988278544293920369, 121.7250811996676134, -0.7665462581867787950 ) ) ;
#36569 = CARTESIAN_POINT ( 'NONE',  ( -8.798071503382049130, 117.6842349159514640, -0.1758064068840608507 ) ) ;
#36570 = ORIENTED_EDGE ( 'NONE', *, *, #6820, .T. ) ;
#36571 = CARTESIAN_POINT ( 'NONE',  ( -6.437058721807690810E-14, 62.83146620154573014, 4.519164521849267879E-29 ) ) ;
#36572 = CARTESIAN_POINT ( 'NONE',  ( -1.615823435711636780, 156.2764358050213787, -0.4002269557471576644 ) ) ;
#36573 = CARTESIAN_POINT ( 'NONE',  ( 3.194768752100229925, -14.65262985833884457, 5.377959301279905624 ) ) ;
#36574 = CARTESIAN_POINT ( 'NONE',  ( -9.403995501905267673, 118.7255599110314961, 0.7521618898589479407 ) ) ;
#36575 = CARTESIAN_POINT ( 'NONE',  ( -6.608367952640316290, 78.82866613109548837, -3.480504251946396455 ) ) ;
#36576 = CARTESIAN_POINT ( 'NONE',  ( 23.10830587629915556, 149.8995197111492814, 0.5387578213853486675 ) ) ;
#36577 = VERTEX_POINT ( 'NONE', #24920 ) ;
#36578 = CARTESIAN_POINT ( 'NONE',  ( -3.974385726840726107, -7.478117039488521023, -2.359557994316856533 ) ) ;
#36579 = CARTESIAN_POINT ( 'NONE',  ( -16.30293663320045994, 121.4145675751456253, -0.3429698291441254931 ) ) ;
#36580 = DIRECTION ( 'NONE',  ( 0.01997839162482749689, 1.040247600000945640E-18, -0.9998004120163610509 ) ) ;
#36581 = DIRECTION ( 'NONE',  ( 0.8745520943968240202, -0.4849315768086553402, 6.829619984160650158E-16 ) ) ;
#36582 = AXIS2_PLACEMENT_3D ( 'NONE', #20048, #33066, #10258 ) ;
#36583 = CARTESIAN_POINT ( 'NONE',  ( 8.163255772186461812, 120.6602155040159658, 1.404671597144966144 ) ) ;
#36584 = CARTESIAN_POINT ( 'NONE',  ( -2.329872802932658082, -2.670747431267189498, -3.990024091085845548 ) ) ;
#36585 = CARTESIAN_POINT ( 'NONE',  ( 22.33586214876074649, 148.6363688457942942, 1.892951199575522159 ) ) ;
#36586 = CARTESIAN_POINT ( 'NONE',  ( -58.64207371057509022, -0.3086014758122701540, -0.3447476069571805413 ) ) ;
#36588 = CARTESIAN_POINT ( 'NONE',  ( 19.23923079580225348, 135.9655892003723636, -1.583918808943347578 ) ) ;
#36587 = DIRECTION ( 'NONE',  ( 4.017660918040594346E-17, -1.000000000000000000, -2.376309959284834438E-19 ) ) ;
#36589 = CARTESIAN_POINT ( 'NONE',  ( 3.857898856315107761, -6.768822978661375167, 2.551181839177400601 ) ) ;
#36590 = CARTESIAN_POINT ( 'NONE',  ( -5.495761340641479364, 159.0395019988757781, -0.8742782617121152011 ) ) ;
#36591 = ORIENTED_EDGE ( 'NONE', *, *, #27215, .F. ) ;
#36592 = ORIENTED_EDGE ( 'NONE', *, *, #28804, .F. ) ;
#36593 = EDGE_CURVE ( 'NONE', #35792, #4212, #8683, .T. ) ;
#36594 = CARTESIAN_POINT ( 'NONE',  ( -9.006799368204402967, 123.6974368934138226, 0.1328627719367738713 ) ) ;
#36595 = CARTESIAN_POINT ( 'NONE',  ( 4.983883817524661808, -15.00518790705197780, 4.081033524500047527 ) ) ;
#36596 = CARTESIAN_POINT ( 'NONE',  ( -41.35619903644415984, 22.77303286471932964, 1.271070091490069665 ) ) ;
#36597 = CIRCLE ( 'NONE', #33865, 0.2540000000000012248 ) ;
#36598 = CARTESIAN_POINT ( 'NONE',  ( -4.549004567883367933, 112.0093730493565545, -2.856396963121139443 ) ) ;
#36599 = EDGE_LOOP ( 'NONE', ( #20463, #5923, #25630, #25655 ) ) ;
#36600 = CARTESIAN_POINT ( 'NONE',  ( 2.300165013715926854, 118.7486697826011977, 0.8022418554901109555 ) ) ;
#36601 = DIRECTION ( 'NONE',  ( 1.011795553208986377E-16, 1.000000000000000000, -0.000000000000000000 ) ) ;
#36602 = LINE ( 'NONE', #24212, #23202 ) ;
#36603 = CARTESIAN_POINT ( 'NONE',  ( -16.18247977474496224, 122.8183540351560907, 0.6517309543831908414 ) ) ;
#36604 = EDGE_CURVE ( 'NONE', #17420, #19292, #21492, .T. ) ;
#36605 = CARTESIAN_POINT ( 'NONE',  ( 5.111951166545567027, 11.99449087320206431, 6.736519543253151276 ) ) ;
#36606 = CARTESIAN_POINT ( 'NONE',  ( 1.501069045181515849, 120.4980338609919386, 0.3776272143368912815 ) ) ;
#36607 = DIRECTION ( 'NONE',  ( -5.206863593109713661E-17, 1.000000000000000000, -1.077750396879097183E-30 ) ) ;
#36608 = EDGE_CURVE ( 'NONE', #27525, #42131, #5558, .T. ) ;
#36609 = CARTESIAN_POINT ( 'NONE',  ( 11.47343314416673010, 118.8698716516685465, -0.3113556051519839607 ) ) ;
#36610 = CARTESIAN_POINT ( 'NONE',  ( 4.745385786424318297, 117.8992089115141226, -0.7661195729942593680 ) ) ;
#36611 = CARTESIAN_POINT ( 'NONE',  ( -56.16217148015365268, 4.421972936757549100, 2.364476696496186303 ) ) ;
#36612 = CARTESIAN_POINT ( 'NONE',  ( -50.25741847910705928, 21.95975045971864503, 0.7628348698132231265 ) ) ;
#36613 = CARTESIAN_POINT ( 'NONE',  ( -4.323668712555765126, 118.1588900175947856, 0.5145642005610773229 ) ) ;
#36614 = CARTESIAN_POINT ( 'NONE',  ( -52.76912830878634253, 12.08540908813377612, 4.334427935445234858 ) ) ;
#36615 = CARTESIAN_POINT ( 'NONE',  ( -58.58875816907507783, -0.2095754749432666153, 0.4896725462942392304 ) ) ;
#36616 = CARTESIAN_POINT ( 'NONE',  ( -4.366622630093331736, 118.1827404141456128, 0.4454535902724743313 ) ) ;
#36617 = CARTESIAN_POINT ( 'NONE',  ( 4.369338447829433925, 112.0483952545421857, -2.684113968122932459 ) ) ;
#36618 = VERTEX_POINT ( 'NONE', #11092 ) ;
#36619 = CARTESIAN_POINT ( 'NONE',  ( -41.45218294293373162, 22.69057396248467384, 1.547390787314418592 ) ) ;
#36620 = CARTESIAN_POINT ( 'NONE',  ( -6.022744270120071519, 119.3729936414536326, -1.265161215359080327 ) ) ;
#36621 = CARTESIAN_POINT ( 'NONE',  ( -4.746159770738358041, 112.7696648386057632, -2.567419849205245796 ) ) ;
#36622 = CARTESIAN_POINT ( 'NONE',  ( 4.467051862462757761, 118.1153619260469156, 0.7452539832175895107 ) ) ;
#36623 = CARTESIAN_POINT ( 'NONE',  ( -8.365438877267290962, 122.6561726160659731, -0.7803013885889897860 ) ) ;
#36624 = CARTESIAN_POINT ( 'NONE',  ( -0.8282417804140018713, 115.7028554972107059, -1.753370426095431256 ) ) ;
#36625 = CARTESIAN_POINT ( 'NONE',  ( 1.626927334713244466, 117.3993836556012269, -1.397841868528616249 ) ) ;
#36626 = CARTESIAN_POINT ( 'NONE',  ( 2.177262389793235720, 106.6864334246082961, -4.884315812310542348 ) ) ;
#36627 = CARTESIAN_POINT ( 'NONE',  ( -10.07755082079049025, 123.5826510519420509, -1.213607387526569159 ) ) ;
#36628 = CARTESIAN_POINT ( 'NONE',  ( -13.34597544948414694, 17.14500000000000313, -5.016499999999999737 ) ) ;
#36629 = CARTESIAN_POINT ( 'NONE',  ( -46.92937102808930661, 20.25120335581494047, 4.971330492147314928 ) ) ;
#36630 = CARTESIAN_POINT ( 'NONE',  ( 8.321979263998503740, 120.1320355853846991, -1.118248183737061696 ) ) ;
#36631 = CARTESIAN_POINT ( 'NONE',  ( -10.39508997167191495, 153.1476119741804496, -0.08737454559994831116 ) ) ;
#36632 = CARTESIAN_POINT ( 'NONE',  ( -5.591535794131393899, 65.03215273817657760, -1.269999999999993801 ) ) ;
#36633 = CARTESIAN_POINT ( 'NONE',  ( 16.47501798513116000, 155.2380866766625047, 1.211716152346587583 ) ) ;
#36634 = CARTESIAN_POINT ( 'NONE',  ( -4.835467458963106147, 104.6144662015457385, 0.09735812545712563271 ) ) ;
#36635 = CARTESIAN_POINT ( 'NONE',  ( 2.867866294591228993, -15.05265924143639467, 4.220695585399262484 ) ) ;
#36636 = CARTESIAN_POINT ( 'NONE',  ( -4.045847121365472532, 157.1622345443605582, 1.633529996401409834 ) ) ;
#36637 = CARTESIAN_POINT ( 'NONE',  ( 0.2395577018624739096, -8.716993574909102094, 0.9436776969787653568 ) ) ;
#36638 = CARTESIAN_POINT ( 'NONE',  ( -22.98914810635016792, 149.5377445326608665, -1.186953142822410268 ) ) ;
#36639 = CARTESIAN_POINT ( 'NONE',  ( -0.9667957141098567631, 26.69201124214932719, -0.1227653459084327853 ) ) ;
#36640 = ORIENTED_EDGE ( 'NONE', *, *, #375, .T. ) ;
#36641 = CARTESIAN_POINT ( 'NONE',  ( -48.35712625370394591, 16.55775765112550602, 2.292466156223448071 ) ) ;
#36642 = CARTESIAN_POINT ( 'NONE',  ( 7.424629525399723207, 123.6670498955208473, 0.1830506623709854119 ) ) ;
#36643 = CARTESIAN_POINT ( 'NONE',  ( -12.22709855250477418, 151.9982576965888654, 0.6666368699087852345 ) ) ;
#36644 = CARTESIAN_POINT ( 'NONE',  ( 4.626636300257242596, -12.70421170364453900, 2.362638098592509284 ) ) ;
#36645 = CARTESIAN_POINT ( 'NONE',  ( 8.163394002857623732, 121.3802920439979118, -0.9196017894915150537 ) ) ;
#36646 = VERTEX_POINT ( 'NONE', #7909 ) ;
#36647 = CARTESIAN_POINT ( 'NONE',  ( -18.85674122909617978, 149.4003703399637288, -2.492295690319126678 ) ) ;
#36648 = VECTOR ( 'NONE', #21543, 1000.000000000000114 ) ;
#36649 = CARTESIAN_POINT ( 'NONE',  ( -4.548286217995207714, 104.6144662015457669, 1.646238831218158616 ) ) ;
#36650 = CARTESIAN_POINT ( 'NONE',  ( 3.219973314159829680, -14.13069947154231620, 2.606357176882864390 ) ) ;
#36651 = LINE ( 'NONE', #33671, #22438 ) ;
#36652 = CARTESIAN_POINT ( 'NONE',  ( 11.18446751737354461, 128.1157469881088105, 0.03160020415517778708 ) ) ;
#36653 = VERTEX_POINT ( 'NONE', #4728 ) ;
#36654 = CARTESIAN_POINT ( 'NONE',  ( -2.353032276821629853, 107.1110135075323200, 4.697993892905302005 ) ) ;
#36656 = EDGE_CURVE ( 'NONE', #28056, #41432, #8315, .T. ) ;
#36655 = CARTESIAN_POINT ( 'NONE',  ( 5.044654562628557493, 113.8200073110732973, 1.826596097189477907 ) ) ;
#36657 = CARTESIAN_POINT ( 'NONE',  ( -5.008948584507882273, 27.92152162925472325, 0.4889012661100834434 ) ) ;
#36658 = EDGE_CURVE ( 'NONE', #6380, #15145, #16832, .T. ) ;
#36659 = CARTESIAN_POINT ( 'NONE',  ( -10.53334313995851801, 65.32054992887103140, 1.524000000000002908 ) ) ;
#36660 = CARTESIAN_POINT ( 'NONE',  ( 11.66036501707579021, 118.7334002725740874, 0.02296568806519975331 ) ) ;
#36661 = AXIS2_PLACEMENT_3D ( 'NONE', #38700, #3344, #22268 ) ;
#36662 = CARTESIAN_POINT ( 'NONE',  ( -30.44847906516384128, 70.61110078258337808, -1.524000000000007571 ) ) ;
#36663 = CARTESIAN_POINT ( 'NONE',  ( 1.689848471312014322, -15.51967327416042863, 5.544298522819651076 ) ) ;
#36664 = CARTESIAN_POINT ( 'NONE',  ( 11.48503488083560597, 55.92196062030126313, 5.016500000000108095 ) ) ;
#36665 = CARTESIAN_POINT ( 'NONE',  ( -2.803395127021860223, 31.26063551530791074, 0.8708390753670086637 ) ) ;
#36666 = CARTESIAN_POINT ( 'NONE',  ( 8.976454200711021514, 119.5326672034033777, 1.412516637748555404 ) ) ;
#36667 = EDGE_LOOP ( 'NONE', ( #35590, #19904, #28281, #16403 ) ) ;
#36668 = CARTESIAN_POINT ( 'NONE',  ( -1.630640499631123452, 19.93121390510496838, -8.274862188801900942 ) ) ;
#36669 = CARTESIAN_POINT ( 'NONE',  ( 8.703198793585960047, 118.2213482221532246, -0.5883035892448743587 ) ) ;
#36670 = CARTESIAN_POINT ( 'NONE',  ( -3.138057391968792409, 117.6701293611589278, -1.012097185230346197 ) ) ;
#36671 = CARTESIAN_POINT ( 'NONE',  ( -5.237832120027548832, 115.7029491485453860, -1.023639123012231034 ) ) ;
#36672 = CARTESIAN_POINT ( 'NONE',  ( -16.02764313970816090, 80.34763903973272647, -1.270000000000001794 ) ) ;
#36673 = CARTESIAN_POINT ( 'NONE',  ( -5.314278422745060126, 105.1224610256965235, 0.4583187270701635785 ) ) ;
#36674 = CARTESIAN_POINT ( 'NONE',  ( -3.998286381996895233, 3.741657206818807424, 2.332027183294827832 ) ) ;
#36675 = DIRECTION ( 'NONE',  ( 0.8745520943968280170, -0.4849315768086480682, 5.361993529360581832E-16 ) ) ;
#36676 = CARTESIAN_POINT ( 'NONE',  ( -4.966115162882106304, 115.6909491485453003, 1.258873721200368445 ) ) ;
#36677 = CARTESIAN_POINT ( 'NONE',  ( 3.236250843111535769, -14.18372432684703099, 3.165927027233770286 ) ) ;
#36678 = CARTESIAN_POINT ( 'NONE',  ( 0.7414234751011252733, 107.0594419416054848, -4.828671665556863779 ) ) ;
#36679 = CARTESIAN_POINT ( 'NONE',  ( -6.911158149689350161, 117.5201695557886410, 0.4259063301137959723 ) ) ;
#36680 = CARTESIAN_POINT ( 'NONE',  ( -5.040295590206522292, 27.95035695144725452, 0.8066306925778705672 ) ) ;
#36681 = DIRECTION ( 'NONE',  ( 5.188838149069472160E-16, -1.699382548006136559E-16, -1.000000000000000000 ) ) ;
#36682 = ORIENTED_EDGE ( 'NONE', *, *, #34822, .T. ) ;
#36683 = CARTESIAN_POINT ( 'NONE',  ( -3.198460053303494366, 104.6144662015424416, -4.272252451844696708 ) ) ;
#36684 = CARTESIAN_POINT ( 'NONE',  ( 4.909888997889673590, -15.31669448615230422, -0.4577950299049654559 ) ) ;
#36685 = CARTESIAN_POINT ( 'NONE',  ( -1.222221009663208457, 118.4063602595805946, 0.6323148984906141745 ) ) ;
#36686 = CARTESIAN_POINT ( 'NONE',  ( 3.745621265272091716, -10.50169880513956322, -2.708184146228840294 ) ) ;
#36687 = DIRECTION ( 'NONE',  ( 1.000000000000000000, -9.627370216492862708E-17, 0.000000000000000000 ) ) ;
#36688 = CARTESIAN_POINT ( 'NONE',  ( 0.7595712053400294206, 120.2878791493615296, 0.5727019010319394088 ) ) ;
#36689 = CARTESIAN_POINT ( 'NONE',  ( -0.8098364334002190468, 156.6562795458349910, 1.088908734543433177 ) ) ;
#36690 = CARTESIAN_POINT ( 'NONE',  ( -47.61268983602954563, 19.67534098009182841, 5.209569014970943712 ) ) ;
#36691 = VECTOR ( 'NONE', #39985, 1000.000000000000114 ) ;
#36692 = CARTESIAN_POINT ( 'NONE',  ( 11.83945725349111910, 123.3160021321619695, -1.255757047829673789 ) ) ;
#36693 = AXIS2_PLACEMENT_3D ( 'NONE', #39876, #27079, #40087 ) ;
#36694 = CARTESIAN_POINT ( 'NONE',  ( -4.042996894205825420, 118.2594131075661608, -0.9467780975002213495 ) ) ;
#36695 = DIRECTION ( 'NONE',  ( 4.017660918040594346E-17, -1.000000000000000000, -2.376309959284832031E-19 ) ) ;
#36696 = ORIENTED_EDGE ( 'NONE', *, *, #15920, .T. ) ;
#36697 = CARTESIAN_POINT ( 'NONE',  ( 4.293837942828126586, 118.2142420844534172, -0.3502869236174088741 ) ) ;
#36698 = CARTESIAN_POINT ( 'NONE',  ( 0.6885929357777421655, 156.3445873232922736, -0.4144571531603682968 ) ) ;
#36699 = VERTEX_POINT ( 'NONE', #35353 ) ;
#36700 = CARTESIAN_POINT ( 'NONE',  ( 3.040187153003802933, -14.59799761600802448, -0.3075781077882258630 ) ) ;
#36701 = LINE ( 'NONE', #40740, #40185 ) ;
#36702 = CARTESIAN_POINT ( 'NONE',  ( -55.35389262108063235, 6.100188123704747056, 2.822635004243398971 ) ) ;
#36703 = EDGE_CURVE ( 'NONE', #4510, #5052, #38552, .T. ) ;
#36704 = CARTESIAN_POINT ( 'NONE',  ( 4.382351430540762927, 4.226039240006542741, -1.512498627010908647 ) ) ;
#36705 = CARTESIAN_POINT ( 'NONE',  ( 3.490201360801168384, 120.2313485970928326, 0.6717870626964186354 ) ) ;
#36706 = CARTESIAN_POINT ( 'NONE',  ( -2.669449998271343993, 31.09737671526713143, 0.9610299433493049159 ) ) ;
#36707 = CARTESIAN_POINT ( 'NONE',  ( 4.326043401919948295, 8.289558097378858292, -1.648119079657388353 ) ) ;
#36708 = CARTESIAN_POINT ( 'NONE',  ( 15.37864313207198208, 147.8292851303062321, 0.3583584359702445266 ) ) ;
#36709 = CARTESIAN_POINT ( 'NONE',  ( -24.26619908708081041, 81.70586579672512073, -1.524000000000006239 ) ) ;
#36710 = VECTOR ( 'NONE', #37956, 1000.000000000000114 ) ;
#36711 = CARTESIAN_POINT ( 'NONE',  ( -55.14069116334859189, 5.401725095812784261, -9.794129604158680367E-15 ) ) ;
#36712 = CARTESIAN_POINT ( 'NONE',  ( -5.549029403653766401, 116.7532827020298072, -0.3649044722746688230 ) ) ;
#36713 = CARTESIAN_POINT ( 'NONE',  ( 0.0002200197269699131770, 124.8375573595198063, -0.01101068683960091353 ) ) ;
#36714 = ORIENTED_EDGE ( 'NONE', *, *, #41474, .T. ) ;
#36715 = CARTESIAN_POINT ( 'NONE',  ( -15.77830307927088604, 80.39606975582424297, 1.269999999999997575 ) ) ;
#36716 = CARTESIAN_POINT ( 'NONE',  ( -14.60888863026623952, 79.54114996201613508, -1.270000000000000906 ) ) ;
#36717 = CARTESIAN_POINT ( 'NONE',  ( -29.57263912055365296, 58.75010695897971402, -1.524000000000004906 ) ) ;
#36718 = CARTESIAN_POINT ( 'NONE',  ( 8.391957350906555035, -2.082342975431243026, 0.7039615705134369961 ) ) ;
#36719 = DIRECTION ( 'NONE',  ( -0.9998004120163608288, 0.000000000000000000, -0.01997839162482749342 ) ) ;
#36720 = PLANE ( 'NONE',  #15051 ) ;
#36721 = CARTESIAN_POINT ( 'NONE',  ( -58.46425016648313999, 0.8496528882456222398, 0.7404953295986751449 ) ) ;
#36722 = DIRECTION ( 'NONE',  ( -0.1469470846586743706, -9.335746474409589170E-17, 0.9891443546370348727 ) ) ;
#36723 = CARTESIAN_POINT ( 'NONE',  ( -15.71820687823864304, 121.0099257824619627, 0.007297392930742367494 ) ) ;
#36724 = ORIENTED_EDGE ( 'NONE', *, *, #36240, .F. ) ;
#36725 = CARTESIAN_POINT ( 'NONE',  ( -57.66243511465493299, 3.255537196535568611, -1.068383054469936886E-14 ) ) ;
#36726 = CARTESIAN_POINT ( 'NONE',  ( 7.797685292537829049, 122.5814106518984943, -0.01624766703686477201 ) ) ;
#36727 = ORIENTED_EDGE ( 'NONE', *, *, #18928, .T. ) ;
#36728 = CARTESIAN_POINT ( 'NONE',  ( -5.293395377538041124, 115.7029491485389769, -0.7213471474272098449 ) ) ;
#36729 = CARTESIAN_POINT ( 'NONE',  ( -15.26129097679461921, 148.0152273645666980, -0.3559380457717281621 ) ) ;
#36730 = CARTESIAN_POINT ( 'NONE',  ( 4.984919470525341012, -14.71752327621497791, 4.178560682339194976 ) ) ;
#36731 = CARTESIAN_POINT ( 'NONE',  ( -12.96767020122751646, 121.2479969211051127, 1.095090382205327284 ) ) ;
#36732 = CARTESIAN_POINT ( 'NONE',  ( -2.768688662514669385, 30.30441277318858440, -3.700580903672975097 ) ) ;
#36733 = CARTESIAN_POINT ( 'NONE',  ( 0.3142790036445871626, 116.6413645472259617, 0.2007485675953370186 ) ) ;
#36734 = CARTESIAN_POINT ( 'NONE',  ( -0.002141067027474409870, 156.3034662015459446, 0.1071477492456789499 ) ) ;
#36735 = CARTESIAN_POINT ( 'NONE',  ( -29.82668814030757787, 58.78177181444144139, 1.269999999999993578 ) ) ;
#36736 = CARTESIAN_POINT ( 'NONE',  ( 0.6269268744496204748, 0.2942410971610713855, -0.7472855871245592807 ) ) ;
#36737 = CARTESIAN_POINT ( 'NONE',  ( -15.99642297876449604, 121.2237126890796191, -0.5535212332769010590 ) ) ;
#36738 = DIRECTION ( 'NONE',  ( -5.206863593109713661E-17, 1.000000000000000000, -1.077750396879097183E-30 ) ) ;
#36739 = CARTESIAN_POINT ( 'NONE',  ( 4.973583767358946695, 117.3966162183520510, 0.9753880923065370023 ) ) ;
#36740 = EDGE_LOOP ( 'NONE', ( #9899, #12783, #19554, #19805 ) ) ;
#36741 = CARTESIAN_POINT ( 'NONE',  ( 8.737166540455065800, 117.9300049749956827, 0.7016146402485585742 ) ) ;
#36742 = CARTESIAN_POINT ( 'NONE',  ( -17.96630583390862057, 147.4621342421176848, 1.576657649719084064 ) ) ;
#36743 = CARTESIAN_POINT ( 'NONE',  ( -58.10440571236197371, 0.2782998738747570200, -0.7125144706669881423 ) ) ;
#36744 = ADVANCED_FACE ( 'NONE', ( #15742 ), #42026, .T. ) ;
#36745 = CARTESIAN_POINT ( 'NONE',  ( 6.974227900756624798, 158.0922581832940921, 1.731937547952115519 ) ) ;
#36746 = CARTESIAN_POINT ( 'NONE',  ( 19.74506706576308090, 148.5147687316951135, -1.724011100433735955 ) ) ;
#36747 = CARTESIAN_POINT ( 'NONE',  ( 0.1402366131884419942, -14.11417690215759713, -0.9622292808001302600 ) ) ;
#36748 = CARTESIAN_POINT ( 'NONE',  ( -7.913941031674717408, 118.5968412048868288, -1.173277403367298355 ) ) ;
#36749 = CARTESIAN_POINT ( 'NONE',  ( -43.24646561529713296, 21.63922848039483071, -2.381786957946274264 ) ) ;
#36750 = CARTESIAN_POINT ( 'NONE',  ( 5.262484858994872283, 104.6144662015456959, 0.9373981974370197978 ) ) ;
#36751 = ADVANCED_FACE ( 'NONE', ( #41549 ), #15540, .T. ) ;
#36752 = VECTOR ( 'NONE', #21684, 1000.000000000000000 ) ;
#36753 = CARTESIAN_POINT ( 'NONE',  ( 10.06202586252257980, 123.8737202207250618, -0.7052144931501600489 ) ) ;
#36754 = CARTESIAN_POINT ( 'NONE',  ( 7.839459231152404506, 122.3084256158383880, 0.7153501415338812119 ) ) ;
#36755 = EDGE_LOOP ( 'NONE', ( #31097, #25271, #9921, #17651, #35100, #12306, #17602, #14973, #13053, #24483, #33659, #39136, #21270, #16019, #8711, #5830, #38129, #3332, #33873, #19211, #23770, #17076, #8006, #820, #35162, #12421, #37468, #21696, #13557, #28601, #31280, #31715, #38369, #20904, #20931, #38919, #33378, #24098, #33721, #19642, #2427, #42147, #12246, #27552, #26170, #36570, #16341, #31160, #14103, #11202, #30090, #9383, #17374, #21673, #37687, #24187, #30696, #27472, #26550, #11476, #2557, #20698, #28309, #15533, #3813, #13184, #17886, #11415, #3495, #26571, #4218, #400, #21196, #27605, #2635, #41116 ) ) ;
#36756 = CARTESIAN_POINT ( 'NONE',  ( -0.5061634396316659901, 119.4440140289964774, -0.5640781084940279522 ) ) ;
#36757 = CARTESIAN_POINT ( 'NONE',  ( 4.902411944313367798, -15.42400938342815309, 0.6670879667284028702 ) ) ;
#36758 = DIRECTION ( 'NONE',  ( -0.8745520943968240202, 0.4849315768086551737, -5.361993529360572958E-16 ) ) ;
#36759 = CARTESIAN_POINT ( 'NONE',  ( -4.384749978537653803, 118.1630025941448849, -0.6641520118282725482 ) ) ;
#36760 = EDGE_CURVE ( 'NONE', #276, #39424, #23540, .T. ) ;
#36761 = CARTESIAN_POINT ( 'NONE',  ( -55.60508136934060275, 7.116827924314645060, -3.170888472016298198 ) ) ;
#36762 = DIRECTION ( 'NONE',  ( 4.017660918040594346E-17, -1.000000000000000000, -2.376309959284834438E-19 ) ) ;
#36763 = CARTESIAN_POINT ( 'NONE',  ( 10.71425622041610204, 122.7614441063800399, 1.568315134061841087 ) ) ;
#36764 = DIRECTION ( 'NONE',  ( -1.000000000000000000, -9.299908063537918137E-16, 0.000000000000000000 ) ) ;
#36765 = CARTESIAN_POINT ( 'NONE',  ( 23.21373371908085304, 149.6306211361744829, 0.4638656453230914356 ) ) ;
#36766 = CARTESIAN_POINT ( 'NONE',  ( 7.178138493693461797, 8.485180552427815215, -4.444891729080387321 ) ) ;
#36767 = CARTESIAN_POINT ( 'NONE',  ( 9.178653662903458965, 123.9301100385560943, 0.5015510438870898202 ) ) ;
#36768 = EDGE_CURVE ( 'NONE', #26876, #27491, #32502, .T. ) ;
#36769 = CARTESIAN_POINT ( 'NONE',  ( 19.19817178191683027, 128.6826163344482268, -0.7403421610261617936 ) ) ;
#36770 = CARTESIAN_POINT ( 'NONE',  ( 5.871452009091314039, 57.14999999999998437, 5.016499999999999737 ) ) ;
#36771 = AXIS2_PLACEMENT_3D ( 'NONE', #31086, #5541, #31291 ) ;
#36772 = CARTESIAN_POINT ( 'NONE',  ( 0.9748426025018137597, 115.6909491485452719, 1.750969170851022216 ) ) ;
#36773 = CARTESIAN_POINT ( 'NONE',  ( -58.28497307353763546, -0.1385909279409125450, 0.01567725181048698277 ) ) ;
#36774 = CARTESIAN_POINT ( 'NONE',  ( -5.750520748247168079, 159.1178304044242964, -0.06386070104996817431 ) ) ;
#36775 = ORIENTED_EDGE ( 'NONE', *, *, #38896, .F. ) ;
#36776 = EDGE_CURVE ( 'NONE', #40888, #17420, #38969, .T. ) ;
#36777 = CARTESIAN_POINT ( 'NONE',  ( -47.36536141536632982, 24.59964078100214380, -1.062456689557177203 ) ) ;
#36778 = CARTESIAN_POINT ( 'NONE',  ( 5.628418590827510393, 120.8807329490735043, -0.4524337895730209391 ) ) ;
#36779 = CARTESIAN_POINT ( 'NONE',  ( -47.06702646257116385, 25.34112732371119137, -1.513569369951335286 ) ) ;
#36780 = ORIENTED_EDGE ( 'NONE', *, *, #31099, .T. ) ;
#36781 = DIRECTION ( 'NONE',  ( 0.9816537812491076265, 0.1906721105965138718, 4.769617732184456426E-16 ) ) ;
#36782 = CARTESIAN_POINT ( 'NONE',  ( -6.481656071630233384, 121.7133186976561205, -0.3761587846782801225 ) ) ;
#36783 = CARTESIAN_POINT ( 'NONE',  ( 4.598504975971844821, -12.83055836278033901, 2.569316529143384820 ) ) ;
#36784 = CARTESIAN_POINT ( 'NONE',  ( -22.19718911286656393, 149.5167998366165989, 0.9981983707184386434 ) ) ;
#36785 = CARTESIAN_POINT ( 'NONE',  ( -25.77058783747419213, 72.83664265955201245, -1.270000000000005569 ) ) ;
#36786 = CARTESIAN_POINT ( 'NONE',  ( 15.52158573417665544, 120.7153972339879715, 0.3606909788719011578 ) ) ;
#36787 = CIRCLE ( 'NONE', #18388, 0.3809999999999984510 ) ;
#36788 = ORIENTED_EDGE ( 'NONE', *, *, #4277, .F. ) ;
#36789 = CARTESIAN_POINT ( 'NONE',  ( 2.551540157903699146, -0.3564265548712530207, -3.854280124997286450 ) ) ;
#36790 = ADVANCED_FACE ( 'NONE', ( #25133 ), #23527, .T. ) ;
#36791 = CARTESIAN_POINT ( 'NONE',  ( -21.90516586211597883, 151.4314113202728436, -0.4630247046772878461 ) ) ;
#36792 = CARTESIAN_POINT ( 'NONE',  ( 13.77279150232676130, 16.85108474679722690, 5.016499999999997961 ) ) ;
#36793 = ORIENTED_EDGE ( 'NONE', *, *, #12262, .F. ) ;
#36794 = CARTESIAN_POINT ( 'NONE',  ( -6.620801883579276570, 119.9392975627847733, 0.9773581895118412799 ) ) ;
#36795 = CARTESIAN_POINT ( 'NONE',  ( 2.198398128136354934, 2.077049112184502278, 4.064154346441791965 ) ) ;
#36796 = CARTESIAN_POINT ( 'NONE',  ( -0.01887972822151342753, 159.3676309965788960, 0.9448188026860502298 ) ) ;
#36797 = CARTESIAN_POINT ( 'NONE',  ( -58.07568876781230216, 0.3868594689444180834, -1.028118745741293028 ) ) ;
#36799 = CARTESIAN_POINT ( 'NONE',  ( 15.93384955644675038, 125.3951846505478329, -1.286024093939968305 ) ) ;
#36798 = CARTESIAN_POINT ( 'NONE',  ( -28.36525985791271154, 77.02308833105713859, -1.270000000000007345 ) ) ;
#36800 = CARTESIAN_POINT ( 'NONE',  ( -4.603752034695621553, -0.9465464349810851497, 0.4006815057252178236 ) ) ;
#36801 = CARTESIAN_POINT ( 'NONE',  ( -12.91997107708633052, 119.9671592456446803, -1.126112081325366443 ) ) ;
#36802 = CIRCLE ( 'NONE', #21794, 0.5080000000000002292 ) ;
#36803 = ADVANCED_FACE ( 'NONE', ( #30951 ), #10711, .T. ) ;
#36804 = EDGE_LOOP ( 'NONE', ( #26090, #27300, #22079, #2864 ) ) ;
#36805 = CARTESIAN_POINT ( 'NONE',  ( -7.846345427436888897, 154.6110463214094182, 0.1182179892959123735 ) ) ;
#36806 = CARTESIAN_POINT ( 'NONE',  ( 2.663097075550662662, -15.49037753074605739, 5.782289944512356783 ) ) ;
#36807 = VECTOR ( 'NONE', #25174, 1000.000000000000114 ) ;
#36808 = CARTESIAN_POINT ( 'NONE',  ( -43.06611735332018043, 21.60822042109154850, 2.043235477782671783 ) ) ;
#36809 = CARTESIAN_POINT ( 'NONE',  ( -0.3873250690985411970, 117.3993820573415974, -1.495214769458282245 ) ) ;
#36810 = ORIENTED_EDGE ( 'NONE', *, *, #25126, .F. ) ;
#36811 = CARTESIAN_POINT ( 'NONE',  ( 16.83022555070501625, 151.2926467857828072, 2.419188160499603057 ) ) ;
#36812 = CARTESIAN_POINT ( 'NONE',  ( 4.850929972935443146, 117.7610086971114356, 0.9074237114610381738 ) ) ;
#36813 = CARTESIAN_POINT ( 'NONE',  ( -29.37460785692852028, 66.57574643235753342, -1.270000000000006457 ) ) ;
#36814 = CARTESIAN_POINT ( 'NONE',  ( -5.868821994818715027, 117.5931221156369730, 0.5844160582045567764 ) ) ;
#36815 = CARTESIAN_POINT ( 'NONE',  ( 3.644365486686961919, 11.68381519529092216, 7.647779612420950279 ) ) ;
#36816 = CARTESIAN_POINT ( 'NONE',  ( 16.31317273256060574, 147.4903123243063590, 1.598834895054539240 ) ) ;
#36817 = DIRECTION ( 'NONE',  ( 0.2290273297124504059, -0.9734199927291325993, 0.000000000000000000 ) ) ;
#36818 = CARTESIAN_POINT ( 'NONE',  ( 16.70010949199478034, 122.7093839631038463, -0.3053630257279364435 ) ) ;
#36819 = CARTESIAN_POINT ( 'NONE',  ( -6.527452395418614125E-14, 72.48346620154573827, -8.020333044904917549E-18 ) ) ;
#36820 = CARTESIAN_POINT ( 'NONE',  ( -52.55726398868221594, 11.61499462435256547, 4.027787250912923334 ) ) ;
#36821 = CARTESIAN_POINT ( 'NONE',  ( -48.36699572807423664, 24.50126085711046997, 0.4363764532069195901 ) ) ;
#36822 = VECTOR ( 'NONE', #28355, 999.9999999999998863 ) ;
#36823 = CARTESIAN_POINT ( 'NONE',  ( -49.56090548067184898, 17.87959676410238430, 5.165259844110607013 ) ) ;
#36824 = CARTESIAN_POINT ( 'NONE',  ( -58.62245367815513220, -0.2772137513683323173, 0.3975356116906103021 ) ) ;
#36825 = CARTESIAN_POINT ( 'NONE',  ( -4.601694216786480496, 118.0766578999420204, 0.5256003764881748141 ) ) ;
#36826 = CARTESIAN_POINT ( 'NONE',  ( 1.506052270138783067, 106.1074135845622379, -5.119289084907052256 ) ) ;
#36827 = B_SPLINE_SURFACE_WITH_KNOTS ( 'NONE', 1, 3, ( 
 ( #14489, #30684, #1322, #36891, #26869, #27502, #33903, #24085, #40510, #36676, #33273, #39877, #10674, #14279 ),
 ( #4102, #11097, #11304, #27080, #20457, #24289, #37294, #24492, #40088, #20878, #7913, #7709, #27289, #33486 ) ),
 .UNSPECIFIED., .F., .F., .F.,
 ( 2, 2 ),
 ( 4, 3, 2, 2, 3, 4 ),
 ( 0.000000000000000000, 1.000000000000000000 ),
 ( -0.01000000000000000021, 0.000000000000000000, 0.2500000000000000000, 0.5000000000000000000, 1.000000000000000000, 1.016440741388755287 ),
 .UNSPECIFIED. ) ;
#36828 = ORIENTED_EDGE ( 'NONE', *, *, #15270, .T. ) ;
#36829 = CARTESIAN_POINT ( 'NONE',  ( -44.66298991629287940, 23.47648082339880915, 1.964675176939932655 ) ) ;
#36830 = CARTESIAN_POINT ( 'NONE',  ( 3.722225234581910236, 118.8509950637502754, -0.7881369688021256925 ) ) ;
#36831 = CARTESIAN_POINT ( 'NONE',  ( -5.928176885185754585, 118.9717589635377664, -0.5867527899620111898 ) ) ;
#36833 = CARTESIAN_POINT ( 'NONE',  ( 4.458613046552058812, 118.1301588028213985, 0.7148097977274291415 ) ) ;
#36832 = AXIS2_PLACEMENT_3D ( 'NONE', #17407, #34037, #17612 ) ;
#36834 = CARTESIAN_POINT ( 'NONE',  ( -8.219871311007542758, 154.6505398758502849, -1.119353551822956927 ) ) ;
#36835 = DIRECTION ( 'NONE',  ( -4.017660918040594346E-17, 1.000000000000000000, 2.376309959284834438E-19 ) ) ;
#36836 = CARTESIAN_POINT ( 'NONE',  ( 0.5670302775938013129, 118.1651003848106996, -0.8699756239007430114 ) ) ;
#36837 = CARTESIAN_POINT ( 'NONE',  ( 5.120189775498607432, 114.3381464724725447, -1.761508159713760735 ) ) ;
#36838 = CARTESIAN_POINT ( 'NONE',  ( -11.23392777908764550, 153.2158294759273360, -1.564101052410651116 ) ) ;
#36839 = CARTESIAN_POINT ( 'NONE',  ( 4.530977940126489578, 116.0444662015457595, 3.792717828883179543 ) ) ;
#36840 = CARTESIAN_POINT ( 'NONE',  ( -46.34235131104849614, 20.67093754025273356, 4.736928721792746266 ) ) ;
#36841 = CARTESIAN_POINT ( 'NONE',  ( 7.920006352636749902, 122.0419191725283099, -0.5993308652498051670 ) ) ;
#36842 = CARTESIAN_POINT ( 'NONE',  ( -7.772909586817207561, 154.6794531666453167, -0.04377667875137248449 ) ) ;
#36843 = ADVANCED_FACE ( 'NONE', ( #40559 ), #8167, .T. ) ;
#36844 = DIRECTION ( 'NONE',  ( -0.9998004120163608288, 0.000000000000000000, -0.01997839162482747608 ) ) ;
#36845 = CARTESIAN_POINT ( 'NONE',  ( 0.3355986945387293696, 116.9201722098172382, 0.3169108175686568551 ) ) ;
#36846 = CARTESIAN_POINT ( 'NONE',  ( -8.258874273888745066, 69.93630909653145977, 1.270000000000003126 ) ) ;
#36847 = CARTESIAN_POINT ( 'NONE',  ( 3.252851485128089415, -14.73889851401814788, 2.797586445667359811 ) ) ;
#36848 = CARTESIAN_POINT ( 'NONE',  ( -0.01111639999524573208, 119.1634951276629550, 0.5563101126475828995 ) ) ;
#36849 = AXIS2_PLACEMENT_3D ( 'NONE', #13245, #484, #16005 ) ;
#36850 = CARTESIAN_POINT ( 'NONE',  ( -0.9711860326002300647, -2.018343210913434493, -0.07513956953184577903 ) ) ;
#36851 = CARTESIAN_POINT ( 'NONE',  ( -10.56633813141753286, 157.9214973357695158, -0.8874509626871485146 ) ) ;
#36852 = EDGE_CURVE ( 'NONE', #38115, #20064, #28393, .T. ) ;
#36853 = CARTESIAN_POINT ( 'NONE',  ( -0.7929698604315037480, -4.880942799695234591, 0.5714185140920283734 ) ) ;
#36854 = ORIENTED_EDGE ( 'NONE', *, *, #28512, .T. ) ;
#36855 = CARTESIAN_POINT ( 'NONE',  ( -50.84949806483948720, 11.71728973011883923, -8.098653904493606571E-15 ) ) ;
#36856 = CARTESIAN_POINT ( 'NONE',  ( 6.287821989302472048, 120.0808430858776887, 0.4528678087849543066 ) ) ;
#36857 = CONTEXT_DEPENDENT_SHAPE_REPRESENTATION ( #26534, #423 ) ;
#36858 = CARTESIAN_POINT ( 'NONE',  ( -7.681492011331976677, 122.2986020547093915, 0.2830363146464230928 ) ) ;
#36859 = CARTESIAN_POINT ( 'NONE',  ( 4.664530445857379526, -12.43571634592606578, 1.922475882534872449 ) ) ;
#36860 = CARTESIAN_POINT ( 'NONE',  ( 16.72891957527388485, 148.5304741467402323, -1.365449702224203810 ) ) ;
#36861 = ORIENTED_EDGE ( 'NONE', *, *, #36760, .F. ) ;
#36862 = VECTOR ( 'NONE', #37484, 1000.000000000000114 ) ;
#36863 = CARTESIAN_POINT ( 'NONE',  ( -10.89600635431589382, 121.6366708983051836, -1.687201357748379094 ) ) ;
#36864 = CARTESIAN_POINT ( 'NONE',  ( 3.627172221952804865, 115.7029588638002480, 1.619983893740152059 ) ) ;
#36865 = AXIS2_PLACEMENT_3D ( 'NONE', #17731, #21337, #40137 ) ;
#36866 = CARTESIAN_POINT ( 'NONE',  ( 3.131463087139035206, -14.49961247625831895, 3.567833873788547550 ) ) ;
#36867 = CARTESIAN_POINT ( 'NONE',  ( -4.748912967724773004, 117.5371765964522126, -1.178473615865876400 ) ) ;
#36868 = CARTESIAN_POINT ( 'NONE',  ( 0.001255909994464627982, 120.9722815239556439, -0.06285087176068919479 ) ) ;
#36869 = VERTEX_POINT ( 'NONE', #27754 ) ;
#36870 = CARTESIAN_POINT ( 'NONE',  ( -4.875672548457829159, 115.9539541688493642, 1.177672081078976252 ) ) ;
#36871 = CARTESIAN_POINT ( 'NONE',  ( 5.078986093043053707, 94.32746620154571815, 0.1014902294541237954 ) ) ;
#36872 = AXIS2_PLACEMENT_3D ( 'NONE', #3656, #676, #30251 ) ;
#36873 = CARTESIAN_POINT ( 'NONE',  ( -2.613900097597573247, 28.43811729901509722, 0.3641677077667250795 ) ) ;
#36874 = CARTESIAN_POINT ( 'NONE',  ( -17.64290547347870941, 83.78857423953914463, 1.269999999999996021 ) ) ;
#36875 = CARTESIAN_POINT ( 'NONE',  ( 18.61428830734542217, 154.1511370093759865, 0.1565858633853993154 ) ) ;
#36876 = DIRECTION ( 'NONE',  ( 5.188838149069472160E-16, -1.699382548006136559E-16, -1.000000000000000000 ) ) ;
#36877 = CARTESIAN_POINT ( 'NONE',  ( 1.866554170971439275, -15.20651402204141434, 5.950605956638611360 ) ) ;
#36878 = FACE_BOUND ( 'NONE', #13157, .T. ) ;
#36879 = CARTESIAN_POINT ( 'NONE',  ( -3.148634455474565108, 30.89457961443325118, -0.4672107454865901954 ) ) ;
#36880 = CARTESIAN_POINT ( 'NONE',  ( 6.672308397275171110, 157.8130281244853279, 1.874701415657104464 ) ) ;
#36881 = ORIENTED_EDGE ( 'NONE', *, *, #21414, .T. ) ;
#36882 = CARTESIAN_POINT ( 'NONE',  ( -4.342437030201590886, 23.60747082334219371, 7.218840658967335067 ) ) ;
#36883 = CARTESIAN_POINT ( 'NONE',  ( 8.715377116203347541, 118.1578518853687427, -0.5461487580537397468 ) ) ;
#36884 = CARTESIAN_POINT ( 'NONE',  ( -2.726848673931784539, 121.4869043954268903, -0.3408589522888660905 ) ) ;
#36885 = CARTESIAN_POINT ( 'NONE',  ( -5.421568387540222744, 78.92574702321228131, 5.165409981420495455 ) ) ;
#36886 = DIRECTION ( 'NONE',  ( 0.000000000000000000, 0.000000000000000000, 1.000000000000000000 ) ) ;
#36887 = CARTESIAN_POINT ( 'NONE',  ( -0.009645608629898889952, 120.9711055683165597, 0.4827056984856005761 ) ) ;
#36888 = CIRCLE ( 'NONE', #28719, 0.5080000000000000071 ) ;
#36889 = CARTESIAN_POINT ( 'NONE',  ( -4.609222696788063622, 3.091975128091568159, 0.4746723485708761459 ) ) ;
#36890 = DIRECTION ( 'NONE',  ( -5.188838149069472160E-16, 1.699382548006136559E-16, 1.000000000000000000 ) ) ;
#36891 = CARTESIAN_POINT ( 'NONE',  ( -5.276425599434917402, 115.6909491485453003, 0.8138454675775167457 ) ) ;
#36892 = CARTESIAN_POINT ( 'NONE',  ( 3.259676495098780880, -13.96886708669151034, 2.676229364769742158 ) ) ;
#36893 = CARTESIAN_POINT ( 'NONE',  ( 5.433597316833147062, 122.7706071131974994, -0.004560450986766740981 ) ) ;
#36894 = CARTESIAN_POINT ( 'NONE',  ( -22.30840772692687324, 150.5193240506149550, 0.5167903241875736464 ) ) ;
#36895 = CARTESIAN_POINT ( 'NONE',  ( 0.9857937726801648815, 36.25851983645378596, 2.381811577489552523 ) ) ;
#36896 = CARTESIAN_POINT ( 'NONE',  ( -24.57769139521899149, 76.70147894597536720, -1.270000000000005569 ) ) ;
#36897 = ORIENTED_EDGE ( 'NONE', *, *, #14987, .T. ) ;
#36898 = CARTESIAN_POINT ( 'NONE',  ( 4.438132741721911856, -15.66483130081081043, 3.040968155030625120 ) ) ;
#36899 = CARTESIAN_POINT ( 'NONE',  ( -6.741493414765860948, 119.3011930948910759, 1.016225879973854829 ) ) ;
#36900 = EDGE_CURVE ( 'NONE', #24401, #5382, #29763, .T. ) ;
#36901 = CARTESIAN_POINT ( 'NONE',  ( 0.7259983000635549244, 26.63096242550804860, 0.6518668477890779966 ) ) ;
#36902 = ORIENTED_EDGE ( 'NONE', *, *, #34822, .F. ) ;
#36903 = CARTESIAN_POINT ( 'NONE',  ( -3.983954973735330363, 31.42523109854115049, -0.6611907497737663508 ) ) ;
#36904 = CARTESIAN_POINT ( 'NONE',  ( 2.327868625978029016, 124.9344662015457175, 0.04651635516647365659 ) ) ;
#36905 = CARTESIAN_POINT ( 'NONE',  ( -15.52878352361693004, 139.6011575924185877, 1.142358493343924364 ) ) ;
#36906 = CARTESIAN_POINT ( 'NONE',  ( -3.682264917456322895, 63.33946620154573282, -0.07358041635423923088 ) ) ;
#36907 = CIRCLE ( 'NONE', #843, 0.2539999999999978386 ) ;
#36908 = CARTESIAN_POINT ( 'NONE',  ( 16.36721571005495690, 151.0861551944122141, -1.708847769304776110 ) ) ;
#36909 = CARTESIAN_POINT ( 'NONE',  ( 0.03067001211929198945, 158.6015251912307633, -1.534852821454057770 ) ) ;
#36910 = CARTESIAN_POINT ( 'NONE',  ( 20.83467972660109169, 65.95194780259438971, 5.016499999999999737 ) ) ;
#36911 = CARTESIAN_POINT ( 'NONE',  ( 4.170329027945798295, 118.2393515795533148, -0.2194353840718009652 ) ) ;
#36912 = CARTESIAN_POINT ( 'NONE',  ( 0.7006168245643282777, 156.3636429644085695, -0.4970284052464095104 ) ) ;
#36913 = ORIENTED_EDGE ( 'NONE', *, *, #26696, .T. ) ;
#36914 = CARTESIAN_POINT ( 'NONE',  ( 2.463764682325012778, -15.17880951736275108, 4.811303307383569816 ) ) ;
#36915 = CARTESIAN_POINT ( 'NONE',  ( 11.58677707360115861, 55.41127257906217807, -4.474811398756807002 ) ) ;
#36916 = CIRCLE ( 'NONE', #35570, 15.21260244842765452 ) ;
#36917 = CARTESIAN_POINT ( 'NONE',  ( -47.84356795211456870, 19.38525671449504983, 5.197506975155130604 ) ) ;
#36918 = CARTESIAN_POINT ( 'NONE',  ( 1.748379858460863856, 5.525481214791113871, -4.283037568778763848 ) ) ;
#36919 = CARTESIAN_POINT ( 'NONE',  ( 10.21894633145440245, 123.0849000269954701, 1.386333990434162944 ) ) ;
#36920 = CARTESIAN_POINT ( 'NONE',  ( 2.383981540283352629, 36.81846344528510429, 1.803752045214196853 ) ) ;
#36921 = CARTESIAN_POINT ( 'NONE',  ( -7.070147686296687439, 122.4340714744230496, -0.03157745743911240244 ) ) ;
#36922 = CARTESIAN_POINT ( 'NONE',  ( 2.584458374606236841, 15.83607344512877368, 3.832284875798456447 ) ) ;
#36923 = CARTESIAN_POINT ( 'NONE',  ( 3.750075860242078729, 121.0949217282140182, 0.1016972523499030667 ) ) ;
#36924 = CARTESIAN_POINT ( 'NONE',  ( -1.424374813699339715, 106.0672060291940539, 5.142970079757129831 ) ) ;
#36925 = CIRCLE ( 'NONE', #13780, 5.080000000000006288 ) ;
#36926 = CARTESIAN_POINT ( 'NONE',  ( -55.14069116334857767, 5.401725095812811794, -0.2259897844578017678 ) ) ;
#36927 = CARTESIAN_POINT ( 'NONE',  ( 5.560045425373370875, 116.7476357771200242, -0.1303784914585657262 ) ) ;
#36928 = DIRECTION ( 'NONE',  ( -0.8745520943968235761, 0.4849315768086558953, -5.361993529360570985E-16 ) ) ;
#36929 = DIRECTION ( 'NONE',  ( -1.000000000000000000, -6.353134868986659519E-16, 0.000000000000000000 ) ) ;
#36930 = CARTESIAN_POINT ( 'NONE',  ( -0.6790824029981872290, 105.9268256211374393, 5.296885899767392658 ) ) ;
#36931 = CARTESIAN_POINT ( 'NONE',  ( -18.27007371177420936, 83.88799758123168715, -1.270000000000003570 ) ) ;
#36932 = CARTESIAN_POINT ( 'NONE',  ( -3.848622047617309860, 1.169161361801722032, -7.524129562738414378 ) ) ;
#36933 = CARTESIAN_POINT ( 'NONE',  ( -5.353961913965729735, 57.14999999999999858, 5.213928161019513396 ) ) ;
#36934 = CARTESIAN_POINT ( 'NONE',  ( 18.32410244842765934, 17.14499999999999602, 2.244055341071511024E-15 ) ) ;
#36935 = CARTESIAN_POINT ( 'NONE',  ( -57.80399136194962040, 2.779771081967835400, 0.2452555687351543334 ) ) ;
#36936 = CARTESIAN_POINT ( 'NONE',  ( -58.87911280034276018, -0.2081424763510641984, 0.2451831517279786654 ) ) ;
#36937 = CARTESIAN_POINT ( 'NONE',  ( -15.92845220574659315, 121.2232988859741027, 0.005268350931750771793 ) ) ;
#36938 = ORIENTED_EDGE ( 'NONE', *, *, #36776, .T. ) ;
#36939 = CARTESIAN_POINT ( 'NONE',  ( -57.83255607995954506, 2.614142775670388996, -0.5104628509321665897 ) ) ;
#36940 = CARTESIAN_POINT ( 'NONE',  ( -6.068413118431933206, 121.4395679076997823, -0.1212613395058407956 ) ) ;
#36941 = ORIENTED_EDGE ( 'NONE', *, *, #36852, .F. ) ;
#36942 = LINE ( 'NONE', #24345, #38971 ) ;
#36943 = CARTESIAN_POINT ( 'NONE',  ( -8.948282891152253171, 123.9641325482187426, -0.1345489399228556593 ) ) ;
#36944 = CARTESIAN_POINT ( 'NONE',  ( 4.535621022044703743, -15.16026073378742822, 4.605481170969206062 ) ) ;
#36945 = CARTESIAN_POINT ( 'NONE',  ( -11.66006228966227454, 156.3395478113760362, 1.582478695429108351 ) ) ;
#36946 = TOROIDAL_SURFACE ( 'NONE', #10414, 8.794749999999996959, 0.2540000000000000036 ) ;
#36947 = CARTESIAN_POINT ( 'NONE',  ( 15.37635245578016630, 120.8297411738997624, 0.7275678838439408880 ) ) ;
#36948 = CARTESIAN_POINT ( 'NONE',  ( 15.77809098948537780, 146.2329395987594012, 0.5167778558810404155 ) ) ;
#36949 = CARTESIAN_POINT ( 'NONE',  ( -17.14500000000466784, 71.11999999999886768, 1.269999999999998241 ) ) ;
#36950 = B_SPLINE_CURVE_WITH_KNOTS ( 'NONE', 3,
 ( #30017, #23611, #34069, #4896, #24449, #857 ),
 .UNSPECIFIED., .F., .F.,
 ( 4, 2, 4 ),
 ( 0.000000000000000000, 0.1265415849040014140, 0.2530831698080028280 ),
 .UNSPECIFIED. ) ;
#36951 = CARTESIAN_POINT ( 'NONE',  ( -15.55067499035036604, 120.8127473925414108, -0.5415919938617848040 ) ) ;
#36952 = CARTESIAN_POINT ( 'NONE',  ( -49.00328780856283828, 17.83307836943493641, -5.117960591156088590 ) ) ;
#36953 = VERTEX_POINT ( 'NONE', #6039 ) ;
#36954 = CARTESIAN_POINT ( 'NONE',  ( -5.559546751422816513, 116.7637306756996338, 0.1380498186195938948 ) ) ;
#36955 = CARTESIAN_POINT ( 'NONE',  ( -0.02969003158485089208, 157.1787724364823760, 1.485810588193620552 ) ) ;
#36956 = CARTESIAN_POINT ( 'NONE',  ( -57.92782709497848970, 0.6610469618635247402, -0.9517285047954554544 ) ) ;
#36957 = CARTESIAN_POINT ( 'NONE',  ( 0.01152893261307403987, 118.7114655739656257, -0.5769549317675699562 ) ) ;
#36958 = CARTESIAN_POINT ( 'NONE',  ( -0.8939936458071766623, -10.86866097718376523, 0.3889025406916932770 ) ) ;
#36959 = CARTESIAN_POINT ( 'NONE',  ( 0.02615207601215727498, 159.0391464308674756, -1.308756824028193044 ) ) ;
#36960 = EDGE_CURVE ( 'NONE', #5222, #32069, #19838, .T. ) ;
#36961 = CARTESIAN_POINT ( 'NONE',  ( -43.49527490626578441, 22.26612824116996237, -2.150709692269579865 ) ) ;
#36962 = VECTOR ( 'NONE', #13807, 1000.000000000000227 ) ;
#36963 = FACE_OUTER_BOUND ( 'NONE', #30398, .T. ) ;
#36964 = CARTESIAN_POINT ( 'NONE',  ( 11.28744401931954577, 153.2158294759273360, -1.114070445992415781 ) ) ;
#36965 = CARTESIAN_POINT ( 'NONE',  ( -0.6412933796113865492, 156.3034662015457741, -0.01281456791805602943 ) ) ;
#36966 = ORIENTED_EDGE ( 'NONE', *, *, #22254, .T. ) ;
#36967 = CARTESIAN_POINT ( 'NONE',  ( -11.51381720411944620, 123.3156264706956478, -1.674137098916062438 ) ) ;
#36968 = CARTESIAN_POINT ( 'NONE',  ( 4.580902669819289841, -15.62468711146633460, 2.622166941725792899 ) ) ;
#36969 = DIRECTION ( 'NONE',  ( 9.627370216492862708E-17, 1.000000000000000000, -0.000000000000000000 ) ) ;
#36970 = CARTESIAN_POINT ( 'NONE',  ( -4.388233089188608105, 118.1817579657902542, -0.5768122195966850496 ) ) ;
#36971 = CARTESIAN_POINT ( 'NONE',  ( -49.19743978460682143, 17.65503563884207594, -5.190924102448302158 ) ) ;
#36972 = CARTESIAN_POINT ( 'NONE',  ( -17.08598887363762131, 83.79821757228496892, 1.523999999999996469 ) ) ;
#36973 = CARTESIAN_POINT ( 'NONE',  ( 12.17039870458260076, 124.2599011343719155, 1.750469281869919014 ) ) ;
#36974 = DIRECTION ( 'NONE',  ( -1.000000000000000000, 0.000000000000000000, 0.000000000000000000 ) ) ;
#36975 = AXIS2_PLACEMENT_3D ( 'NONE', #39134, #35944, #32107 ) ;
#36976 = CARTESIAN_POINT ( 'NONE',  ( 15.56076557482319700, 120.7233670659379214, 0.3109411287488704767 ) ) ;
#36977 = CARTESIAN_POINT ( 'NONE',  ( -4.930748812479134990, 13.88268055242722987, 6.853499169485068876 ) ) ;
#36978 = CARTESIAN_POINT ( 'NONE',  ( 9.378755113003604649, 124.2036136473707018, 0.5113998741172594009 ) ) ;
#36979 = AXIS2_PLACEMENT_3D ( 'NONE', #31446, #34653, #30813 ) ;
#36980 = CARTESIAN_POINT ( 'NONE',  ( 20.14555658732719934, 152.4688535085772685, -0.7444337660854590810 ) ) ;
#36981 = DIRECTION ( 'NONE',  ( 0.08575086330566537851, 4.464930482241040583E-18, 0.9963166110440663248 ) ) ;
#36982 = CARTESIAN_POINT ( 'NONE',  ( 0.3689803932068112524, 115.6909491485452719, 1.766244566112858738 ) ) ;
#36983 = AXIS2_PLACEMENT_3D ( 'NONE', #305, #13275, #36495 ) ;
#36984 = CARTESIAN_POINT ( 'NONE',  ( -57.53554607470949378, 1.398951746849091959, 0.8928682508385403782 ) ) ;
#36985 = CARTESIAN_POINT ( 'NONE',  ( -23.43370484584250590, 146.8275480241000253, -0.3132885061830181783 ) ) ;
#36986 = ORIENTED_EDGE ( 'NONE', *, *, #3012, .T. ) ;
#36987 = CARTESIAN_POINT ( 'NONE',  ( -46.68395179480138779, 26.03198510454123848, -1.524000000000008015 ) ) ;
#36988 = CARTESIAN_POINT ( 'NONE',  ( -7.868921389075623551, 122.1502739528543771, -0.8431891051951234672 ) ) ;
#36989 = PLANE ( 'NONE',  #30534 ) ;
#36990 = CARTESIAN_POINT ( 'NONE',  ( -4.757248700628498916, 117.4032733054477973, -1.206458840162573543 ) ) ;
#36991 = CARTESIAN_POINT ( 'NONE',  ( -14.33905310436375480, 139.0340687859245463, -0.7442083991839666401 ) ) ;
#36992 = CARTESIAN_POINT ( 'NONE',  ( 4.995837928452414367, -12.01622098921958859, 1.211524600846092481 ) ) ;
#36993 = CARTESIAN_POINT ( 'NONE',  ( -21.01108318401078279, 151.1643092826112138, 1.006483555388256290 ) ) ;
#36994 = CARTESIAN_POINT ( 'NONE',  ( -6.758480964575440453, 78.81581826900305998, -3.179117336685193695 ) ) ;
#36995 = CARTESIAN_POINT ( 'NONE',  ( 16.14716650825965161, 121.2501203052637493, 0.3739013473229990669 ) ) ;
#36996 = EDGE_CURVE ( 'NONE', #32811, #6738, #23022, .T. ) ;
#36997 = CARTESIAN_POINT ( 'NONE',  ( -22.98045850745951668, 78.35500052582088415, -1.270000000000005125 ) ) ;
#36998 = CARTESIAN_POINT ( 'NONE',  ( 0.7336086519982951692, 0.2932837538699786251, -4.563195415240439701 ) ) ;
#36999 = EDGE_CURVE ( 'NONE', #7108, #32222, #31124, .T. ) ;
#37000 = CARTESIAN_POINT ( 'NONE',  ( -2.735903701988665393, 116.5290148844309357, -0.06805092059891044987 ) ) ;
#37001 = CARTESIAN_POINT ( 'NONE',  ( -7.213960532363665301, 83.56599999999998829, 1.904999999999995364 ) ) ;
#37002 = CARTESIAN_POINT ( 'NONE',  ( -23.75997692595333177, 82.67351089148900201, 1.269999999999992024 ) ) ;
#37003 = VERTEX_POINT ( 'NONE', #16432 ) ;
#37004 = CARTESIAN_POINT ( 'NONE',  ( -6.655208740269098477, 120.0178561674164115, 0.9687501452866643659 ) ) ;
#37005 = CARTESIAN_POINT ( 'NONE',  ( -4.027482788729651375, -0.2968512080594384317, 2.264360808822050597 ) ) ;
#37006 = CARTESIAN_POINT ( 'NONE',  ( 22.29769713523675634, 148.9358926463403918, 1.890714429241201922 ) ) ;
#37007 = CARTESIAN_POINT ( 'NONE',  ( -58.67410397513807396, -0.3138866149756391888, -0.3147537707001585860 ) ) ;
#37008 = CARTESIAN_POINT ( 'NONE',  ( 13.89335097268673280, 122.2371923977168109, -1.173247377384143642 ) ) ;
#37009 = AXIS2_PLACEMENT_3D ( 'NONE', #27243, #14444, #11459 ) ;
#37010 = CARTESIAN_POINT ( 'NONE',  ( -4.627572956979934204, -1.171460759993483647, -0.2796867628226345492 ) ) ;
#37011 = CARTESIAN_POINT ( 'NONE',  ( -19.95201466422913228, 152.4248492066682559, -1.669502467017324632 ) ) ;
#37012 = ORIENTED_EDGE ( 'NONE', *, *, #931, .T. ) ;
#37014 = VECTOR ( 'NONE', #19248, 1000.000000000000000 ) ;
#37013 = CARTESIAN_POINT ( 'NONE',  ( -4.566879893416770031, 121.1702857069421100, 0.02052890071062577274 ) ) ;
#37015 = CARTESIAN_POINT ( 'NONE',  ( 2.110383923269381512, -15.54165552008020335, 5.912460941884730481 ) ) ;
#37016 =( BOUNDED_CURVE ( )  B_SPLINE_CURVE ( 3, ( #38126, #9357, #35560, #29366 ),
 .UNSPECIFIED., .F., .T. ) 
 B_SPLINE_CURVE_WITH_KNOTS ( ( 4, 4 ),
 ( 0.0001874388305180640468, 0.2498838476046065793 ),
 .UNSPECIFIED. ) 
 CURVE ( )  GEOMETRIC_REPRESENTATION_ITEM ( )  RATIONAL_B_SPLINE_CURVE ( ( 0.9999925516704997186, 0.6670664864091201407, 0.5004025452935453311, 0.5000007283237750677 ) ) 
 REPRESENTATION_ITEM ( '' )  );
#37017 = DIRECTION ( 'NONE',  ( -0.8745520943968245753, 0.4849315768086539524, -5.691349986800526185E-16 ) ) ;
#37018 = AXIS2_PLACEMENT_3D ( 'NONE', #17276, #23868, #30265 ) ;
#37019 = CARTESIAN_POINT ( 'NONE',  ( -0.4922460975656830495, 117.3993826272291869, -1.493757915153530735 ) ) ;
#37020 = VERTEX_POINT ( 'NONE', #32004 ) ;
#37021 = CARTESIAN_POINT ( 'NONE',  ( 18.97908907040207538, 145.0145856610025987, 2.515253529532921917 ) ) ;
#37022 = DIRECTION ( 'NONE',  ( -0.9876665170007969952, 0.1565721916417935344, -5.390917751951444915E-16 ) ) ;
#37023 = AXIS2_PLACEMENT_3D ( 'NONE', #28778, #12997, #32819 ) ;
#37024 = CARTESIAN_POINT ( 'NONE',  ( -4.792324638262678960, 56.51998046905272588, 4.972049999962470324 ) ) ;
#37025 = CARTESIAN_POINT ( 'NONE',  ( -3.102616959202407099, 159.2904672602661549, 0.8345756338990469869 ) ) ;
#37027 = EDGE_CURVE ( 'NONE', #38485, #32125, #39277, .T. ) ;
#37026 = CARTESIAN_POINT ( 'NONE',  ( 8.086262078954034038, 3.373778641329666872, 2.357548046588672008 ) ) ;
#37028 = CARTESIAN_POINT ( 'NONE',  ( 9.985636026282364242, 124.1433363813624311, 1.001463123883985729 ) ) ;
#37029 = LINE ( 'NONE', #8249, #1573 ) ;
#37030 = CARTESIAN_POINT ( 'NONE',  ( 14.51632629332712909, 120.3567457872619997, -0.2133257594814960689 ) ) ;
#37031 = DIRECTION ( 'NONE',  ( -5.188838149069472160E-16, 1.699382548006136559E-16, 1.000000000000000000 ) ) ;
#37032 = CARTESIAN_POINT ( 'NONE',  ( -57.54159257952407103, 1.494932415318306340, 1.359492011164181946 ) ) ;
#37033 = CARTESIAN_POINT ( 'NONE',  ( -57.57967628038989005, 1.451576601202181349, 1.494865757154131725 ) ) ;
#37034 = CARTESIAN_POINT ( 'NONE',  ( -57.61954905543894512, 1.880482199989210956, 1.716091637445736007 ) ) ;
#37035 = CARTESIAN_POINT ( 'NONE',  ( -4.170396868163473769, 118.2393519985668746, 0.2194165179955171185 ) ) ;
#37036 = CARTESIAN_POINT ( 'NONE',  ( -5.078986093043186045, 88.48546620154573361, -0.1014902294541231709 ) ) ;
#37037 = ORIENTED_EDGE ( 'NONE', *, *, #13059, .T. ) ;
#37038 = CARTESIAN_POINT ( 'NONE',  ( -41.88683177698051452, 22.33947639032530219, 1.656270940288490312 ) ) ;
#37039 = CARTESIAN_POINT ( 'NONE',  ( 8.289722630716616081, 120.2889166620582131, -1.113928890953434170 ) ) ;
#37040 = CARTESIAN_POINT ( 'NONE',  ( -5.608813212978156493, 117.9149360781225937, -0.7492264055198124550 ) ) ;
#37041 = CARTESIAN_POINT ( 'NONE',  ( 4.155982282308561260, 118.2394341885533038, 0.3882798843181367032 ) ) ;
#37042 = CARTESIAN_POINT ( 'NONE',  ( -16.16038979459568381, 146.4165046419237228, -1.293905914731260598 ) ) ;
#37043 = SURFACE_SIDE_STYLE ('',( #11043 ) ) ;
#37044 = CARTESIAN_POINT ( 'NONE',  ( 4.425820884885741435, 117.3993836135481530, -1.092143121358476687 ) ) ;
#37045 = EDGE_CURVE ( 'NONE', #32933, #11474, #16011, .T. ) ;
#37046 = ORIENTED_EDGE ( 'NONE', *, *, #32458, .T. ) ;
#37047 = CARTESIAN_POINT ( 'NONE',  ( 5.292163649236448109, 116.0761519159950552, -1.031159682278862233 ) ) ;
#37048 = CARTESIAN_POINT ( 'NONE',  ( -4.757797086070440606, 156.0326374431741385, -1.238355579604159873 ) ) ;
#37049 = DIRECTION ( 'NONE',  ( -1.224646799147353207E-16, 1.239092185628910643E-32, 1.000000000000000000 ) ) ;
#37050 = CARTESIAN_POINT ( 'NONE',  ( -45.09675090431021260, 21.02858785303205380, 3.680331723257769028 ) ) ;
#37051 = CARTESIAN_POINT ( 'NONE',  ( -10.28897677580358305, 57.14999999999998437, -5.016499999999999737 ) ) ;
#37052 = CARTESIAN_POINT ( 'NONE',  ( 7.784012322544599627, 122.6313477034872506, 0.1555430911242069170 ) ) ;
#37053 = DIRECTION ( 'NONE',  ( 4.017660918040594346E-17, -1.000000000000000000, -2.376309959284834438E-19 ) ) ;
#37054 = CARTESIAN_POINT ( 'NONE',  ( 15.49230080900811402, 121.3130774642648220, 1.004719031932798767 ) ) ;
#37055 = CARTESIAN_POINT ( 'NONE',  ( 5.241362157049057835, 53.58606249999999704, -5.310945289804168468 ) ) ;
#37056 = CARTESIAN_POINT ( 'NONE',  ( 3.208040786519721355, -14.49217647381938257, 1.686337311097440894 ) ) ;
#37057 = CARTESIAN_POINT ( 'NONE',  ( -2.342076541036599124, 157.5529522918930638, 1.611985001046909005 ) ) ;
#37058 = CARTESIAN_POINT ( 'NONE',  ( 0.7944722411588411859, -7.641519016208866866, 0.5639076281424253434 ) ) ;
#37059 = CARTESIAN_POINT ( 'NONE',  ( -7.903286925170654342, 158.6683511845044734, -0.6884992853041225214 ) ) ;
#37060 = CARTESIAN_POINT ( 'NONE',  ( -0.9746272421432693456, 17.39786500698104277, 0.06925455797152506310 ) ) ;
#37061 = ORIENTED_EDGE ( 'NONE', *, *, #28462, .T. ) ;
#37062 = EDGE_CURVE ( 'NONE', #29590, #16766, #34547, .T. ) ;
#37063 = CARTESIAN_POINT ( 'NONE',  ( -50.34589867275522579, 15.36027825638806910, 4.364407372394862428 ) ) ;
#37064 = PRODUCT_CONTEXT ( 'NONE', #25165, 'mechanical' ) ;
#37065 = CARTESIAN_POINT ( 'NONE',  ( -2.740744172220349384, 120.7841308545065431, 0.2151145298216796120 ) ) ;
#37066 = CARTESIAN_POINT ( 'NONE',  ( 4.431203275146504694, -13.68733396499126265, 3.949578922469492603 ) ) ;
#37067 = CARTESIAN_POINT ( 'NONE',  ( 8.085704850285637235, 121.5393406094847819, -0.8545391641419386453 ) ) ;
#37068 = ORIENTED_EDGE ( 'NONE', *, *, #4319, .F. ) ;
#37069 = CARTESIAN_POINT ( 'NONE',  ( -3.347088983278076579, 104.6144662015457811, 3.489637925767542725 ) ) ;
#37070 = CARTESIAN_POINT ( 'NONE',  ( 3.347306494706169477, -13.94864326390300668, 3.303819676456750898 ) ) ;
#37071 = CARTESIAN_POINT ( 'NONE',  ( -4.957019470562856078, 117.4692298950752161, -0.9989214207450358707 ) ) ;
#37072 = CARTESIAN_POINT ( 'NONE',  ( 15.79259660498968643, 146.2429432508320417, 0.1870566092231163435 ) ) ;
#37073 = ORIENTED_EDGE ( 'NONE', *, *, #6562, .F. ) ;
#37074 = CARTESIAN_POINT ( 'NONE',  ( 20.22999339756068693, 148.7458375694471044, 2.474301912364148315 ) ) ;
#37075 = CARTESIAN_POINT ( 'NONE',  ( 1.300340531814593081, 106.1074135845529582, 5.175367491933112518 ) ) ;
#37076 = CARTESIAN_POINT ( 'NONE',  ( -5.180755175387888656, 27.96082930289568935, 0.4723356417371947225 ) ) ;
#37077 = DIRECTION ( 'NONE',  ( 0.3213437296502729135, -0.9469626219732499850, 2.623573200068682142E-15 ) ) ;
#37078 = CARTESIAN_POINT ( 'NONE',  ( 23.09707919911549467, 149.8924475812327159, 0.2317116236470735946 ) ) ;
#37079 = EDGE_CURVE ( 'NONE', #19701, #929, #39541, .T. ) ;
#37080 = LINE ( 'NONE', #21276, #6388 ) ;
#37081 = EDGE_CURVE ( 'NONE', #10127, #41143, #13251, .T. ) ;
#37082 = CARTESIAN_POINT ( 'NONE',  ( 1.759694577103611213, -15.65007286489543326, 5.607714211663698656 ) ) ;
#37083 = DIRECTION ( 'NONE',  ( -0.9998004120163609398, 0.000000000000000000, -0.01997839162482749689 ) ) ;
#37084 = CARTESIAN_POINT ( 'NONE',  ( -4.980269422504584043, 117.5911954193708908, -0.7465893992053445061 ) ) ;
#37085 = CARTESIAN_POINT ( 'NONE',  ( 20.51324802173755657, 148.8605967840894095, 2.436527653975322227 ) ) ;
#37086 = ORIENTED_EDGE ( 'NONE', *, *, #41075, .T. ) ;
#37087 = CARTESIAN_POINT ( 'NONE',  ( 2.510961470319720501, 15.29743382693132148, 8.092466016612050339 ) ) ;
#37088 = CARTESIAN_POINT ( 'NONE',  ( -8.586090317502511837, 118.6238329966567306, -1.141930902790657898 ) ) ;
#37089 = CARTESIAN_POINT ( 'NONE',  ( -3.197921176416423261, 118.4615047536228047, -0.7906167528392610278 ) ) ;
#37090 = CARTESIAN_POINT ( 'NONE',  ( 4.973153598853037316, 117.3993852231080268, 0.9753024529967266876 ) ) ;
#37091 = CARTESIAN_POINT ( 'NONE',  ( -4.724244202807499349, 117.6625551699878827, -1.131988795082268240 ) ) ;
#37092 = CARTESIAN_POINT ( 'NONE',  ( -4.572702043008527895, 104.6144662015325224, 2.768430063960745979 ) ) ;
#37093 = CARTESIAN_POINT ( 'NONE',  ( -4.157303687089163979, 2.242350289152962528, -2.029258473605290103 ) ) ;
#37094 = DIRECTION ( 'NONE',  ( 0.4849315768086534528, 0.8745520943968249084, 1.030032898892974818E-16 ) ) ;
#37095 = FACE_OUTER_BOUND ( 'NONE', #18400, .T. ) ;
#37096 = CARTESIAN_POINT ( 'NONE',  ( 3.188489192988832155, -14.31930622237681483, 3.473944028487384372 ) ) ;
#37097 = CARTESIAN_POINT ( 'NONE',  ( 4.210090452738473488, 118.4033805524614849, -0.5735154781215827668 ) ) ;
#37098 = EDGE_CURVE ( 'NONE', #2129, #22153, #11381, .T. ) ;
#37099 = CARTESIAN_POINT ( 'NONE',  ( 1.928079173006373104, 38.28172739177303896, 1.429945915702467651 ) ) ;
#37100 = CARTESIAN_POINT ( 'NONE',  ( 10.28897677580358128, 57.14999999999999858, 5.016499999999999737 ) ) ;
#37101 = ORIENTED_EDGE ( 'NONE', *, *, #31623, .T. ) ;
#37102 = CARTESIAN_POINT ( 'NONE',  ( -5.344453801630723255, 105.1225221600350466, 0.1077189844379473072 ) ) ;
#37103 = CARTESIAN_POINT ( 'NONE',  ( 4.930802857217395641, -15.55747185075553851, 2.516589264972601825 ) ) ;
#37104 = CARTESIAN_POINT ( 'NONE',  ( -4.459427130834483499, 157.7533977378147654, 1.670975814381038926 ) ) ;
#37105 = CARTESIAN_POINT ( 'NONE',  ( -0.6497956273327881727, 21.66276798020532013, -0.7290388503713802759 ) ) ;
#37106 = EDGE_LOOP ( 'NONE', ( #6935, #2903, #23230, #28967 ) ) ;
#37107 = EDGE_LOOP ( 'NONE', ( #28022, #2261, #24954, #1034 ) ) ;
#37108 = CARTESIAN_POINT ( 'NONE',  ( 0.007549346801170758389, 106.0530876078258586, 5.266739608401566741 ) ) ;
#37109 = CARTESIAN_POINT ( 'NONE',  ( -10.28583081752403139, 123.7737839053064022, 0.8195368008302437168 ) ) ;
#37110 = FACE_OUTER_BOUND ( 'NONE', #19260, .T. ) ;
#37111 = CARTESIAN_POINT ( 'NONE',  ( 17.99030040960589005, 148.1388135707062474, -1.617688361210429582 ) ) ;
#37112 = CARTESIAN_POINT ( 'NONE',  ( -13.20682171306295238, 121.8780043825237982, -1.728041046422398086 ) ) ;
#37113 = FACE_OUTER_BOUND ( 'NONE', #21028, .T. ) ;
#37114 = CARTESIAN_POINT ( 'NONE',  ( 4.246255474397634622, 118.2246697035938752, -0.3144686129305331868 ) ) ;
#37115 = CARTESIAN_POINT ( 'NONE',  ( 9.260187833317498729, 153.8817031120973411, -0.3320757922997037426 ) ) ;
#37116 = ADVANCED_FACE ( 'NONE', ( #26235 ), #23161, .T. ) ;
#37117 = ORIENTED_EDGE ( 'NONE', *, *, #37635, .F. ) ;
#37118 = CARTESIAN_POINT ( 'NONE',  ( 3.044219152853963717, -14.30162947539197127, 0.8262259773895895831 ) ) ;
#37119 = CARTESIAN_POINT ( 'NONE',  ( 10.96186877710200491, 56.39406130473815892, -5.016499999999892268 ) ) ;
#37120 = CARTESIAN_POINT ( 'NONE',  ( -57.97024931889899335, 0.5691613924951877124, 0.8993266954188116058 ) ) ;
#37121 = CARTESIAN_POINT ( 'NONE',  ( -1.146732334619779969, -3.095543821355960734, -4.488006035213349953 ) ) ;
#37122 = CARTESIAN_POINT ( 'NONE',  ( 1.917342111448682607, 156.7095495334699535, 1.310369884728257217 ) ) ;
#37123 = CARTESIAN_POINT ( 'NONE',  ( -0.01131193556908014278, 32.98573834278982986, 2.219894021788903160 ) ) ;
#37124 = CARTESIAN_POINT ( 'NONE',  ( -4.405468973772928010, 113.1344509532474376, 2.291157639236350185 ) ) ;
#37125 = EDGE_CURVE ( 'NONE', #26682, #13736, #20224, .T. ) ;
#37126 = CARTESIAN_POINT ( 'NONE',  ( -4.151662239014343392, 13.23730288530712862, 2.070234887608822572 ) ) ;
#37127 = CARTESIAN_POINT ( 'NONE',  ( 10.40832821182515033, 153.0987333575537548, 0.3246753324606913016 ) ) ;
#37128 = CARTESIAN_POINT ( 'NONE',  ( -11.11710224467008601, 56.30409367656574915, 5.016499999999452619 ) ) ;
#37129 = EDGE_CURVE ( 'NONE', #37552, #35632, #4607, .T. ) ;
#37130 = CARTESIAN_POINT ( 'NONE',  ( -57.85534701229749999, 0.8496279762696401505, -1.203237356453227491 ) ) ;
#37131 = CARTESIAN_POINT ( 'NONE',  ( -8.783221293945311814, 117.7336977213016382, -0.4113777022403178329 ) ) ;
#37132 = CARTESIAN_POINT ( 'NONE',  ( 11.66725022231030984, 16.51000000000000156, 5.016499999999999737 ) ) ;
#37133 = CARTESIAN_POINT ( 'NONE',  ( -46.89253820722738908, 25.40240703814324164, -1.700804414715234580 ) ) ;
#37134 = CARTESIAN_POINT ( 'NONE',  ( 1.896617635523347944, -15.61750365820154407, 5.464805439086086736 ) ) ;
#37135 = CARTESIAN_POINT ( 'NONE',  ( -31.58045816364236202, 52.93464387108262059, -1.524000000000004906 ) ) ;
#37136 = CARTESIAN_POINT ( 'NONE',  ( -2.691543149356179665, 0.9405793051805824145, -7.980626778548312927 ) ) ;
#37137 = CARTESIAN_POINT ( 'NONE',  ( -8.594951744493888768, 74.76616009375631222, -1.523999999999996913 ) ) ;
#37138 = DIRECTION ( 'NONE',  ( -0.9998004118909472604, 1.039228058384960363E-20, -0.01997839790104462970 ) ) ;
#37139 = CARTESIAN_POINT ( 'NONE',  ( -57.92935616279446265, 2.416188466839983118, 0.2259612492381935789 ) ) ;
#37140 = CARTESIAN_POINT ( 'NONE',  ( -5.010144981628188887, 117.3993855238222608, -0.7522679339500687457 ) ) ;
#37141 = CARTESIAN_POINT ( 'NONE',  ( -23.20995092461745202, 148.9919839608952827, 0.1323997120335726196 ) ) ;
#37142 = ORIENTED_EDGE ( 'NONE', *, *, #25382, .F. ) ;
#37143 = CARTESIAN_POINT ( 'NONE',  ( -57.42300747107054093, 3.318281940618617032, -1.876676483338179491 ) ) ;
#37144 = EDGE_LOOP ( 'NONE', ( #24133, #22559, #21465, #4703 ) ) ;
#37145 = CARTESIAN_POINT ( 'NONE',  ( -45.60639265695031952, 20.98815520443264404, -4.238054969593709309 ) ) ;
#37146 = CARTESIAN_POINT ( 'NONE',  ( -15.38000172822634326, 147.8312228277220868, -0.3073290368998167210 ) ) ;
#37147 = CARTESIAN_POINT ( 'NONE',  ( 6.371418708240476292, -13.42079056852439578, 0.8326245159988630018 ) ) ;
#37148 = CARTESIAN_POINT ( 'NONE',  ( -4.057542840006509444, 118.1249481555716301, 0.7600096289331684796 ) ) ;
#37149 = CARTESIAN_POINT ( 'NONE',  ( 11.13388036866224873, 119.2389763063149388, -0.6860836662663821750 ) ) ;
#37150 = LINE ( 'NONE', #17542, #6742 ) ;
#37151 = CARTESIAN_POINT ( 'NONE',  ( -8.041834545247111166, 158.6767594643193604, -0.3248513814034965641 ) ) ;
#37152 = CARTESIAN_POINT ( 'NONE',  ( -49.56431242325176356, 16.98212490189121127, -5.014837167102403015 ) ) ;
#37153 = ORIENTED_EDGE ( 'NONE', *, *, #26154, .T. ) ;
#37154 = CIRCLE ( 'NONE', #3844, 0.2540000000000000591 ) ;
#37155 = CARTESIAN_POINT ( 'NONE',  ( 5.559147133327456025, 116.7105361058337252, 0.2236709051713111351 ) ) ;
#37156 = CARTESIAN_POINT ( 'NONE',  ( -7.347594966877752043, 120.9764928074160082, 0.8683198564056586743 ) ) ;
#37157 = CARTESIAN_POINT ( 'NONE',  ( -58.19031870555688357, 0.09256663605368072034, -0.5720079524431537221 ) ) ;
#37158 = CARTESIAN_POINT ( 'NONE',  ( 2.466025220844119126, 157.8629595415303584, -1.630325060746250498 ) ) ;
#37159 = CARTESIAN_POINT ( 'NONE',  ( 0.8685042297821888857, -7.415843212509670934, 0.4410767154842855642 ) ) ;
#37160 = CARTESIAN_POINT ( 'NONE',  ( -1.224709079186641514, 159.1407128229522527, -1.247756218451904209 ) ) ;
#37161 = CARTESIAN_POINT ( 'NONE',  ( -47.16890147375937659, 22.20336809214646578, -4.187060126831891438 ) ) ;
#37162 = CARTESIAN_POINT ( 'NONE',  ( 15.62653493684484651, 149.1167355181319181, -1.114087811593069688 ) ) ;
#37163 = CARTESIAN_POINT ( 'NONE',  ( -6.439802323014594534E-14, 156.3034662015457172, 9.765829976239106842E-17 ) ) ;
#37164 = B_SPLINE_CURVE_WITH_KNOTS ( 'NONE', 5,
 ( #41670, #31006, #18424, #25254, #18852, #9076 ),
 .UNSPECIFIED., .F., .F.,
 ( 6, 6 ),
 ( 0.000000000000000000, 0.2175306174020106287 ),
 .UNSPECIFIED. ) ;
#37165 = ORIENTED_EDGE ( 'NONE', *, *, #37062, .T. ) ;
#37166 = CARTESIAN_POINT ( 'NONE',  ( -17.12878219156706905, 140.2562023718666353, -2.330665938063504417 ) ) ;
#37167 = CARTESIAN_POINT ( 'NONE',  ( 4.104683988343100332, -15.63859574289259946, 3.129333468668611840 ) ) ;
#37168 = PLANE ( 'NONE',  #27191 ) ;
#37169 = CARTESIAN_POINT ( 'NONE',  ( -4.274993567701977248, 118.2142329864754799, -0.5231303911420034369 ) ) ;
#37170 = CARTESIAN_POINT ( 'NONE',  ( -52.42133349025997546, 11.92692459785933679, -4.172736198742198255 ) ) ;
#37171 = CARTESIAN_POINT ( 'NONE',  ( -4.932986805861466095, 117.5466154476640952, 0.8856657162804417727 ) ) ;
#37172 = CARTESIAN_POINT ( 'NONE',  ( 3.791208754741518305, 156.9018388488748883, 1.699278904607349094 ) ) ;
#37173 = DIRECTION ( 'NONE',  ( 1.000000000000000000, 0.000000000000000000, 0.000000000000000000 ) ) ;
#37174 = CARTESIAN_POINT ( 'NONE',  ( 22.53527615164620101, 150.7831677823008363, 0.4503084484864737225 ) ) ;
#37175 = ADVANCED_FACE ( 'NONE', ( #20252 ), #1115, .F. ) ;
#37176 = CARTESIAN_POINT ( 'NONE',  ( 8.243228241119590294, 17.55835651096333194, -1.765626013165721320 ) ) ;
#37177 = CARTESIAN_POINT ( 'NONE',  ( 15.85571122620632245, 146.2799285973741519, 0.7709397856434243579 ) ) ;
#37178 = CARTESIAN_POINT ( 'NONE',  ( 1.589478822742971486E-15, 16.51000000000000156, 0.000000000000000000 ) ) ;
#37179 = AXIS2_PLACEMENT_3D ( 'NONE', #33308, #17098, #7120 ) ;
#37180 = CARTESIAN_POINT ( 'NONE',  ( -45.90302585792993284, 20.78970012321159899, -4.334318749026735418 ) ) ;
#37181 = DIRECTION ( 'NONE',  ( -0.8745520943968235761, 0.4849315768086558953, -5.361993529360570985E-16 ) ) ;
#37182 = CARTESIAN_POINT ( 'NONE',  ( -57.37715403173692152, 1.618736692213004869, 0.5106765013061003167 ) ) ;
#37183 = CARTESIAN_POINT ( 'NONE',  ( -4.735783051744410166, 116.7698466342620378, -0.01422048256815223663 ) ) ;
#37184 = ORIENTED_EDGE ( 'NONE', *, *, #32083, .F. ) ;
#37185 = CARTESIAN_POINT ( 'NONE',  ( -47.31580374228550312, 25.16323110364244897, -0.6294670755810810592 ) ) ;
#37186 = CARTESIAN_POINT ( 'NONE',  ( 6.902403728792015691, 121.7324704480519983, -0.3323477824281221849 ) ) ;
#37187 = CARTESIAN_POINT ( 'NONE',  ( -8.764399874728846740, 117.8902759020840421, 0.3181776094565136881 ) ) ;
#37188 = VERTEX_POINT ( 'NONE', #33278 ) ;
#37189 = CARTESIAN_POINT ( 'NONE',  ( 3.259383964624091412, 115.6909491485452435, -1.531612751755973223 ) ) ;
#37190 = CARTESIAN_POINT ( 'NONE',  ( -5.263358945736734462, 121.3020066425206807, -0.2711714534586359138 ) ) ;
#37191 = CARTESIAN_POINT ( 'NONE',  ( 2.546550616605329775, -14.95902107118821078, 5.737972450990987738 ) ) ;
#37192 = CARTESIAN_POINT ( 'NONE',  ( -21.13693409061731998, 150.2702755442954583, 1.277357359820448846 ) ) ;
#37193 = AXIS2_PLACEMENT_3D ( 'NONE', #9598, #16183, #6415 ) ;
#37194 = CARTESIAN_POINT ( 'NONE',  ( 4.801338745261147345, 117.3993836135855275, -1.016148444996444189 ) ) ;
#37195 = CARTESIAN_POINT ( 'NONE',  ( 0.3005257795022526213, 116.4832816433156069, 0.09989594597631686057 ) ) ;
#37196 = CARTESIAN_POINT ( 'NONE',  ( 15.38000172822621536, 147.8312228277220868, 0.3073290368998169431 ) ) ;
#37197 = ORIENTED_EDGE ( 'NONE', *, *, #33925, .F. ) ;
#37198 = CARTESIAN_POINT ( 'NONE',  ( -0.1020318426323372635, 30.30579279289823802, -0.9687052925327788166 ) ) ;
#37199 = CARTESIAN_POINT ( 'NONE',  ( -8.078287538471746743, 158.6595088495342338, -0.1614234102745197019 ) ) ;
#37200 = CARTESIAN_POINT ( 'NONE',  ( -41.41133299024001246, 23.09032428891222111, -1.527002492031612979 ) ) ;
#37201 = EDGE_LOOP ( 'NONE', ( #41099, #3594, #13967, #41117 ) ) ;
#37202 = CARTESIAN_POINT ( 'NONE',  ( 3.456281358658134906, 50.63946620154572997, 1.847419665314800064 ) ) ;
#37203 = ORIENTED_EDGE ( 'NONE', *, *, #406, .T. ) ;
#37204 = CARTESIAN_POINT ( 'NONE',  ( 8.451590122553549023, 119.2591792085226103, 1.352863054565908607 ) ) ;
#37205 = CARTESIAN_POINT ( 'NONE',  ( 3.951836011467571907, -5.044640503713330837, -2.394960105287299523 ) ) ;
#37206 = CARTESIAN_POINT ( 'NONE',  ( 21.80375291804136140, 148.4185114426368841, 2.147915116047498962 ) ) ;
#37207 = CARTESIAN_POINT ( 'NONE',  ( -58.82991071597902533, -0.2577532384650527142, -9.114074148744775817E-15 ) ) ;
#37208 = TOROIDAL_SURFACE ( 'NONE', #33149, 3.683000000000000718, 0.5080000000000000071 ) ;
#37209 = CARTESIAN_POINT ( 'NONE',  ( 14.68166051447191123, 123.3142630313093377, -1.213898157370195241 ) ) ;
#37210 = CARTESIAN_POINT ( 'NONE',  ( -0.05192310401019068627, -8.293124787585329116, 4.627658001227512585 ) ) ;
#37211 = CARTESIAN_POINT ( 'NONE',  ( -5.840790351889599386, 117.5931221156369730, -0.8184019802203832405 ) ) ;
#37212 = CARTESIAN_POINT ( 'NONE',  ( 4.793196582158109287, 117.7334801314650008, -0.8915230911338991593 ) ) ;
#37213 = ORIENTED_EDGE ( 'NONE', *, *, #27356, .F. ) ;
#37214 = TOROIDAL_SURFACE ( 'NONE', #28364, 0.3809999999999990616, 0.2540000000000000036 ) ;
#37215 = CARTESIAN_POINT ( 'NONE',  ( -15.57078937218329173, 147.5402044622178153, 0.01782986306386609779 ) ) ;
#37216 = CARTESIAN_POINT ( 'NONE',  ( 4.375071722208805802, -15.20633266255931559, 4.762636924185132514 ) ) ;
#37217 = CARTESIAN_POINT ( 'NONE',  ( -18.88649316419433788, 79.99958772249931371, 1.269999999999996021 ) ) ;
#37218 = CARTESIAN_POINT ( 'NONE',  ( -4.824733838022108756, 115.9539541688524622, -1.371509286363743030 ) ) ;
#37219 = VERTEX_POINT ( 'NONE', #701 ) ;
#37220 = CARTESIAN_POINT ( 'NONE',  ( 18.69815986816969655, 149.1225091032880528, 2.485088035475524038 ) ) ;
#37221 = CARTESIAN_POINT ( 'NONE',  ( -3.174366308152013705, 104.6144662015457243, -0.06343139340882732180 ) ) ;
#37222 = AXIS2_PLACEMENT_3D ( 'NONE', #41669, #2902, #9075 ) ;
#37223 = CARTESIAN_POINT ( 'NONE',  ( -2.940475496281335310, 117.1197906563906344, 0.4390297717439134995 ) ) ;
#37224 = CARTESIAN_POINT ( 'NONE',  ( 8.413794655563325620, 13.29309125005104164, 0.5966991197660089785 ) ) ;
#37225 = CARTESIAN_POINT ( 'NONE',  ( 16.14046266016579878, 146.7365623387580342, 1.292066526867236220 ) ) ;
#37226 = CARTESIAN_POINT ( 'NONE',  ( 1.650612623617701257E-15, 17.14499999999999957, 0.000000000000000000 ) ) ;
#37227 = CARTESIAN_POINT ( 'NONE',  ( 11.52575769572317377, 118.8226552325407397, -0.2321966025152968904 ) ) ;
#37228 = CARTESIAN_POINT ( 'NONE',  ( 4.825452542548434920, 117.8355215987486275, -0.7438749666106165837 ) ) ;
#37229 = VECTOR ( 'NONE', #30352, 1000.000000000000000 ) ;
#37230 = CARTESIAN_POINT ( 'NONE',  ( -52.99508395989393250, 10.78319250833652809, 3.865765426181710041 ) ) ;
#37231 = DIRECTION ( 'NONE',  ( 0.8745520943968235761, -0.4849315768086558398, 4.268512490100410909E-16 ) ) ;
#37232 = CARTESIAN_POINT ( 'NONE',  ( -58.60752282809816904, -0.1920500713008393978, 0.6598870774482750168 ) ) ;
#37233 = CARTESIAN_POINT ( 'NONE',  ( -58.61247718564857223, -0.2580816525627335767, 0.4259738903449781788 ) ) ;
#37234 = CARTESIAN_POINT ( 'NONE',  ( -4.246359198923776113, 118.2246726177936580, 0.3144336963837771615 ) ) ;
#37235 = CARTESIAN_POINT ( 'NONE',  ( 1.969389160195163857, 106.3931338143290475, -4.957017173386934594 ) ) ;
#37236 = AXIS2_PLACEMENT_3D ( 'NONE', #19420, #36051, #19622 ) ;
#37237 = ORIENTED_EDGE ( 'NONE', *, *, #33876, .F. ) ;
#37238 = CARTESIAN_POINT ( 'NONE',  ( -53.65759266121656879, 11.01975743955735432, 4.003319250743206936 ) ) ;
#37239 = CARTESIAN_POINT ( 'NONE',  ( -4.228505362209877383, 119.3620910118516321, -0.9269648930420215649 ) ) ;
#37240 = CARTESIAN_POINT ( 'NONE',  ( -5.028795574735199558, 114.3519703858145959, -1.961426316196308361 ) ) ;
#37241 = CARTESIAN_POINT ( 'NONE',  ( 4.340305978642269302, 118.1815293345206896, 0.6239748096490277396 ) ) ;
#37242 = CARTESIAN_POINT ( 'NONE',  ( -16.06762827093127299, 146.3760696504137684, -1.175121962453930635 ) ) ;
#37243 = CARTESIAN_POINT ( 'NONE',  ( -6.656543858376176668E-14, 104.6144662015457243, -3.850115147268248130E-19 ) ) ;
#37244 = DIRECTION ( 'NONE',  ( 0.7770581983690878491, -0.6294287539883980376, 5.101669463485847584E-16 ) ) ;
#37245 = ORIENTED_EDGE ( 'NONE', *, *, #39652, .T. ) ;
#37246 = CARTESIAN_POINT ( 'NONE',  ( 3.110646482806172397, 107.8085536575111689, -4.359277737140974551 ) ) ;
#37247 = CARTESIAN_POINT ( 'NONE',  ( -15.47075146591473072, 139.6011575924185877, -1.761802977227842293 ) ) ;
#37248 = DIRECTION ( 'NONE',  ( -1.000000000000000000, -1.092739197465705287E-15, 0.000000000000000000 ) ) ;
#37249 = CARTESIAN_POINT ( 'NONE',  ( -46.82131867383161961, 20.47688106639223449, 5.000304862135632966 ) ) ;
#37250 = CARTESIAN_POINT ( 'NONE',  ( -12.21488373879589240, 55.24499999999999034, -5.016499999999999737 ) ) ;
#37251 = CARTESIAN_POINT ( 'NONE',  ( -15.53206457832155785, 147.5381829847979702, -0.1100152830077117949 ) ) ;
#37252 = CARTESIAN_POINT ( 'NONE',  ( -8.519412162535125788, 69.40335734044577976, 1.524000000000003352 ) ) ;
#37253 = CARTESIAN_POINT ( 'NONE',  ( 13.07250590169503823, 156.9444350391594014, 1.084824903291609743 ) ) ;
#37254 = CARTESIAN_POINT ( 'NONE',  ( 5.664977208693820820, 53.58606249999999704, -5.033228321271210781 ) ) ;
#37256 = CARTESIAN_POINT ( 'NONE',  ( 7.994725381675307219, 118.4344479264803169, -0.7928399906090749516 ) ) ;
#37255 = CARTESIAN_POINT ( 'NONE',  ( 3.076715286590720133, -14.17522324541667444, 1.337940584860995319 ) ) ;
#37257 = CARTESIAN_POINT ( 'NONE',  ( -11.72911894083935458, 122.8035986606355152, 1.269020613264102204 ) ) ;
#37258 = CARTESIAN_POINT ( 'NONE',  ( -0.6334066649623988354, -12.81304641701132851, -0.7396855475671405555 ) ) ;
#37259 = CARTESIAN_POINT ( 'NONE',  ( 0.004913308685967637639, 116.7872217978203224, -0.2458820580207658202 ) ) ;
#37260 = CARTESIAN_POINT ( 'NONE',  ( 0.3889013835376298744, 10.72134676413487142, 0.8939893681288630933 ) ) ;
#37261 = ORIENTED_EDGE ( 'NONE', *, *, #21654, .T. ) ;
#37262 = CARTESIAN_POINT ( 'NONE',  ( -52.57757236033170045, 11.11936768914174145, 3.180765541460421897 ) ) ;
#37263 = CARTESIAN_POINT ( 'NONE',  ( -14.97557080935144569, 148.8997249754567349, 0.5399649533830233050 ) ) ;
#37264 = CARTESIAN_POINT ( 'NONE',  ( 4.144384115003134639, -13.99490941865914806, 4.432938699676250316 ) ) ;
#37265 = CARTESIAN_POINT ( 'NONE',  ( 8.809140270325693578, 122.1986804192922875, -0.8245386672919368110 ) ) ;
#37266 = EDGE_LOOP ( 'NONE', ( #40354, #34079, #34537, #20842 ) ) ;
#37267 = CARTESIAN_POINT ( 'NONE',  ( 1.784992122055886199, 115.7029483427795782, 1.723372422334099152 ) ) ;
#37268 = CARTESIAN_POINT ( 'NONE',  ( 2.843374750741399559, -13.00285448706176084, 0.5077109796929276664 ) ) ;
#37269 = DIRECTION ( 'NONE',  ( 0.8745520943968253524, -0.4849315768086530087, 8.537024980200771528E-16 ) ) ;
#37270 = CARTESIAN_POINT ( 'NONE',  ( 11.84655969407677567, 151.9972573545839225, 0.1156591128142185482 ) ) ;
#37271 = ORIENTED_EDGE ( 'NONE', *, *, #34710, .T. ) ;
#37272 = CARTESIAN_POINT ( 'NONE',  ( 14.15513794057036989, 123.4894365733723447, 1.873888081047781595 ) ) ;
#37273 = CARTESIAN_POINT ( 'NONE',  ( 1.247874008749637165, 106.2090255614403276, 5.187965977526303618 ) ) ;
#37274 = CARTESIAN_POINT ( 'NONE',  ( -10.08214312826213721, 118.0934564804969114, -0.2014652138697927419 ) ) ;
#37275 = EDGE_CURVE ( 'NONE', #27765, #5344, #29331, .T. ) ;
#37276 = CARTESIAN_POINT ( 'NONE',  ( 0.03245814172805025488, 157.7902383798253538, -1.624338139048501439 ) ) ;
#37277 = CARTESIAN_POINT ( 'NONE',  ( 21.89150648822671030, 151.4414241944827495, 0.2106634337039131888 ) ) ;
#37278 = CARTESIAN_POINT ( 'NONE',  ( -10.00099186598785650, 77.19260062651656540, 1.524000000000000465 ) ) ;
#37279 = CARTESIAN_POINT ( 'NONE',  ( 1.871143833745863239, -15.59325378310091814, 5.931567052087414638 ) ) ;
#37280 = LINE ( 'NONE', #28102, #6565 ) ;
#37281 = CARTESIAN_POINT ( 'NONE',  ( -14.21338345945963688, 79.68069512491149453, 1.269999999999998241 ) ) ;
#37282 = EDGE_CURVE ( 'NONE', #10652, #25646, #26663, .T. ) ;
#37283 = CARTESIAN_POINT ( 'NONE',  ( -4.720317703858613712, 117.8402133106318246, 0.8448306392985246438 ) ) ;
#37284 = EDGE_LOOP ( 'NONE', ( #28040, #31224, #22140, #5701 ) ) ;
#37285 = CARTESIAN_POINT ( 'NONE',  ( -4.801770124281918406, 117.3993836135855133, 1.016061139389656587 ) ) ;
#37286 = CARTESIAN_POINT ( 'NONE',  ( -2.554268019588743943, 117.5995512635590643, -0.7715010912678383903 ) ) ;
#37287 = CARTESIAN_POINT ( 'NONE',  ( -1.451835205608249080, 110.3135721340718334, -3.567596948272937496 ) ) ;
#37288 = CARTESIAN_POINT ( 'NONE',  ( 4.820214878024821736, 117.6751674563618053, 1.076090311930151255 ) ) ;
#37289 = FACE_OUTER_BOUND ( 'NONE', #40407, .T. ) ;
#37290 = CARTESIAN_POINT ( 'NONE',  ( -0.03040743766756944313, 116.4813942609868178, 1.521712522323421579 ) ) ;
#37291 = VECTOR ( 'NONE', #621, 1000.000000000000000 ) ;
#37292 = CARTESIAN_POINT ( 'NONE',  ( 4.364008504204949013, 7.202613900313124873, 1.580794030135405537 ) ) ;
#37293 = CARTESIAN_POINT ( 'NONE',  ( -3.527324519276147541, 50.63946620154572997, 1.707870599815379364 ) ) ;
#37294 = CARTESIAN_POINT ( 'NONE',  ( -4.815530361150011984, 118.5264896598256854, 0.7999101472927785395 ) ) ;
#37295 = CARTESIAN_POINT ( 'NONE',  ( 3.910559219094527528, -13.09373064504072737, 2.776858670901594994 ) ) ;
#37296 = CARTESIAN_POINT ( 'NONE',  ( 4.048024155119271050, 117.4230540797109938, -0.8140401526052125636 ) ) ;
#37297 = PRODUCT_DEFINITION ( 'UNKNOWN', '', #18251, #6535 ) ;
#37298 = CARTESIAN_POINT ( 'NONE',  ( -3.575185924110746871, 29.88618740006140584, 3.683134272688635580 ) ) ;
#37299 = EDGE_CURVE ( 'NONE', #38754, #37322, #16137, .T. ) ;
#37300 = CARTESIAN_POINT ( 'NONE',  ( -0.5927862973117289380, 115.7030772917255490, 1.739502740807663095 ) ) ;
#37301 = VERTEX_POINT ( 'NONE', #23443 ) ;
#37302 = CARTESIAN_POINT ( 'NONE',  ( -2.612664856745740671, 104.6144662015509681, -4.653567239894925933 ) ) ;
#37303 = CARTESIAN_POINT ( 'NONE',  ( 4.169050558263453610, -15.30144204372030359, -0.4701337638493395255 ) ) ;
#37304 = CARTESIAN_POINT ( 'NONE',  ( -18.61143607275154466, 150.2488615152233820, 1.729315005182988418 ) ) ;
#37305 = CARTESIAN_POINT ( 'NONE',  ( -0.08934464221186895483, 15.61415217803747169, 0.9739947352787643453 ) ) ;
#37306 = ADVANCED_FACE ( 'NONE', ( #29653 ), #20462, .T. ) ;
#37307 = VERTEX_POINT ( 'NONE', #30274 ) ;
#37308 = ORIENTED_EDGE ( 'NONE', *, *, #8984, .F. ) ;
#37309 = LINE ( 'NONE', #34124, #1135 ) ;
#37310 = CARTESIAN_POINT ( 'NONE',  ( 2.266726881631522694, 118.5759350612125900, 0.8281820106640960244 ) ) ;
#37311 = CARTESIAN_POINT ( 'NONE',  ( -3.544426656953535204, 120.3814187630814132, 0.4774784233729821303 ) ) ;
#37312 = DIRECTION ( 'NONE',  ( -6.353134868986659519E-16, 1.000000000000000000, -0.000000000000000000 ) ) ;
#37313 = EDGE_CURVE ( 'NONE', #915, #12580, #14284, .T. ) ;
#37314 = CARTESIAN_POINT ( 'NONE',  ( 4.601497379863265458, 118.0704624899502164, -0.5722604949035791089 ) ) ;
#37315 = CARTESIAN_POINT ( 'NONE',  ( 1.363824289596507588, 119.4570717772418220, -0.5813626927913072562 ) ) ;
#37316 = CARTESIAN_POINT ( 'NONE',  ( -2.213841846844945671, 118.2767885243204944, -0.7726204694312125421 ) ) ;
#37317 = CARTESIAN_POINT ( 'NONE',  ( 11.58677707360137710, 55.24500000000000455, 4.474811398758258285 ) ) ;
#37318 = EDGE_CURVE ( 'NONE', #40156, #22433, #908, .T. ) ;
#37319 = VERTEX_POINT ( 'NONE', #13881 ) ;
#37320 = CARTESIAN_POINT ( 'NONE',  ( 4.116109897646406779, 118.2429491485453354, -0.1887006734943049158 ) ) ;
#37321 = CARTESIAN_POINT ( 'NONE',  ( 14.81827458270670128, 148.8567844064068026, -0.2884810962875100637 ) ) ;
#37322 = VERTEX_POINT ( 'NONE', #11101 ) ;
#37323 = CARTESIAN_POINT ( 'NONE',  ( 3.216700609619024931, -14.42020774479446921, 2.887214088933996337 ) ) ;
#37324 = AXIS2_PLACEMENT_3D ( 'NONE', #27542, #18145, #40131 ) ;
#37325 = VECTOR ( 'NONE', #14266, 1000.000000000000000 ) ;
#37326 = CARTESIAN_POINT ( 'NONE',  ( -5.006118277528749161, 117.4009255802263283, 0.7893014723888780448 ) ) ;
#37327 = CARTESIAN_POINT ( 'NONE',  ( -52.95179419874582294, 11.24610246599371699, 4.133922171299013293 ) ) ;
#37328 = CARTESIAN_POINT ( 'NONE',  ( 1.861163356255745915, -7.643417679262992870, 4.233688895527200735 ) ) ;
#37329 = CARTESIAN_POINT ( 'NONE',  ( 11.93440950959098323, 126.0992317015783328, 1.505959514896210827 ) ) ;
#37330 = CARTESIAN_POINT ( 'NONE',  ( -3.933769473788125026, 27.98561731294367050, 0.4889718192695881038 ) ) ;
#37331 = CARTESIAN_POINT ( 'NONE',  ( -7.563607548680848502, 124.2956292408697863, -0.1420234171030813897 ) ) ;
#37332 = CARTESIAN_POINT ( 'NONE',  ( -1.251853189678833411, -4.679435864505671283, 4.458631606201990394 ) ) ;
#37333 = CARTESIAN_POINT ( 'NONE',  ( 15.22644562805675328, 143.4365109762209158, 0.4329964906482477449 ) ) ;
#37334 = CARTESIAN_POINT ( 'NONE',  ( -11.82906070755491612, 56.41571150956222880, 5.016499999999999737 ) ) ;
#37335 = CARTESIAN_POINT ( 'NONE',  ( -57.23135758994266098, 1.814875683430833275, -0.2588789259697646394 ) ) ;
#37336 = CARTESIAN_POINT ( 'NONE',  ( -5.489085054281237497, 117.1391964092379965, -0.7660907124981986005 ) ) ;
#37337 = CARTESIAN_POINT ( 'NONE',  ( 0.007670926890785616931, 121.5961256765098284, -0.3838845493044710233 ) ) ;
#37338 = DIRECTION ( 'NONE',  ( 5.188838149069472160E-16, -1.699382548006136559E-16, -1.000000000000000000 ) ) ;
#37339 = DIRECTION ( 'NONE',  ( 5.188838149069472160E-16, -1.699382548006136559E-16, -1.000000000000000000 ) ) ;
#37340 = CARTESIAN_POINT ( 'NONE',  ( 0.7770267621822702919, 9.899933826931993863, -8.437367074289049640 ) ) ;
#37341 = CARTESIAN_POINT ( 'NONE',  ( -5.177913976931285411, 57.14999999999999858, -5.372100000000001430 ) ) ;
#37342 = DIRECTION ( 'NONE',  ( 5.188838149069472160E-16, -1.699382548006136559E-16, -1.000000000000000000 ) ) ;
#37343 = DIRECTION ( 'NONE',  ( -0.8745520943968241312, 0.4849315768086547851, -5.271987356194193006E-16 ) ) ;
#37344 = CARTESIAN_POINT ( 'NONE',  ( 0.04081796246445149740, 114.7739974199301969, -2.042697753608868627 ) ) ;
#37345 = CARTESIAN_POINT ( 'NONE',  ( -22.64827982350394464, 150.3405807453409579, 0.2709709482530831548 ) ) ;
#37346 = EDGE_CURVE ( 'NONE', #37301, #16441, #37940, .T. ) ;
#37347 = EDGE_LOOP ( 'NONE', ( #38412, #6159, #19986, #13484 ) ) ;
#37348 = CARTESIAN_POINT ( 'NONE',  ( -58.83227707057486811, -0.08366279997996939333, -5.839471642284167958E-15 ) ) ;
#37349 = AXIS2_PLACEMENT_3D ( 'NONE', #5244, #31418, #30782 ) ;
#37350 = EDGE_CURVE ( 'NONE', #1503, #915, #7994, .T. ) ;
#37351 = ORIENTED_EDGE ( 'NONE', *, *, #15141, .T. ) ;
#37352 = CARTESIAN_POINT ( 'NONE',  ( -47.34495446287286313, 19.93462121980824620, -5.151308439895126767 ) ) ;
#37353 = CARTESIAN_POINT ( 'NONE',  ( -15.52687642492895037, 147.5330934759543879, -0.3102639428822864254 ) ) ;
#37354 = CARTESIAN_POINT ( 'NONE',  ( 5.820489720963992752, -14.55473177801069795, 2.572867947693331381 ) ) ;
#37355 = CARTESIAN_POINT ( 'NONE',  ( -19.67014042257531869, 150.6586468064772646, 1.570413873854537457 ) ) ;
#37356 = CARTESIAN_POINT ( 'NONE',  ( 12.81731082034050573, 120.0678233105195716, -0.7045657984066407975 ) ) ;
#37357 = CARTESIAN_POINT ( 'NONE',  ( -2.136650056307613621, 10.86338872207680950, -4.114640003288728920 ) ) ;
#37358 = CARTESIAN_POINT ( 'NONE',  ( -9.724873038622067867, 118.0756159837034716, -0.5523889259422301024 ) ) ;
#37359 = CARTESIAN_POINT ( 'NONE',  ( -49.47195631129834226, 17.12452434303404303, -5.032791565054547611 ) ) ;
#37360 = FACE_OUTER_BOUND ( 'NONE', #35070, .T. ) ;
#37361 = CARTESIAN_POINT ( 'NONE',  ( -5.322365003949023787, 156.4258374981641282, 1.486226487625613712 ) ) ;
#37362 = CARTESIAN_POINT ( 'NONE',  ( -50.95832625531466675, 14.53658918554379298, -4.553647182183382824 ) ) ;
#37363 = EDGE_CURVE ( 'NONE', #29093, #25607, #23661, .T. ) ;
#37364 = CARTESIAN_POINT ( 'NONE',  ( 0.01133701094394712686, 119.0130636887059410, -0.5673503866435171128 ) ) ;
#37365 = CARTESIAN_POINT ( 'NONE',  ( -0.3947855200659833863, 117.7785671674745771, -0.5311790665990139271 ) ) ;
#37366 = CARTESIAN_POINT ( 'NONE',  ( -46.81005371095109524, 25.73327194510133253, -1.583310528698488984 ) ) ;
#37367 = EDGE_CURVE ( 'NONE', #42131, #11710, #24303, .T. ) ;
#37368 = CARTESIAN_POINT ( 'NONE',  ( 16.05848832435423290, 147.7157881801689427, -0.7882342824236391321 ) ) ;
#37369 = ORIENTED_EDGE ( 'NONE', *, *, #7992, .T. ) ;
#37370 = CARTESIAN_POINT ( 'NONE',  ( 0.03066982525775523508, 157.3074135339440147, -1.534843470138540278 ) ) ;
#37371 = CARTESIAN_POINT ( 'NONE',  ( 3.754758974503722868, -15.60599068302642678, 3.401513958955031836 ) ) ;
#37372 = EDGE_CURVE ( 'NONE', #31966, #2670, #22851, .T. ) ;
#37373 = CARTESIAN_POINT ( 'NONE',  ( -4.426261876493431835, 118.1635320031892178, -0.6236544883123098515 ) ) ;
#37374 = CARTESIAN_POINT ( 'NONE',  ( -57.93941708942283952, 2.052042089854988483, -1.628789306319529118 ) ) ;
#37375 = CARTESIAN_POINT ( 'NONE',  ( -4.997723913362575487, 117.4043970260275813, 0.8231665828273773133 ) ) ;
#37376 = CARTESIAN_POINT ( 'NONE',  ( 2.103759425340601119, 157.1282018749678002, 1.585319646506186730 ) ) ;
#37377 = DIRECTION ( 'NONE',  ( -0.9998004120163608288, -5.205824365704082573E-17, -0.01997839162482749342 ) ) ;
#37378 = AXIS2_PLACEMENT_3D ( 'NONE', #23983, #14601, #7397 ) ;
#37379 = VECTOR ( 'NONE', #35154, 1000.000000000000000 ) ;
#37380 = CARTESIAN_POINT ( 'NONE',  ( 22.83607019214376521, 150.4065277667444036, 0.4307393832409500134 ) ) ;
#37381 = CARTESIAN_POINT ( 'NONE',  ( -8.161197318747062113, 2.438352165997351495, -2.203247879407881804 ) ) ;
#37382 = CARTESIAN_POINT ( 'NONE',  ( 13.65930421665831851, 150.2105054413494543, 0.7115039165091188167 ) ) ;
#37383 = CARTESIAN_POINT ( 'NONE',  ( 0.4044265971210334598, 118.1627375710014007, -0.8899864531652206256 ) ) ;
#37384 = CARTESIAN_POINT ( 'NONE',  ( -41.38112080847943020, 22.74200708568027807, -0.4658591655019068689 ) ) ;
#37385 = CARTESIAN_POINT ( 'NONE',  ( -3.147325619572344468, 118.1588897472110773, 0.6788706689571556430 ) ) ;
#37386 = CARTESIAN_POINT ( 'NONE',  ( -7.819160365854489037, 122.4258430437401159, -0.5979938724132283223 ) ) ;
#37387 = CARTESIAN_POINT ( 'NONE',  ( -57.47393550255003447, 1.325481720219581661, -1.009526220810559183E-14 ) ) ;
#37388 = CARTESIAN_POINT ( 'NONE',  ( -20.69264154312393700, 152.5691845998198346, -0.2640292844866432009 ) ) ;
#37389 = VERTEX_POINT ( 'NONE', #30483 ) ;
#37390 = CARTESIAN_POINT ( 'NONE',  ( -47.23483502501005660, 23.02499599010462816, -3.263444997004429915 ) ) ;
#37391 = CARTESIAN_POINT ( 'NONE',  ( 5.907666735792171053, 121.3440877105034019, -0.1410375414887058143 ) ) ;
#37392 = CARTESIAN_POINT ( 'NONE',  ( -7.784012322544769269, 122.6313477034873074, -0.1555430911242075831 ) ) ;
#37393 = EDGE_LOOP ( 'NONE', ( #4645, #40309, #41371, #29224 ) ) ;
#37394 = CARTESIAN_POINT ( 'NONE',  ( 0.8084953953736374599, 118.7629491485454025, -1.239640985604131274 ) ) ;
#37395 = CARTESIAN_POINT ( 'NONE',  ( -9.106360905785223281, 123.9337093609977529, -0.4112724569044293177 ) ) ;
#37396 = CARTESIAN_POINT ( 'NONE',  ( 4.626636300257242596, -12.70421170364453900, 2.362638098592509284 ) ) ;
#37397 = CARTESIAN_POINT ( 'NONE',  ( -0.02156508032628448243, 159.2730288250082538, 1.079204802879467850 ) ) ;
#37398 = CARTESIAN_POINT ( 'NONE',  ( 1.204770341778093456E-15, 12.51401280605345967, 0.000000000000000000 ) ) ;
#37399 = CARTESIAN_POINT ( 'NONE',  ( 3.735388766124958515, 116.6566025657135413, 0.1875874814615932362 ) ) ;
#37400 = CARTESIAN_POINT ( 'NONE',  ( 11.83237999055733525, 152.0315156623530015, 0.2988832620038224253 ) ) ;
#37401 = CARTESIAN_POINT ( 'NONE',  ( 0.8332047475417917459, 28.58290516567101491, -0.5069163209656499802 ) ) ;
#37402 = CARTESIAN_POINT ( 'NONE',  ( -18.84770637050854347, 125.3331924886369961, -0.3953412214710179673 ) ) ;
#37403 = DIRECTION ( 'NONE',  ( -5.188838149069471174E-16, 1.699382548006136313E-16, 1.000000000000000000 ) ) ;
#37404 = AXIS2_PLACEMENT_3D ( 'NONE', #18761, #36969, #5384 ) ;
#37405 = ORIENTED_EDGE ( 'NONE', *, *, #32873, .T. ) ;
#37406 = DIRECTION ( 'NONE',  ( -0.7548010569845216011, -0.6559537821943317581, -2.801824109679581255E-16 ) ) ;
#37407 = EDGE_LOOP ( 'NONE', ( #5141, #19428, #11907, #27313 ) ) ;
#37408 = CARTESIAN_POINT ( 'NONE',  ( -8.410730074438736992, 119.6967890130903527, 1.093143251542445293 ) ) ;
#37409 = CARTESIAN_POINT ( 'NONE',  ( -17.76856900107737403, 61.81127730225986738, 1.523999999999999133 ) ) ;
#37410 = CARTESIAN_POINT ( 'NONE',  ( 4.887760029584741872, 117.7409041207840090, 0.8724161813180757452 ) ) ;
#37411 = CARTESIAN_POINT ( 'NONE',  ( -58.45128286774109938, -0.4309378487381305689, -0.3205346425646805053 ) ) ;
#37412 = CARTESIAN_POINT ( 'NONE',  ( 19.78169998575264898, 149.7343351798865285, -1.666391814173802777 ) ) ;
#37413 = CARTESIAN_POINT ( 'NONE',  ( -8.287855504117665362, 18.49606730478969752, 1.603550922811438406 ) ) ;
#37414 = CARTESIAN_POINT ( 'NONE',  ( -1.978713825503293000, 117.0827246868714013, -0.4887249842031141656 ) ) ;
#37415 = CARTESIAN_POINT ( 'NONE',  ( 4.765286331752896842, 117.6625230355866734, -0.9424543435797743118 ) ) ;
#37416 = EDGE_CURVE ( 'NONE', #36699, #35463, #24234, .T. ) ;
#37417 = VERTEX_POINT ( 'NONE', #7918 ) ;
#37418 = CARTESIAN_POINT ( 'NONE',  ( -15.28873023128513431, 143.4753230507764670, 0.02859522846259937578 ) ) ;
#37419 = CARTESIAN_POINT ( 'NONE',  ( 6.478224611219328466, -13.79365725417489053, 0.02984861787792387686 ) ) ;
#37420 = CARTESIAN_POINT ( 'NONE',  ( -5.243373088111836999, 115.7725975576125421, -0.9931249584465892122 ) ) ;
#37421 = EDGE_LOOP ( 'NONE', ( #5260, #31371, #10895, #22601 ) ) ;
#37422 = CARTESIAN_POINT ( 'NONE',  ( 12.47579035109649936, 122.9501582372872406, 1.831147514963964884 ) ) ;
#37423 = DIRECTION ( 'NONE',  ( -4.017660918040594346E-17, 1.000000000000000000, 2.376309959284834438E-19 ) ) ;
#37424 = DIRECTION ( 'NONE',  ( -1.000000000000000000, 0.000000000000000000, 0.000000000000000000 ) ) ;
#37425 = CARTESIAN_POINT ( 'NONE',  ( -0.8718816746735710277, 108.7514562038770976, 4.146788293844217321 ) ) ;
#37426 = CARTESIAN_POINT ( 'NONE',  ( -6.647063868753328997, 9.619588520696709111, 5.217091374630535405 ) ) ;
#37427 = CARTESIAN_POINT ( 'NONE',  ( 8.365438877267163065, 122.6561726160659731, 0.7803013885889898971 ) ) ;
#37428 = LINE ( 'NONE', #5709, #28767 ) ;
#37429 = CARTESIAN_POINT ( 'NONE',  ( 13.37627446016221811, 119.7032035076741465, -0.2201875619950499907 ) ) ;
#37430 = CARTESIAN_POINT ( 'NONE',  ( 5.813441077436474202, 56.51500000000003610, -4.384678760708148992 ) ) ;
#37431 = CARTESIAN_POINT ( 'NONE',  ( -58.36702958454534951, -0.2857891562030455135, 0.06428893395075664652 ) ) ;
#37432 = CARTESIAN_POINT ( 'NONE',  ( 2.958531772299236362, 39.20946620154573736, 1.329372033065076453 ) ) ;
#37433 = CARTESIAN_POINT ( 'NONE',  ( -51.04345146481078643, 14.57989528305921745, 4.679979037057004909 ) ) ;
#37434 = DIRECTION ( 'NONE',  ( -0.9998004120163608288, 0.000000000000000000, -0.01997839162482747608 ) ) ;
#37435 = CARTESIAN_POINT ( 'NONE',  ( -4.118424193844660408, 118.2429491485453354, 0.1861966408306291454 ) ) ;
#37436 = CARTESIAN_POINT ( 'NONE',  ( 3.765733841297878470, 109.1680412998367018, -3.784223926032564744 ) ) ;
#37437 = VERTEX_POINT ( 'NONE', #37100 ) ;
#37438 = CARTESIAN_POINT ( 'NONE',  ( -53.17586183559576085, 10.67386474145934372, 4.017225210190868978 ) ) ;
#37439 = CARTESIAN_POINT ( 'NONE',  ( -8.260936656145158707, 120.1795542499276337, -1.448930651378003365 ) ) ;
#37440 = DIRECTION ( 'NONE',  ( -0.000000000000000000, -0.000000000000000000, -1.000000000000000000 ) ) ;
#37441 = CARTESIAN_POINT ( 'NONE',  ( 4.269754544072226210, 118.2136401199853850, 0.5281557113276503790 ) ) ;
#37442 = CARTESIAN_POINT ( 'NONE',  ( -4.491182069977996072, 120.9948550335633115, -0.4087774027959018563 ) ) ;
#37443 = CARTESIAN_POINT ( 'NONE',  ( -2.958531772299361595, 50.13146620154573441, -1.329372033065077119 ) ) ;
#37444 = AXIS2_PLACEMENT_3D ( 'NONE', #31063, #27867, #37672 ) ;
#37445 = DIRECTION ( 'NONE',  ( -1.000000000000000000, 1.365923996832131856E-16, 0.000000000000000000 ) ) ;
#37446 = ORIENTED_EDGE ( 'NONE', *, *, #38355, .T. ) ;
#37447 = CARTESIAN_POINT ( 'NONE',  ( 0.9564925537785137211, 29.00497265395555857, -4.523030980006896407 ) ) ;
#37448 = CARTESIAN_POINT ( 'NONE',  ( 0.006810764310280531704, 120.3493709785083183, -0.3408384964863777622 ) ) ;
#37449 = CARTESIAN_POINT ( 'NONE',  ( -5.591489108514605455, 77.73497692594764885, -1.269999999999996021 ) ) ;
#37450 = CARTESIAN_POINT ( 'NONE',  ( -43.40712238249599864, 21.47926646521387184, 2.288489392298276748 ) ) ;
#37451 = CARTESIAN_POINT ( 'NONE',  ( -41.05193670661653726, 23.09446788613699653, 1.270000000071882518 ) ) ;
#37452 = CARTESIAN_POINT ( 'NONE',  ( 7.784761315929978664, 122.6240617022501169, 0.1928303156072929958 ) ) ;
#37453 = CARTESIAN_POINT ( 'NONE',  ( 4.610398055573782905, 23.01736123548795021, -0.3254830233858732602 ) ) ;
#37454 = CARTESIAN_POINT ( 'NONE',  ( 22.22941764614895277, 150.1947564971097222, 1.617977611002929805 ) ) ;
#37455 = CARTESIAN_POINT ( 'NONE',  ( 5.664977208693820820, 65.30181249999998272, -5.033228321271210781 ) ) ;
#37457 = CARTESIAN_POINT ( 'NONE',  ( 21.08161885447492168, 149.3892802667211868, -1.460526482899864309 ) ) ;
#37456 = CARTESIAN_POINT ( 'NONE',  ( 3.046489168745748266, -14.83993489217504091, 3.784491786591300588 ) ) ;
#37458 = CARTESIAN_POINT ( 'NONE',  ( -7.897101653775167485, 156.2605297791399437, 1.696642280025655758 ) ) ;
#37459 = CARTESIAN_POINT ( 'NONE',  ( 4.518289034361447243, 23.24227448397437001, -0.9983406360900146659 ) ) ;
#37460 = CARTESIAN_POINT ( 'NONE',  ( -0.9708930699732380987, 116.8374933757159795, -0.3283832199399771001 ) ) ;
#37461 = CARTESIAN_POINT ( 'NONE',  ( 0.2555639604167124768, 10.49987491555810593, 0.9396316490698124468 ) ) ;
#37462 = B_SPLINE_CURVE_WITH_KNOTS ( 'NONE', 3,
 ( #9068, #19052, #22653, #19680, #41876, #29066 ),
 .UNSPECIFIED., .F., .F.,
 ( 4, 2, 4 ),
 ( 8.339423840660491790E-05, 0.0004508778365104737095, 0.0008183614346143424333 ),
 .UNSPECIFIED. ) ;
#37463 = ORIENTED_EDGE ( 'NONE', *, *, #23687, .T. ) ;
#37464 = CARTESIAN_POINT ( 'NONE',  ( -51.42025106686629243, 13.11195823927271320, 3.453838694686329536 ) ) ;
#37465 = CARTESIAN_POINT ( 'NONE',  ( -11.61789020275273110, 128.2970750771678752, 0.3952796010287949469 ) ) ;
#37466 = CARTESIAN_POINT ( 'NONE',  ( 5.673176617818914913, -13.06232935199844114, 2.160669506476638357 ) ) ;
#37467 = CARTESIAN_POINT ( 'NONE',  ( 5.070296302330485894, 156.2174774745075183, -1.306674740328298112 ) ) ;
#37468 = ORIENTED_EDGE ( 'NONE', *, *, #2742, .T. ) ;
#37469 = CARTESIAN_POINT ( 'NONE',  ( 2.906445675538798845, 115.7029491485453434, 1.674890049949036896 ) ) ;
#37470 = CARTESIAN_POINT ( 'NONE',  ( 1.985452195540454934, -15.12483337350742296, 5.348831821476924375 ) ) ;
#37471 = CARTESIAN_POINT ( 'NONE',  ( -4.796665243919449928, 117.7368776771948831, -1.049558999684713667 ) ) ;
#37472 = CARTESIAN_POINT ( 'NONE',  ( 0.001367086239692558765, 156.3041635968983485, -0.06841458569046209026 ) ) ;
#37473 = VERTEX_POINT ( 'NONE', #16645 ) ;
#37474 = CARTESIAN_POINT ( 'NONE',  ( 2.242647228084396982, 118.4336326928681729, 0.7879290844312368813 ) ) ;
#37475 = FACE_OUTER_BOUND ( 'NONE', #7213, .T. ) ;
#37476 = FACE_OUTER_BOUND ( 'NONE', #32635, .T. ) ;
#37477 = CIRCLE ( 'NONE', #7539, 5.080000000000006288 ) ;
#37478 = CARTESIAN_POINT ( 'NONE',  ( -28.09515292912719175, 77.51021392068167870, 1.523999999999992028 ) ) ;
#37479 = CARTESIAN_POINT ( 'NONE',  ( 1.415223785869755613, 159.6020224343070026, -0.1017758242917465722 ) ) ;
#37480 = DIRECTION ( 'NONE',  ( -0.4849315768086481238, -0.8745520943968281280, 8.647447314816545091E-15 ) ) ;
#37481 = TOROIDAL_SURFACE ( 'NONE', #18402, 5.080000000000005400, 0.5080000000000000071 ) ;
#37482 = CARTESIAN_POINT ( 'NONE',  ( 1.693218665641037735, -15.38421670575504407, 5.480670678043046529 ) ) ;
#37483 = CARTESIAN_POINT ( 'NONE',  ( 11.25890006629630591, 56.90956307411710924, 5.016499999999999737 ) ) ;
#37484 = DIRECTION ( 'NONE',  ( 0.6294287539884059202, 0.7770581983690814099, 1.945484789722797322E-16 ) ) ;
#37485 = CARTESIAN_POINT ( 'NONE',  ( -4.743057898818983986, 117.8454596101170750, 0.8300490160943797546 ) ) ;
#37486 = ORIENTED_EDGE ( 'NONE', *, *, #1206, .F. ) ;
#37487 = ORIENTED_EDGE ( 'NONE', *, *, #18338, .F. ) ;
#37488 = CARTESIAN_POINT ( 'NONE',  ( -1.008980461684340080, 118.7629491485454025, 1.225333421752663021 ) ) ;
#37489 = EDGE_CURVE ( 'NONE', #24814, #30281, #3873, .T. ) ;
#37490 = CARTESIAN_POINT ( 'NONE',  ( 2.640464088051889480, 117.6788351930554199, -0.6858096912303740522 ) ) ;
#37491 = CARTESIAN_POINT ( 'NONE',  ( -1.881281939329409125, 113.2583846565721757, -2.513576850050686318 ) ) ;
#37492 = CARTESIAN_POINT ( 'NONE',  ( 4.873962307784054815, 117.4785107143119092, 1.135666542019568404 ) ) ;
#37493 = CARTESIAN_POINT ( 'NONE',  ( -4.611806494114576438, 117.9324678712513759, -0.9633187536371230486 ) ) ;
#37494 = CARTESIAN_POINT ( 'NONE',  ( -0.1289837059588684054, 106.1822392402443143, 5.211597877332949658 ) ) ;
#37495 =( LENGTH_UNIT ( ) NAMED_UNIT ( * ) SI_UNIT ( .MILLI., .METRE. ) );
#37496 = CARTESIAN_POINT ( 'NONE',  ( -57.43227285409300009, 3.226759729073131133, 2.064049688025078488 ) ) ;
#37497 = CARTESIAN_POINT ( 'NONE',  ( -17.14500000000000313, 71.11999999999999034, -5.080000000000000959 ) ) ;
#37498 = CARTESIAN_POINT ( 'NONE',  ( 2.953219771904812774, -14.51063682438745417, 4.500484459945554683 ) ) ;
#37499 = CARTESIAN_POINT ( 'NONE',  ( 6.983605877934210504, 124.9344662015457175, 0.1395490654994204494 ) ) ;
#37500 = CARTESIAN_POINT ( 'NONE',  ( -2.127773614577548766, 31.68089970468614069, 4.228698531287117035 ) ) ;
#37501 = CARTESIAN_POINT ( 'NONE',  ( -0.1384325697538203448, 115.7030669245054497, 1.759162187147021550 ) ) ;
#37502 = CARTESIAN_POINT ( 'NONE',  ( 0.6590154617207463206, 19.50938314818779062, -4.574821423538240950 ) ) ;
#37503 = EDGE_LOOP ( 'NONE', ( #22307, #23162, #29506, #347, #1471, #23186 ) ) ;
#37504 = DIRECTION ( 'NONE',  ( -0.7308269722843343530, 0.6825627711659295604, -8.537024980200805055E-16 ) ) ;
#37505 = CARTESIAN_POINT ( 'NONE',  ( 2.770358398913809861, -15.65020961539316602, 4.804192819214700982 ) ) ;
#37506 = CARTESIAN_POINT ( 'NONE',  ( -5.031139012175450453, 119.0545008048120366, 0.9043826811606223703 ) ) ;
#37507 = CARTESIAN_POINT ( 'NONE',  ( -0.7929698604315037480, -4.880942799695234591, 0.5714185140920283734 ) ) ;
#37508 = AXIS2_PLACEMENT_3D ( 'NONE', #7930, #34752, #8769 ) ;
#37509 = CARTESIAN_POINT ( 'NONE',  ( 0.9036657058557058253, 17.56215383894848614, 0.3677562154327245758 ) ) ;
#37510 = EDGE_CURVE ( 'NONE', #36953, #29654, #38543, .T. ) ;
#37511 = VERTEX_POINT ( 'NONE', #31317 ) ;
#37512 = ORIENTED_EDGE ( 'NONE', *, *, #25820, .T. ) ;
#37513 = FACE_OUTER_BOUND ( 'NONE', #34187, .T. ) ;
#37514 = CARTESIAN_POINT ( 'NONE',  ( 0.1346051971225362132, 106.5118632461160217, 5.080372420286161095 ) ) ;
#37515 = CARTESIAN_POINT ( 'NONE',  ( -1.846154440359773385, 156.5029897098349636, 0.9826124536999809589 ) ) ;
#37516 = DIRECTION ( 'NONE',  ( 0.000000000000000000, -0.000000000000000000, -1.000000000000000000 ) ) ;
#37517 = CARTESIAN_POINT ( 'NONE',  ( 4.515008956836783049, 118.0822181440858287, -0.6204359177205427400 ) ) ;
#37518 = CARTESIAN_POINT ( 'NONE',  ( 10.90225753734626757, 122.6724665872831679, -1.173089625842028472 ) ) ;
#37519 = VECTOR ( 'NONE', #2719, 1000.000000000000000 ) ;
#37520 = CARTESIAN_POINT ( 'NONE',  ( -15.05911097818686883, 125.5446871707752763, -2.024973821723874856 ) ) ;
#37521 = DIRECTION ( 'NONE',  ( 5.188838149069472160E-16, -1.699382548006136559E-16, -1.000000000000000000 ) ) ;
#37522 = CARTESIAN_POINT ( 'NONE',  ( 4.123312261480172047, 118.2429491485453354, -0.1806149775832581461 ) ) ;
#37523 = CARTESIAN_POINT ( 'NONE',  ( 13.24427968334902062, 134.0707761029912035, -0.3110103029741251857 ) ) ;
#37524 = EDGE_LOOP ( 'NONE', ( #36854, #8329, #28858, #27790 ) ) ;
#37525 = CARTESIAN_POINT ( 'NONE',  ( 2.101618670382315646, -15.21789252882688182, 5.187277112784037136 ) ) ;
#37526 = AXIS2_PLACEMENT_3D ( 'NONE', #35625, #32844, #12615 ) ;
#37527 = CARTESIAN_POINT ( 'NONE',  ( 11.25890006629607143, 56.90956307411702397, -5.016500000000000625 ) ) ;
#37528 = CARTESIAN_POINT ( 'NONE',  ( -57.70126415073575998, 1.705439686548140710, 1.647193596431507645 ) ) ;
#37529 = CARTESIAN_POINT ( 'NONE',  ( 4.168288449772385995, -6.568960759998498489, 2.029292378399509378 ) ) ;
#37530 = CARTESIAN_POINT ( 'NONE',  ( 16.52407570443671148, 148.2569838091642964, 1.909119861936069640 ) ) ;
#37531 = CARTESIAN_POINT ( 'NONE',  ( 0.03201377673046579275, 33.52827609515317420, 3.383309648808628278 ) ) ;
#37532 = CARTESIAN_POINT ( 'NONE',  ( -4.210090452738601385, 118.4033805524614849, 0.5735154781215828779 ) ) ;
#37533 = AXIS2_PLACEMENT_3D ( 'NONE', #15102, #28534, #11493 ) ;
#37534 = AXIS2_PLACEMENT_3D ( 'NONE', #27635, #2305, #16050 ) ;
#37535 = CARTESIAN_POINT ( 'NONE',  ( -0.5842699607273857954, -4.454521554441356557, 4.585487691134133570 ) ) ;
#37536 = CARTESIAN_POINT ( 'NONE',  ( 13.59447973938432241, 150.2262467139961473, 0.3969463805754211427 ) ) ;
#37537 = B_SPLINE_CURVE_WITH_KNOTS ( 'NONE', 3,
 ( #37285, #24484, #5142, #18096, #29591, #6177 ),
 .UNSPECIFIED., .F., .F.,
 ( 4, 2, 4 ),
 ( 0.000000000000000000, 0.5000000000000000000, 1.000000000000000000 ),
 .UNSPECIFIED. ) ;
#37538 = EDGE_CURVE ( 'NONE', #27974, #1598, #7013, .T. ) ;
#37539 = CARTESIAN_POINT ( 'NONE',  ( 4.614102091175348086, 5.327238342305563812, -7.074968232746598140 ) ) ;
#37540 = CARTESIAN_POINT ( 'NONE',  ( -57.28860081656939229, 2.041040056096066202, -1.590330371070468152 ) ) ;
#37541 = CARTESIAN_POINT ( 'NONE',  ( -5.507236293901328850, 116.9742688490489684, -0.6495416791669329504 ) ) ;
#37542 = DIRECTION ( 'NONE',  ( -0.01997839162482737546, -1.040247600000940825E-18, 0.9998004120163610509 ) ) ;
#37543 = CARTESIAN_POINT ( 'NONE',  ( -8.313969523394650452, 67.96940778435646280, -1.269999999999995577 ) ) ;
#37544 = DIRECTION ( 'NONE',  ( 0.2883665106726583938, 0.9575201071113210727, 0.000000000000000000 ) ) ;
#37545 = LINE ( 'NONE', #40551, #18154 ) ;
#37546 = CARTESIAN_POINT ( 'NONE',  ( -4.785772612713214080, 1.365856510964248649, -6.940074030798050408 ) ) ;
#37547 = CARTESIAN_POINT ( 'NONE',  ( 0.6939153454146552713, 117.9394491594808159, 1.403384569749132282 ) ) ;
#37548 = DIRECTION ( 'NONE',  ( 9.627370216492862708E-17, 1.000000000000000000, -0.000000000000000000 ) ) ;
#37549 = CARTESIAN_POINT ( 'NONE',  ( 2.568134854143032442, -15.02010252187911554, 4.714990346623905815 ) ) ;
#37550 = CARTESIAN_POINT ( 'NONE',  ( 0.5256976547265018729, 110.0486234891351245, -3.677594289785357518 ) ) ;
#37551 = CARTESIAN_POINT ( 'NONE',  ( -15.13173320725188553, 120.7387302883610118, 0.2100629019518970853 ) ) ;
#37552 = VERTEX_POINT ( 'NONE', #6395 ) ;
#37553 = CARTESIAN_POINT ( 'NONE',  ( -58.66661043166477896, 0.3408866871785626307, -0.5032371457779314383 ) ) ;
#37554 = ORIENTED_EDGE ( 'NONE', *, *, #23278, .F. ) ;
#37555 = CYLINDRICAL_SURFACE ( 'NONE', #40330, 0.2539999999999996150 ) ;
#37556 = CARTESIAN_POINT ( 'NONE',  ( -2.846496745999657740, 121.0294354067666802, -0.02263809173328865804 ) ) ;
#37557 = CARTESIAN_POINT ( 'NONE',  ( 5.316001070410483642, -15.20466279102368468, 3.045604417706107458 ) ) ;
#37558 = CARTESIAN_POINT ( 'NONE',  ( -13.28772774122556122, 155.5383117973235585, 1.582857276444406658 ) ) ;
#37559 = CARTESIAN_POINT ( 'NONE',  ( 22.37379725164909416, 146.3189071340513294, -1.009121573351525303 ) ) ;
#37560 = CARTESIAN_POINT ( 'NONE',  ( 1.893578447776079754, 19.08455809737888487, -4.224370802633358402 ) ) ;
#37561 = CARTESIAN_POINT ( 'NONE',  ( -14.67516008282149897, 120.3119357913517291, -0.6057029122735547721 ) ) ;
#37562 = CARTESIAN_POINT ( 'NONE',  ( -52.44660108373793150, 12.13357835523497563, -4.279154699026443964 ) ) ;
#37563 = ORIENTED_EDGE ( 'NONE', *, *, #26671, .T. ) ;
#37564 = CARTESIAN_POINT ( 'NONE',  ( 2.183095549435995597, 116.1905277699444952, 0.05681614786306111303 ) ) ;
#37565 = DIRECTION ( 'NONE',  ( -0.9998004120163609398, 0.000000000000000000, -0.01997839162482749689 ) ) ;
#37566 = CARTESIAN_POINT ( 'NONE',  ( -2.082154424533116721, 156.9412006218898057, 1.407003841209468753 ) ) ;
#37567 = CARTESIAN_POINT ( 'NONE',  ( -19.97113776634630256, 79.44829951959813741, -1.270000000000003570 ) ) ;
#37568 = CARTESIAN_POINT ( 'NONE',  ( 6.702632528927829902, 119.6463993818898359, -1.017002412926887311 ) ) ;
#37569 = CARTESIAN_POINT ( 'NONE',  ( -21.00644369030287351, 149.3892802667211868, -2.301546136566545275 ) ) ;
#37570 = CARTESIAN_POINT ( 'NONE',  ( -54.39768377094780760, 8.094885465611476150, -3.421923752996840928 ) ) ;
#37571 = AXIS2_PLACEMENT_3D ( 'NONE', #36044, #29647, #58 ) ;
#37572 = EDGE_CURVE ( 'NONE', #4432, #31634, #31900, .T. ) ;
#37573 = CARTESIAN_POINT ( 'NONE',  ( 4.574562528865535604, 155.9125706774115940, -0.7527123864290742317 ) ) ;
#37574 = ORIENTED_EDGE ( 'NONE', *, *, #34966, .T. ) ;
#37575 = CARTESIAN_POINT ( 'NONE',  ( -18.30884121703848066, 147.6341482083243761, -2.394331140672893099 ) ) ;
#37576 = CARTESIAN_POINT ( 'NONE',  ( 3.404406166340397277, -15.64019586361782643, 4.053891870528842922 ) ) ;
#37577 = CARTESIAN_POINT ( 'NONE',  ( -4.381873770367138654, 118.1622909913610187, -0.6666483627925274824 ) ) ;
#37578 = CARTESIAN_POINT ( 'NONE',  ( -58.09657527255103560, 0.9821181129459344294, -1.359330230256445393 ) ) ;
#37579 = CIRCLE ( 'NONE', #18537, 3.111499999999999932 ) ;
#37580 = CARTESIAN_POINT ( 'NONE',  ( -4.998096739426165946, 117.4661840451863100, 0.7739782158464477702 ) ) ;
#37581 = CARTESIAN_POINT ( 'NONE',  ( 12.00230265366658600, 124.3217332413628640, 1.707838685025481418 ) ) ;
#37582 = ADVANCED_FACE ( 'NONE', ( #15548 ), #12366, .T. ) ;
#37583 = DIRECTION ( 'NONE',  ( -5.188838149069472160E-16, 1.699382548006136559E-16, 1.000000000000000000 ) ) ;
#37584 = CARTESIAN_POINT ( 'NONE',  ( 6.515560366292186600, -0.8950661730705262720, -5.416678580889517924 ) ) ;
#37585 = CARTESIAN_POINT ( 'NONE',  ( 9.426771831325547524, 124.2753396726362780, 0.5138045435804897698 ) ) ;
#37586 = CARTESIAN_POINT ( 'NONE',  ( -54.34142964503966056, 9.837102586603037935, -3.694930414371515148 ) ) ;
#37587 = EDGE_CURVE ( 'NONE', #16646, #6407, #28957, .T. ) ;
#37589 = ORIENTED_EDGE ( 'NONE', *, *, #11735, .T. ) ;
#37588 = CARTESIAN_POINT ( 'NONE',  ( -44.16391282238571847, 20.57229585060895616, -1.749602973179261944 ) ) ;
#37590 = CARTESIAN_POINT ( 'NONE',  ( -2.609053440593664508, 117.3993834727424286, 1.321828139561898041 ) ) ;
#37591 = CARTESIAN_POINT ( 'NONE',  ( -7.869668022420311715, 122.1460381220860540, -0.8492931709348270353 ) ) ;
#37592 = AXIS2_PLACEMENT_3D ( 'NONE', #36571, #3406, #7597 ) ;
#37593 = EDGE_CURVE ( 'NONE', #5725, #22720, #32399, .T. ) ;
#37594 = CARTESIAN_POINT ( 'NONE',  ( -57.63883995378735392, 1.113466886629776997, 0.4249547484444501921 ) ) ;
#37595 = CARTESIAN_POINT ( 'NONE',  ( -51.38196307734524737, 20.99359796827592817, 0.3730309213897141096 ) ) ;
#37596 = CARTESIAN_POINT ( 'NONE',  ( -22.65693159617103802, 137.2763855621842026, -0.2353725067100884694 ) ) ;
#37597 = ORIENTED_EDGE ( 'NONE', *, *, #2971, .F. ) ;
#37598 = CARTESIAN_POINT ( 'NONE',  ( -48.33886291794431145, 23.55519408767752054, -1.110521498696447118 ) ) ;
#37599 = CARTESIAN_POINT ( 'NONE',  ( -5.844832110966546423, 121.2807673435547571, -0.4307865532411910281 ) ) ;
#37600 = CARTESIAN_POINT ( 'NONE',  ( -7.895606690698891761, 122.1535174891447468, 0.5249436039529434828 ) ) ;
#37601 = EDGE_LOOP ( 'NONE', ( #38772, #10356, #18787, #23023 ) ) ;
#37602 = CARTESIAN_POINT ( 'NONE',  ( -4.757281688282281706, 117.4019771528195690, -1.206666768175857385 ) ) ;
#37603 = CARTESIAN_POINT ( 'NONE',  ( -3.721623402434381056, 121.0563512343167645, -0.1807651092205456167 ) ) ;
#37604 = CARTESIAN_POINT ( 'NONE',  ( 3.016199308703121140, -15.16462411293013979, 5.702656747445028707 ) ) ;
#37605 = CARTESIAN_POINT ( 'NONE',  ( -5.259787267153689605, 158.8115599018184412, 1.116423854902496071 ) ) ;
#37606 = LINE ( 'NONE', #41236, #25440 ) ;
#37607 = CIRCLE ( 'NONE', #24004, 0.3810000000000030584 ) ;
#37608 = CARTESIAN_POINT ( 'NONE',  ( 20.36427691206291257, 129.0035756037533758, 0.5974333909176805513 ) ) ;
#37609 = CARTESIAN_POINT ( 'NONE',  ( 7.783246152616065672, 154.6561476914895081, 0.1555277812256516956 ) ) ;
#37610 = CARTESIAN_POINT ( 'NONE',  ( -4.876368518028720622, 117.7626870461374580, 0.7578736298905299762 ) ) ;
#37611 = CARTESIAN_POINT ( 'NONE',  ( -0.9636992805836054332, 23.18535052081312386, 0.1494942155713751553 ) ) ;
#37612 = CARTESIAN_POINT ( 'NONE',  ( -15.48069746188187956, 120.7065362441885981, -0.4134764081404141978 ) ) ;
#37613 = CARTESIAN_POINT ( 'NONE',  ( -46.85406971281315691, 20.44882436048083818, -5.016006885995599518 ) ) ;
#37614 = CIRCLE ( 'NONE', #41699, 0.5079999999999997851 ) ;
#37615 = CARTESIAN_POINT ( 'NONE',  ( -38.65395868481546415, 29.38327706004843876, 1.523999999999994470 ) ) ;
#37616 = ADVANCED_FACE ( 'NONE', ( #32371 ), #33111, .T. ) ;
#37617 = VERTEX_POINT ( 'NONE', #2794 ) ;
#37618 = CARTESIAN_POINT ( 'NONE',  ( 6.232159320193214391, 119.2349664191863070, 1.255280209171262040 ) ) ;
#37619 =( BOUNDED_SURFACE ( )  B_SPLINE_SURFACE ( 3, 2, ( 
 ( #26441, #29643, #10248 ),
 ( #36462, #26865, #20243 ),
 ( #39873, #36252, #4098 ),
 ( #7074, #20037, #8317 ),
 ( #14485, #11300, #40706 ),
 ( #5350, #1529, #40299 ),
 ( #18514, #31306, #18100 ),
 ( #31103, #18304, #34107 ),
 ( #8532, #34524, #31520 ),
 ( #27904, #1942, #14693 ) ),
 .UNSPECIFIED., .F., .F., .F. ) 
 B_SPLINE_SURFACE_WITH_KNOTS ( ( 4, 2, 2, 2, 4 ),
 ( 3, 3 ),
 ( 4.712388980384689674, 5.105088062083413369, 5.497787143782137065, 5.890486225480861648, 6.283185307179585344 ),
 ( 0.000000000000000000, 1.000000000000000000 ),
 .UNSPECIFIED. ) 
 GEOMETRIC_REPRESENTATION_ITEM ( )  RATIONAL_B_SPLINE_SURFACE ( (
 ( 1.000000000000000000, 0.7071067811865475727, 1.000000000000000000),
 ( 1.000000000000000000, 0.7139102541738931995, 1.000000000000000000),
 ( 1.000000000000000000, 0.7206031636702244780, 1.000000000000000000),
 ( 1.000000000000000000, 0.7328301610703541469, 1.000000000000000000),
 ( 1.000000000000000000, 0.7383589052088842530, 1.000000000000000000),
 ( 1.000000000000000000, 0.7475127447244133139, 1.000000000000000000),
 ( 1.000000000000000000, 0.7511365686958336729, 1.000000000000000000),
 ( 1.000000000000000000, 0.7560206254138944759, 1.000000000000000000),
 ( 1.000000000000000000, 0.7572851909593535380, 1.000000000000000000),
 ( 1.000000000000000000, 0.7572803591334833495, 1.000000000000000000) ) ) 
 REPRESENTATION_ITEM ( '' )  SURFACE ( )  );
#37620 = CARTESIAN_POINT ( 'NONE',  ( -5.334819979684278124, 105.1224662015457199, -0.01225255181739587709 ) ) ;
#37621 = CARTESIAN_POINT ( 'NONE',  ( -0.02156508032628448243, 159.2730288250082538, 1.079204802879467850 ) ) ;
#37622 = CARTESIAN_POINT ( 'NONE',  ( -58.49146960918327665, -0.5079027975582817156, -0.2843517202595862714 ) ) ;
#37623 = CARTESIAN_POINT ( 'NONE',  ( 10.28923284337270871, 120.3038588096988803, -1.141564125291498089 ) ) ;
#37624 = CARTESIAN_POINT ( 'NONE',  ( 4.543739712435177047, -15.19060223592207137, -0.8445694877862246486 ) ) ;
#37625 = CARTESIAN_POINT ( 'NONE',  ( 0.007599820978684407140, 117.2191897141855179, -0.3803261187632671625 ) ) ;
#37626 = CARTESIAN_POINT ( 'NONE',  ( 4.832896482213426381, 117.6748455158117395, -0.9055039834170672819 ) ) ;
#37627 = CARTESIAN_POINT ( 'NONE',  ( 0.6661646497576521053, 105.9485402691003060, 5.310688274649121077 ) ) ;
#37628 = ORIENTED_EDGE ( 'NONE', *, *, #2742, .F. ) ;
#37629 = CARTESIAN_POINT ( 'NONE',  ( -15.73538347863352804, 145.6958675726371553, -0.1858358763210236630 ) ) ;
#37630 = CARTESIAN_POINT ( 'NONE',  ( -12.47579035109662726, 122.9501582372872406, -1.831147514963964662 ) ) ;
#37631 = CARTESIAN_POINT ( 'NONE',  ( 5.947420766284201576, -14.61438673846185488, 1.993024607196187459 ) ) ;
#37632 = AXIS2_PLACEMENT_3D ( 'NONE', #26822, #14025, #10624 ) ;
#37633 = DIRECTION ( 'NONE',  ( 0.1565721916418034432, 0.9876665170007953298, -8.659954811667511346E-17 ) ) ;
#37634 = CIRCLE ( 'NONE', #11082, 6.349999999999999645 ) ;
#37635 = EDGE_CURVE ( 'NONE', #41779, #11064, #29384, .T. ) ;
#37636 = CARTESIAN_POINT ( 'NONE',  ( -0.7954092736443492129, 117.3993835805549537, -1.485886877084427571 ) ) ;
#37637 = ORIENTED_EDGE ( 'NONE', *, *, #20329, .F. ) ;
#37638 = CARTESIAN_POINT ( 'NONE',  ( 7.518309192797149265, 120.1328256275108828, 1.363123692563724454 ) ) ;
#37639 = CARTESIAN_POINT ( 'NONE',  ( -28.60507221318228943, 76.72702915747851193, -1.270000000000007567 ) ) ;
#37640 = CARTESIAN_POINT ( 'NONE',  ( 3.682264917456193665, 69.94346620154573202, 0.07358041635423968885 ) ) ;
#37641 = AXIS2_PLACEMENT_3D ( 'NONE', #819, #27209, #16980 ) ;
#37642 = CARTESIAN_POINT ( 'NONE',  ( -0.6471768874971802754, 112.6282971158091470, 2.732684515117584034 ) ) ;
#37643 = CARTESIAN_POINT ( 'NONE',  ( 0.3193725800214416988, -13.04287899337829515, -8.422265478599168631 ) ) ;
#37644 = CARTESIAN_POINT ( 'NONE',  ( 9.846098633339698480, 123.9483309312939099, 0.9889573185143103462 ) ) ;
#37645 = CARTESIAN_POINT ( 'NONE',  ( 10.92199999999999704, 12.96416000000000146, 0.000000000000000000 ) ) ;
#37646 = B_SPLINE_CURVE_WITH_KNOTS ( 'NONE', 3,
 ( #38948, #19749, #35548, #19334, #10176, #31928 ),
 .UNSPECIFIED., .F., .F.,
 ( 4, 2, 4 ),
 ( 0.07978617534938510503, 0.5398930876746925733, 1.000000000000000000 ),
 .UNSPECIFIED. ) ;
#37647 = CARTESIAN_POINT ( 'NONE',  ( 20.34281169216118101, 152.5255278361454145, -0.5339126128458229203 ) ) ;
#37648 = FACE_OUTER_BOUND ( 'NONE', #11709, .T. ) ;
#37649 = CARTESIAN_POINT ( 'NONE',  ( -58.18051401232126807, 0.1137601867684435997, 0.5894366672358869463 ) ) ;
#37650 = CARTESIAN_POINT ( 'NONE',  ( 5.177913976931208140, 64.41499993257285439, 5.372100000000000541 ) ) ;
#37651 = ADVANCED_FACE ( 'NONE', ( #29165 ), #13199, .T. ) ;
#37652 = CARTESIAN_POINT ( 'NONE',  ( -6.517733866319332394E-14, 78.32546620154573702, 2.848871684924056535E-29 ) ) ;
#37653 = CARTESIAN_POINT ( 'NONE',  ( -4.248938432191276426, 118.2248689806160797, 0.3116314407555961230 ) ) ;
#37654 = CARTESIAN_POINT ( 'NONE',  ( 5.113597892238037623, 113.8200073110514836, -1.623610037850725218 ) ) ;
#37655 = VERTEX_POINT ( 'NONE', #17016 ) ;
#37656 = CARTESIAN_POINT ( 'NONE',  ( -48.82738941085167284, 18.57305038084609095, 5.399437279161905856 ) ) ;
#37657 = CARTESIAN_POINT ( 'NONE',  ( 4.133480150819543120, 119.2345050349130702, -0.7621166359342830265 ) ) ;
#37658 = CARTESIAN_POINT ( 'NONE',  ( -2.934015389105513183, 107.8085536575111689, -4.480064466837520243 ) ) ;
#37659 = CARTESIAN_POINT ( 'NONE',  ( 4.378792325076509506, 118.1614122340369875, 0.6691606409793376953 ) ) ;
#37660 = CARTESIAN_POINT ( 'NONE',  ( -6.199776539618502724, 155.3658059236344684, -0.8002054381730364652 ) ) ;
#37661 = CARTESIAN_POINT ( 'NONE',  ( -23.14542444889682216, 82.37908244650444090, -1.270000000000005791 ) ) ;
#37662 = PLANE ( 'NONE',  #23219 ) ;
#37663 = ORIENTED_EDGE ( 'NONE', *, *, #3477, .T. ) ;
#37664 = CARTESIAN_POINT ( 'NONE',  ( 2.488009491785908800, 18.85968022696138391, -3.895047602898422223 ) ) ;
#37665 = CARTESIAN_POINT ( 'NONE',  ( -30.03238267980982457, 57.98137616137810824, 1.524000000000849564 ) ) ;
#37666 = DIRECTION ( 'NONE',  ( 4.017660918040594346E-17, -1.000000000000000000, -2.376309959284834438E-19 ) ) ;
#37667 = CARTESIAN_POINT ( 'NONE',  ( 3.174366308151880922, 104.6144662015457243, 0.06343139340882769650 ) ) ;
#37668 = DIRECTION ( 'NONE',  ( -0.7770581983690836303, 0.6294287539884032556, -5.101669463485833779E-16 ) ) ;
#37669 = CARTESIAN_POINT ( 'NONE',  ( -6.062815761959031491, 121.4378744781062096, -0.02555828286107298536 ) ) ;
#37670 = CARTESIAN_POINT ( 'NONE',  ( -4.628372119175923949, 18.04465247731148381, -0.2036312542868722320 ) ) ;
#37671 = CARTESIAN_POINT ( 'NONE',  ( 14.85510260296663176, 121.0052616771249347, 1.128405194827190705 ) ) ;
#37672 = DIRECTION ( 'NONE',  ( -0.8745520943968243532, 0.4849315768086547296, -5.361993529360573944E-16 ) ) ;
#37674 = CARTESIAN_POINT ( 'NONE',  ( 13.76672422736534607, 155.7522398296385404, -1.402631553274309217 ) ) ;
#37673 = CARTESIAN_POINT ( 'NONE',  ( 3.205116352530840373, -14.62692654125133451, 3.000134484400556190 ) ) ;
#37675 = CARTESIAN_POINT ( 'NONE',  ( -9.425666535144351599, 121.4347015428822374, 1.122958709584368053 ) ) ;
#37676 = CARTESIAN_POINT ( 'NONE',  ( 4.103230867730633058, 22.16771668783608007, 2.168033597859526651 ) ) ;
#37677 = CARTESIAN_POINT ( 'NONE',  ( -1.374325311230039093, 159.5643428290674990, -0.4556871491110245365 ) ) ;
#37678 = AXIS2_PLACEMENT_3D ( 'NONE', #17879, #14681, #11490 ) ;
#37679 = CARTESIAN_POINT ( 'NONE',  ( 0.05984739657028866761, 19.78266025878678391, 0.9748693421377304658 ) ) ;
#37680 = ORIENTED_EDGE ( 'NONE', *, *, #13898, .F. ) ;
#37681 = CARTESIAN_POINT ( 'NONE',  ( -56.36488200494262202, 4.056002992322685685, 2.423683632884268579 ) ) ;
#37682 = CARTESIAN_POINT ( 'NONE',  ( -13.89276580153831020, 150.2454140652271803, 0.5485491450630710641 ) ) ;
#37683 = CARTESIAN_POINT ( 'NONE',  ( 4.441035242322985965, -14.03446645907663282, 4.353459135924754086 ) ) ;
#37684 = CARTESIAN_POINT ( 'NONE',  ( 11.42483690514958461, 124.5424752485109963, -1.054873134768183895 ) ) ;
#37685 = VERTEX_POINT ( 'NONE', #39616 ) ;
#37686 = CARTESIAN_POINT ( 'NONE',  ( 0.7772691865734456806, 115.7028435863886386, 1.754949168150819583 ) ) ;
#37687 = ORIENTED_EDGE ( 'NONE', *, *, #18824, .T. ) ;
#37688 = CARTESIAN_POINT ( 'NONE',  ( 3.240066224740343781, -14.18897675264189928, 3.749338592554243288 ) ) ;
#37689 = CARTESIAN_POINT ( 'NONE',  ( -4.710974563145049032, 117.8981397293982667, -0.9559088427545711086 ) ) ;
#37690 = CARTESIAN_POINT ( 'NONE',  ( 9.118838228053421702, 124.0847320388339625, 0.09724818526966655385 ) ) ;
#37691 = VERTEX_POINT ( 'NONE', #10837 ) ;
#37692 = CARTESIAN_POINT ( 'NONE',  ( 19.76635024033924992, 141.2215177107240436, 2.477633452034131434 ) ) ;
#37693 = CARTESIAN_POINT ( 'NONE',  ( 13.59117098936144075, 150.2425924485622772, 0.2715839415567424808 ) ) ;
#37694 = VECTOR ( 'NONE', #34520, 1000.000000000000000 ) ;
#37695 = LINE ( 'NONE', #31290, #34766 ) ;
#37696 = CARTESIAN_POINT ( 'NONE',  ( 0.001640166039734963777, 159.6041700698465036, -0.08208061555506483697 ) ) ;
#37697 = CARTESIAN_POINT ( 'NONE',  ( 21.87358050093867945, 151.4416708234707301, 0.1116233529550400561 ) ) ;
#37698 = CARTESIAN_POINT ( 'NONE',  ( -5.256666790930538014, 56.51500000000019952, -5.296388420399792629 ) ) ;
#37699 = CARTESIAN_POINT ( 'NONE',  ( 1.865576733372334761, -15.48222874659857595, 5.392302077751139677 ) ) ;
#37700 = CARTESIAN_POINT ( 'NONE',  ( 11.08653569745430190, 56.26057688450594441, 4.438844214435382796 ) ) ;
#37701 = CARTESIAN_POINT ( 'NONE',  ( -36.79765817521327165, 27.64956762128695900, 1.269999999999994689 ) ) ;
#37702 = CARTESIAN_POINT ( 'NONE',  ( -4.740160372624219853, 117.9514375547949925, 0.6504355775612526980 ) ) ;
#37703 = ORIENTED_EDGE ( 'NONE', *, *, #15180, .T. ) ;
#37704 = EDGE_LOOP ( 'NONE', ( #9384, #40632, #23735, #23199, #8754, #34051, #31327, #3733 ) ) ;
#37705 = CARTESIAN_POINT ( 'NONE',  ( 5.266140447862612817, 115.7029491485453150, -0.8695525029155279917 ) ) ;
#37706 = CARTESIAN_POINT ( 'NONE',  ( -8.413693646442473195, 119.4405076545267548, -1.388540977510597685 ) ) ;
#37707 = CARTESIAN_POINT ( 'NONE',  ( -5.744069310734515987, 120.3160329940760818, -0.4351690567359401407 ) ) ;
#37708 = CARTESIAN_POINT ( 'NONE',  ( 4.871458131390602020, 117.6697264362294533, 1.013602582129945473 ) ) ;
#37709 = CARTESIAN_POINT ( 'NONE',  ( -17.14499999999999957, 71.11999999999999034, 1.904999999999989146 ) ) ;
#37710 = CARTESIAN_POINT ( 'NONE',  ( -0.8647483397479580614, 121.9014879524050343, 0.2897378433829553290 ) ) ;
#37711 = CARTESIAN_POINT ( 'NONE',  ( -0.5842699607273857954, -4.454521554441356557, 4.585487691134133570 ) ) ;
#37712 = CARTESIAN_POINT ( 'NONE',  ( -58.33777482027512207, 1.113448835244237767, 1.208045587469420701 ) ) ;
#37713 = FACE_OUTER_BOUND ( 'NONE', #10230, .T. ) ;
#37714 = CARTESIAN_POINT ( 'NONE',  ( 2.454477138217164178, -14.79624793513299785, 5.258896552041426808 ) ) ;
#37715 = CARTESIAN_POINT ( 'NONE',  ( 7.256067632580297300, 123.0461458356614628, 0.07605313119184042847 ) ) ;
#37716 = CARTESIAN_POINT ( 'NONE',  ( -24.46582648842863961, 82.15028593570633575, -1.270000000000006679 ) ) ;
#37717 = CARTESIAN_POINT ( 'NONE',  ( -14.73199999999999932, 12.96416000000000146, 0.000000000000000000 ) ) ;
#37718 = DIRECTION ( 'NONE',  ( -0.9998004120163609398, 0.000000000000000000, -0.01997839162482749689 ) ) ;
#37719 = CARTESIAN_POINT ( 'NONE',  ( 3.935102970030662117, 16.48578375386999539, 2.424025302511324309 ) ) ;
#37721 = VERTEX_POINT ( 'NONE', #7031 ) ;
#37720 = CARTESIAN_POINT ( 'NONE',  ( 15.83212890848021281, 121.4040080620525117, 0.8411940925737090291 ) ) ;
#37722 = CARTESIAN_POINT ( 'NONE',  ( 3.864505497398623923, 104.6144662015456959, -2.895664945016856784 ) ) ;
#37723 = CARTESIAN_POINT ( 'NONE',  ( 4.238804029399687145, -15.60588767656335918, 2.735912002563000822 ) ) ;
#37724 = CARTESIAN_POINT ( 'NONE',  ( -4.562247774926802002, 157.9011380394538833, 1.652341844578318453 ) ) ;
#37725 = CARTESIAN_POINT ( 'NONE',  ( 0.2465545558977290663, 24.09562519341298170, -0.9435640554424079562 ) ) ;
#37726 = CARTESIAN_POINT ( 'NONE',  ( -0.8313783143457759151, 22.10655722792919065, -0.5139362334944024280 ) ) ;
#37727 = VERTEX_POINT ( 'NONE', #7452 ) ;
#37728 = ORIENTED_EDGE ( 'NONE', *, *, #16581, .T. ) ;
#37729 = DIRECTION ( 'NONE',  ( -0.01997839162482764261, -1.040247600000952381E-18, 0.9998004120163609398 ) ) ;
#37730 = CARTESIAN_POINT ( 'NONE',  ( 1.302594956492339584, 113.6455945353133643, 2.391525302099168471 ) ) ;
#37731 =( LENGTH_UNIT ( ) NAMED_UNIT ( * ) SI_UNIT ( .MILLI., .METRE. ) );
#37732 = CARTESIAN_POINT ( 'NONE',  ( -8.687188811298957702, 122.3401343867201945, 0.7349857017399259451 ) ) ;
#37733 = CARTESIAN_POINT ( 'NONE',  ( -43.26072228752227744, 21.85338980287131605, 2.263362209153686244 ) ) ;
#37734 = CARTESIAN_POINT ( 'NONE',  ( 3.022112892507086812, -12.39725416092116106, 0.4273193741429963666 ) ) ;
#37735 = CARTESIAN_POINT ( 'NONE',  ( 18.17603978048560620, 146.7121067869193496, -1.621728993581971645 ) ) ;
#37736 = CARTESIAN_POINT ( 'NONE',  ( -2.242647228084525324, 118.4336326928681729, -0.7879290844312367703 ) ) ;
#37737 = CYLINDRICAL_SURFACE ( 'NONE', #32451, 6.350000000000004974 ) ;
#37738 = B_SPLINE_CURVE_WITH_KNOTS ( 'NONE', 3,
 ( #23083, #10535, #13734, #4382 ),
 .UNSPECIFIED., .F., .F.,
 ( 4, 4 ),
 ( 0.000000000000000000, 0.9716004430332778607 ),
 .UNSPECIFIED. ) ;
#37739 = CARTESIAN_POINT ( 'NONE',  ( -4.873850642958227120, 32.38564726215445688, 3.744354677719523572 ) ) ;
#37740 = CARTESIAN_POINT ( 'NONE',  ( 4.537977675602582472, 121.1059516323014549, -0.1178196913276177149 ) ) ;
#37741 = VERTEX_POINT ( 'NONE', #29603 ) ;
#37742 = CARTESIAN_POINT ( 'NONE',  ( 1.979187190576821465, -15.21425526833739639, 5.301287498526151332 ) ) ;
#37743 = CARTESIAN_POINT ( 'NONE',  ( 4.979814073991923884, 117.5943741255363477, 0.7446744892861771881 ) ) ;
#37744 = CARTESIAN_POINT ( 'NONE',  ( -58.62884620442479644, -0.7615560826029293962, 0.07633319197526360067 ) ) ;
#37745 = CARTESIAN_POINT ( 'NONE',  ( -4.567530434605131084, -10.44214056487004250, 0.7003524306260878740 ) ) ;
#37746 = CARTESIAN_POINT ( 'NONE',  ( 8.727673846237058441, 154.8283212766472445, 1.585547369736020062 ) ) ;
#37747 = CARTESIAN_POINT ( 'NONE',  ( 2.944162091193518904, 38.75495963859787452, 0.7149833688506975760 ) ) ;
#37748 = CARTESIAN_POINT ( 'NONE',  ( -1.576215671565407650, 106.2483430537416638, 5.109971884176318646 ) ) ;
#37749 = CARTESIAN_POINT ( 'NONE',  ( -0.5496829067194369811, 0.7180641350488168317, -4.598301960397928489 ) ) ;
#37750 = CARTESIAN_POINT ( 'NONE',  ( -2.579283729523311308, 34.63205429821886838, 0.7922911722492685938 ) ) ;
#37751 = CARTESIAN_POINT ( 'NONE',  ( 4.653112868187331941, 2.303567304790777648, 7.043327697551765354 ) ) ;
#37752 = CARTESIAN_POINT ( 'NONE',  ( -57.38720131040756200, 1.641502911523470942, -0.7119259365333358014 ) ) ;
#37753 = CARTESIAN_POINT ( 'NONE',  ( 8.775998379516696701, 117.8320079785639365, -0.2360308319456460580 ) ) ;
#37754 = CARTESIAN_POINT ( 'NONE',  ( -0.3606724330769058295, 121.2597428844643161, -0.4428036157107447801 ) ) ;
#37755 = FACE_OUTER_BOUND ( 'NONE', #15962, .T. ) ;
#37756 = FACE_OUTER_BOUND ( 'NONE', #2598, .T. ) ;
#37757 = CARTESIAN_POINT ( 'NONE',  ( 4.619096255015035624, 27.05588869245799089, -0.3994036469054788596 ) ) ;
#37758 = CARTESIAN_POINT ( 'NONE',  ( -0.02983097946891679134, 117.3993836135855702, 1.492864285907040456 ) ) ;
#37759 = CARTESIAN_POINT ( 'NONE',  ( -19.33375693323417366, 80.42273151551299293, 1.269999999999995577 ) ) ;
#37760 = CARTESIAN_POINT ( 'NONE',  ( -58.83227707057486811, -0.08366279997996939333, -1.539018077965326743E-14 ) ) ;
#37761 = CARTESIAN_POINT ( 'NONE',  ( 0.9377939088480686802, 122.9246775559910390, -0.1697371007065931747 ) ) ;
#37762 = CARTESIAN_POINT ( 'NONE',  ( -4.803851041827917001, 116.9482543694763166, 0.2466672064845016887 ) ) ;
#37763 = ORIENTED_EDGE ( 'NONE', *, *, #8676, .F. ) ;
#37764 = CARTESIAN_POINT ( 'NONE',  ( -58.64217253742437208, 0.4108157498741576985, -0.3978973257256673279 ) ) ;
#37765 = ORIENTED_EDGE ( 'NONE', *, *, #13693, .T. ) ;
#37766 = CARTESIAN_POINT ( 'NONE',  ( -47.20408514806585742, 20.03888983422004344, -5.082056583519131365 ) ) ;
#37767 = CARTESIAN_POINT ( 'NONE',  ( -8.027194241900888372, 122.8503413726703428, -0.1191878892407382262 ) ) ;
#37768 = CARTESIAN_POINT ( 'NONE',  ( 3.423347803338410156, -15.46749709811699702, 5.412694551837634371 ) ) ;
#37769 = CARTESIAN_POINT ( 'NONE',  ( -2.188165212810393445, 117.9909145081919917, 0.6446704472730119262 ) ) ;
#37770 = CARTESIAN_POINT ( 'NONE',  ( 15.97727112977735686, 122.8751182158008959, -0.7600457325971274880 ) ) ;
#37771 = CARTESIAN_POINT ( 'NONE',  ( 3.935102970030661673, 16.48578375386999539, 2.424025302511324309 ) ) ;
#37772 = CARTESIAN_POINT ( 'NONE',  ( -6.906622810364809517, 117.2343425291504104, -0.3847307661620059105 ) ) ;
#37773 = CARTESIAN_POINT ( 'NONE',  ( -50.06326276805182118, 16.19468026859921039, -4.911295769374709685 ) ) ;
#37774 = EDGE_LOOP ( 'NONE', ( #33998, #12134, #41568, #26662 ) ) ;
#37775 = CARTESIAN_POINT ( 'NONE',  ( 8.797618036347394366, 117.6845732567335290, 0.1950281128173915746 ) ) ;
#37776 = FACE_OUTER_BOUND ( 'NONE', #37106, .T. ) ;
#37777 = B_SPLINE_SURFACE_WITH_KNOTS ( 'NONE', 1, 3, ( 
 ( #34251, #31033, #11650, #14836, #34454, #8884, #34662, #5490, #21636, #37853, #27630, #8471 ),
 ( #5081, #38067, #40641, #34876, #31672, #11435, #15260, #1671, #18237, #2082, #21426, #21221 ) ),
 .UNSPECIFIED., .F., .F., .F.,
 ( 2, 2 ),
 ( 4, 3, 2, 3, 4 ),
 ( 0.000000000000000000, 1.000000000000000000 ),
 ( -0.01866551247456825838, 0.000000000000000000, 0.5000000000000000000, 1.000000000000000000, 1.010000000000000009 ),
 .UNSPECIFIED. ) ;
#37778 = CARTESIAN_POINT ( 'NONE',  ( -10.46700094992505647, 122.9580799906392343, 1.049763322952065758 ) ) ;
#37779 = CARTESIAN_POINT ( 'NONE',  ( -53.97752642499204967, 8.868598658150437686, -3.466679480857036477 ) ) ;
#37780 = CARTESIAN_POINT ( 'NONE',  ( 8.634969826328919851, 120.3810071108087243, -1.137220218559220619 ) ) ;
#37781 = CARTESIAN_POINT ( 'NONE',  ( -1.172210521474351452, 158.9035955689636523, -1.423060353815112089 ) ) ;
#37782 = CARTESIAN_POINT ( 'NONE',  ( -52.97391985390434144, 12.30611266682019789, -4.247241762254921227 ) ) ;
#37783 = CARTESIAN_POINT ( 'NONE',  ( 8.467456592458612263, 122.5794309061019618, -0.5337204191277989951 ) ) ;
#37784 = ORIENTED_EDGE ( 'NONE', *, *, #29434, .T. ) ;
#37785 = CARTESIAN_POINT ( 'NONE',  ( -11.12287255170445022, 123.1247571232444784, -1.608126361149618821 ) ) ;
#37786 = CARTESIAN_POINT ( 'NONE',  ( 2.046246934637348858, -15.60107924929197942, 5.318501171315276999 ) ) ;
#37787 = DIRECTION ( 'NONE',  ( -5.188838149069471174E-16, 1.699382548006136313E-16, 1.000000000000000000 ) ) ;
#37788 = CARTESIAN_POINT ( 'NONE',  ( -58.03414100541874632, 0.4564111095344686175, -0.9708715263941700702 ) ) ;
#37789 = CARTESIAN_POINT ( 'NONE',  ( -4.950256445730226496, 117.4773595571565608, 0.8982803358397978277 ) ) ;
#37790 = CARTESIAN_POINT ( 'NONE',  ( 16.72996320514137736, 149.5530097695598215, 2.252745029998448167 ) ) ;
#37791 = CARTESIAN_POINT ( 'NONE',  ( -14.60500000000000043, 71.11999999999999034, 1.904999999999990701 ) ) ;
#37792 = EDGE_CURVE ( 'NONE', #22227, #41583, #11325, .T. ) ;
#37793 = CARTESIAN_POINT ( 'NONE',  ( -7.483757832938788823, -7.479835662595867518, -3.861840502031824940 ) ) ;
#37794 = CARTESIAN_POINT ( 'NONE',  ( 9.737435037572364394, 124.8671652961716489, 0.4371131421146306484 ) ) ;
#37795 = DIRECTION ( 'NONE',  ( -0.7770581983690878491, 0.6294287539883980376, -5.101669463485847584E-16 ) ) ;
#37797 = EDGE_LOOP ( 'NONE', ( #12206, #37308, #31082, #4327 ) ) ;
#37796 = CARTESIAN_POINT ( 'NONE',  ( -44.09535491252989203, 20.89266065238331294, -2.220044762595793753 ) ) ;
#37798 = CARTESIAN_POINT ( 'NONE',  ( 15.50061618130081165, 62.14374591690594940, -1.904999999999999583 ) ) ;
#37799 = FACE_OUTER_BOUND ( 'NONE', #33215, .T. ) ;
#37800 = LINE ( 'NONE', #34618, #13339 ) ;
#37801 = CARTESIAN_POINT ( 'NONE',  ( -50.73416975447392474, 21.22185706673585059, 0.7846160747444976824 ) ) ;
#37802 = EDGE_CURVE ( 'NONE', #34625, #32786, #25264, .T. ) ;
#37803 = CARTESIAN_POINT ( 'NONE',  ( -16.06481930096632027, 121.2308719818149712, -0.1605585295567894255 ) ) ;
#37804 = AXIS2_PLACEMENT_3D ( 'NONE', #36163, #13572, #29964 ) ;
#37805 = ORIENTED_EDGE ( 'NONE', *, *, #28238, .F. ) ;
#37806 = CARTESIAN_POINT ( 'NONE',  ( -50.57586884603683330, 21.47051451305503988, -0.7809936997224710131 ) ) ;
#37807 = CARTESIAN_POINT ( 'NONE',  ( 6.887288372000457848, 121.6289117458970850, -0.4154818992412157019 ) ) ;
#37808 = CARTESIAN_POINT ( 'NONE',  ( 16.04309792416813707, 12.96416000000000146, 5.016499999999999737 ) ) ;
#37809 = ORIENTED_EDGE ( 'NONE', *, *, #2569, .F. ) ;
#37810 = CARTESIAN_POINT ( 'NONE',  ( 0.7417783677999320036, 115.6909491485452719, -1.732018146620468046 ) ) ;
#37811 = CARTESIAN_POINT ( 'NONE',  ( -3.706155879762023098, 121.0264708767875561, -0.2234555574396432376 ) ) ;
#37812 = CARTESIAN_POINT ( 'NONE',  ( 4.778253948640466042, -14.19231145175180231, 4.234097743872750286 ) ) ;
#37813 = CARTESIAN_POINT ( 'NONE',  ( -12.48318382086466904, 120.3283006479967128, 0.8937555771000559313 ) ) ;
#37814 = CARTESIAN_POINT ( 'NONE',  ( -6.573280687130626123E-14, 88.99346620154574339, 1.699031322814114629E-29 ) ) ;
#37815 = CARTESIAN_POINT ( 'NONE',  ( 15.60991558517063815, 120.8175431576145940, 0.4704071646738435253 ) ) ;
#37816 = CARTESIAN_POINT ( 'NONE',  ( 1.623171908765614901, 120.9965112475868096, 0.06597297138143794204 ) ) ;
#37817 = DIRECTION ( 'NONE',  ( -0.4849315768086534528, -0.8745520943968250194, -1.030032898892974942E-16 ) ) ;
#37818 = CARTESIAN_POINT ( 'NONE',  ( 0.9750733387068674096, 18.20995955126885590, -0.03652159252302569076 ) ) ;
#37819 = CARTESIAN_POINT ( 'NONE',  ( -15.52158573417678511, 120.7153972339879715, -0.3606909788719010468 ) ) ;
#37820 = CARTESIAN_POINT ( 'NONE',  ( -41.08171237912073792, 23.06270199366203855, -1.270028482463944064 ) ) ;
#37821 = DIRECTION ( 'NONE',  ( -0.8745520943968225769, 0.4849315768086576717, -5.691349986800551823E-16 ) ) ;
#37822 = PRODUCT_RELATED_PRODUCT_CATEGORY ( 'part', '', ( #30001 ) ) ;
#37823 = ORIENTED_EDGE ( 'NONE', *, *, #6349, .T. ) ;
#37824 = CARTESIAN_POINT ( 'NONE',  ( -2.917723067105041146, 117.2534023856253782, 0.5932563568887373462 ) ) ;
#37825 = CARTESIAN_POINT ( 'NONE',  ( -19.68500000000000227, 71.11999999999999034, -1.904999999999999583 ) ) ;
#37826 = CARTESIAN_POINT ( 'NONE',  ( 14.28642979620150300, 121.5541609676003389, 1.504719748795722234 ) ) ;
#37827 = CARTESIAN_POINT ( 'NONE',  ( -57.83370854706699760, 0.8645507274500918715, -1.063039573801316307 ) ) ;
#37828 = CARTESIAN_POINT ( 'NONE',  ( 13.37375235405023588, 122.3357896625302459, -1.257830042033918128 ) ) ;
#37829 = CARTESIAN_POINT ( 'NONE',  ( 1.466575460758787530, 20.86946789039323491, 8.308456332865098659 ) ) ;
#37830 = CARTESIAN_POINT ( 'NONE',  ( -15.68124023389198385, 122.9504679175852573, -1.501494826411869932 ) ) ;
#37831 = CARTESIAN_POINT ( 'NONE',  ( 4.902322516856424173, 117.7191841120239673, -0.7486650477168125262 ) ) ;
#37832 = CARTESIAN_POINT ( 'NONE',  ( 5.211883163658348472, 116.1034411669277375, 1.237845179234434267 ) ) ;
#37833 = EDGE_CURVE ( 'NONE', #33026, #10948, #39241, .T. ) ;
#37834 = EDGE_LOOP ( 'NONE', ( #27445, #39843, #29519, #6010 ) ) ;
#37835 = CARTESIAN_POINT ( 'NONE',  ( -0.6395209782510218322, 120.9735524437166561, 0.05055770394172671295 ) ) ;
#37836 = CARTESIAN_POINT ( 'NONE',  ( -12.03045567952079331, 122.8144071692085504, -1.784322758991244040 ) ) ;
#37837 = EDGE_CURVE ( 'NONE', #5531, #10519, #14859, .T. ) ;
#37838 = CARTESIAN_POINT ( 'NONE',  ( 3.031078967112608158, -15.50598464685963584, 5.611516622434578494 ) ) ;
#37839 = DIRECTION ( 'NONE',  ( -1.000000000000000000, 1.177520686924251719E-16, 0.000000000000000000 ) ) ;
#37840 = EDGE_CURVE ( 'NONE', #11774, #5717, #17849, .T. ) ;
#37841 = AXIS2_PLACEMENT_3D ( 'NONE', #34957, #38769, #22549 ) ;
#37842 = LINE ( 'NONE', #21627, #32201 ) ;
#37844 = EDGE_LOOP ( 'NONE', ( #24738, #10369, #1917, #37405 ) ) ;
#37843 = VECTOR ( 'NONE', #5581, 1000.000000000000114 ) ;
#37845 = CARTESIAN_POINT ( 'NONE',  ( 18.63996327081343907, 147.1333978507680627, 2.447832456508666876 ) ) ;
#37846 = CIRCLE ( 'NONE', #28990, 3.683000000000001162 ) ;
#37847 = LINE ( 'NONE', #12070, #7952 ) ;
#37848 = DIRECTION ( 'NONE',  ( -0.8745520943968235761, 0.4849315768086558398, -4.268512490100410909E-16 ) ) ;
#37849 = CARTESIAN_POINT ( 'NONE',  ( -1.135428393696731098, 110.6314368487224300, 3.415474402745806604 ) ) ;
#37850 = B_SPLINE_CURVE_WITH_KNOTS ( 'NONE', 3,
 ( #20623, #36634, #11893, #22088, #8702, #18265, #18901, #9127, #21665, #28074, #24882, #21452, #2326, #31481, #12315, #35115, #34482, #2748, #41085, #37879, #31698, #14864, #15286, #5942, #31911, #15703, #5314, #28291, #34689, #1901, #25091, #41717, #25303, #5518, #31268, #18476 ),
 .UNSPECIFIED., .F., .F.,
 ( 4, 2, 2, 2, 2, 2, 2, 2, 2, 2, 2, 2, 2, 2, 2, 2, 2, 4 ),
 ( 0.02988307654956906881, 0.03083251118258813206, 0.03178194581560719878, 0.03273138044862625856, 0.03368081508164531834, 0.03463024971466438506, 0.03557968434768345178, 0.03652911898070251157, 0.03747855361372157829, 0.03842798824674063807, 0.03937742287975970479, 0.04032685751277876457, 0.04127629214579783129, 0.04222572677881689801, 0.04270044409532643137, 0.04317516141183595779, 0.04412459604485502451, 0.04507403067787408429 ),
 .UNSPECIFIED. ) ;
#37851 = CARTESIAN_POINT ( 'NONE',  ( -6.736519641741455899, -9.595509028896938020, 5.111951147309959254 ) ) ;
#37852 = CARTESIAN_POINT ( 'NONE',  ( 7.104091076028325347, 121.8059686962219672, 0.6844636119373688210 ) ) ;
#37853 = CARTESIAN_POINT ( 'NONE',  ( -5.240108103846050192, 115.6909491485453003, -1.021770142138806792 ) ) ;
#37854 = CARTESIAN_POINT ( 'NONE',  ( 7.827178552123568167, 158.6358315003295161, -0.5664908120210206954 ) ) ;
#37855 = CARTESIAN_POINT ( 'NONE',  ( 4.965996940879040977, 56.51499999999996504, -4.710730864944427942 ) ) ;
#37856 = CARTESIAN_POINT ( 'NONE',  ( -58.17408770762806114, 0.1276510453498960473, 0.6006340682012513144 ) ) ;
#37857 = CARTESIAN_POINT ( 'NONE',  ( -32.35164496306255444, 51.35586489404142441, -1.524000000000005794 ) ) ;
#37858 = DIRECTION ( 'NONE',  ( -0.6294287539884133587, -0.7770581983690755257, 0.000000000000000000 ) ) ;
#37859 = CARTESIAN_POINT ( 'NONE',  ( -4.117464183752013618, 118.2429491485453354, 0.1872741133385840973 ) ) ;
#37860 = FACE_OUTER_BOUND ( 'NONE', #21485, .T. ) ;
#37861 = ORIENTED_EDGE ( 'NONE', *, *, #42074, .T. ) ;
#37862 = CARTESIAN_POINT ( 'NONE',  ( -51.02479983779974049, 14.46739584830851477, 4.600955224801048793 ) ) ;
#37863 = CARTESIAN_POINT ( 'NONE',  ( -8.238205950790057130, 120.2908699818124916, -1.444131204026530391 ) ) ;
#37864 = CARTESIAN_POINT ( 'NONE',  ( 5.299048467822902175, 104.6144662015457527, -1.294354682138050050 ) ) ;
#37865 = CARTESIAN_POINT ( 'NONE',  ( -1.678671165333144533, 156.3322054215483092, -0.6622483832023352557 ) ) ;
#37866 = CARTESIAN_POINT ( 'NONE',  ( 4.907841372110366862, 117.4079477242360525, -0.9677383763118554416 ) ) ;
#37867 = LINE ( 'NONE', #8486, #24598 ) ;
#37868 = ORIENTED_EDGE ( 'NONE', *, *, #564, .T. ) ;
#37869 = CARTESIAN_POINT ( 'NONE',  ( 0.4746723515649934888, 24.68197512780947278, 4.609222710213416896 ) ) ;
#37870 = CARTESIAN_POINT ( 'NONE',  ( -6.756648348127426651, 78.81597664337222398, 3.183520453979958642 ) ) ;
#37871 = DIRECTION ( 'NONE',  ( -0.8745520943968240202, 0.4849315768086553402, -5.361993529360572958E-16 ) ) ;
#37872 = CARTESIAN_POINT ( 'NONE',  ( -42.18235783619532953, 22.15054559413689006, 1.778153187293267434 ) ) ;
#37873 = EDGE_CURVE ( 'NONE', #25568, #28106, #1131, .T. ) ;
#37874 = CIRCLE ( 'NONE', #33114, 5.588000000000006295 ) ;
#37875 = CARTESIAN_POINT ( 'NONE',  ( -48.24242213954391900, 19.61027420771482355, 5.299259492517840009 ) ) ;
#37876 = CARTESIAN_POINT ( 'NONE',  ( 7.785935935534881835, 122.6147637717617727, 0.2294641480035215786 ) ) ;
#37877 = CARTESIAN_POINT ( 'NONE',  ( -4.580899860306842264, 27.87760619330545708, 0.5121266511161914892 ) ) ;
#37878 = CARTESIAN_POINT ( 'NONE',  ( 16.43260349481032279, 122.7513851185756693, 1.135385547233646264 ) ) ;
#37879 = CARTESIAN_POINT ( 'NONE',  ( 0.8484574697436598756, 104.6144662015457243, -4.760796931819447408 ) ) ;
#37881 = CARTESIAN_POINT ( 'NONE',  ( 1.249041419371635930, 159.0162744061759099, -1.301773431059132458 ) ) ;
#37880 = CARTESIAN_POINT ( 'NONE',  ( 2.670684053127368784, -15.04618456763519241, 4.548342027319769443 ) ) ;
#37882 = CARTESIAN_POINT ( 'NONE',  ( -12.69375283655744724, 153.7453525671159298, 1.672805011026381017 ) ) ;
#37883 = CARTESIAN_POINT ( 'NONE',  ( 4.466176584706416541, 22.48015689762229030, 1.290832665783417488 ) ) ;
#37884 = CARTESIAN_POINT ( 'NONE',  ( -6.894332492628214126, 117.4533518774869947, -0.6472591412684409740 ) ) ;
#37885 = CARTESIAN_POINT ( 'NONE',  ( 0.3177745610913299545, 14.38516025884261929, -0.9235644396001725376 ) ) ;
#37886 = ORIENTED_EDGE ( 'NONE', *, *, #9514, .T. ) ;
#37887 = CARTESIAN_POINT ( 'NONE',  ( -56.89722832398061314, 2.603431824206650536, 0.9028745487782365853 ) ) ;
#37888 = CARTESIAN_POINT ( 'NONE',  ( -4.520495148373047556, 121.0527503406816123, 0.1761357111252132845 ) ) ;
#37889 = CARTESIAN_POINT ( 'NONE',  ( 5.611934155553572445, -13.19144435144412064, 2.399925970747030846 ) ) ;
#37890 = CARTESIAN_POINT ( 'NONE',  ( 16.77072586670511356, 146.3384789841921361, -1.111521918641044104 ) ) ;
#37891 = ORIENTED_EDGE ( 'NONE', *, *, #29465, .T. ) ;
#37892 = CIRCLE ( 'NONE', #41981, 0.5080000000000000071 ) ;
#37893 = CARTESIAN_POINT ( 'NONE',  ( 1.287233266581064184, 115.7028696085538115, 1.739241353082145780 ) ) ;
#37894 = AXIS2_PLACEMENT_3D ( 'NONE', #5683, #9484, #31646 ) ;
#37895 = ADVANCED_FACE ( 'NONE', ( #31264 ), #6559, .T. ) ;
#37896 = CARTESIAN_POINT ( 'NONE',  ( -4.721710813556387443, 117.8486367688393557, -1.008509401085505575 ) ) ;
#37897 = CARTESIAN_POINT ( 'NONE',  ( 9.001127587916124995, 123.9218113011205986, 0.09563458650452050236 ) ) ;
#37898 = ORIENTED_EDGE ( 'NONE', *, *, #36293, .F. ) ;
#37899 = CARTESIAN_POINT ( 'NONE',  ( 12.76651978940611620, 122.1393999080170971, 1.787974849574114122 ) ) ;
#37900 = DIRECTION ( 'NONE',  ( -0.9998004120163609398, -4.016384292689130894E-17, -0.01997839162482749689 ) ) ;
#37901 = CIRCLE ( 'NONE', #35876, 0.7620000000000000107 ) ;
#37902 = CARTESIAN_POINT ( 'NONE',  ( 17.14499999999999957, 71.11999999999999034, 1.904999999999989146 ) ) ;
#37903 = CARTESIAN_POINT ( 'NONE',  ( 0.02399864187730229442, 159.1630378086529731, -1.200990174154242141 ) ) ;
#37904 = CIRCLE ( 'NONE', #12724, 0.5080000000000002292 ) ;
#37905 = CARTESIAN_POINT ( 'NONE',  ( 15.31729018078742932, 120.6995131204970875, -0.01165691202436091103 ) ) ;
#37906 = CARTESIAN_POINT ( 'NONE',  ( 0.06282972276035359016, 111.5577547982949227, -3.144256248693377387 ) ) ;
#37907 = CARTESIAN_POINT ( 'NONE',  ( 1.796294892211930838, -15.43586790762843641, 5.400043117830624517 ) ) ;
#37908 = DIRECTION ( 'NONE',  ( -0.8745520943968251304, 0.4849315768086535638, 5.226292508699495262E-15 ) ) ;
#37909 = FACE_OUTER_BOUND ( 'NONE', #32167, .T. ) ;
#37910 = CARTESIAN_POINT ( 'NONE',  ( -4.692573795977630802, 117.8898090967043402, 0.8100504932816339210 ) ) ;
#37911 = ORIENTED_EDGE ( 'NONE', *, *, #38386, .F. ) ;
#37912 = ORIENTED_EDGE ( 'NONE', *, *, #3337, .F. ) ;
#37913 = CARTESIAN_POINT ( 'NONE',  ( -23.69188486464780752, 78.08202335040543574, -1.524000000000005350 ) ) ;
#37914 = CARTESIAN_POINT ( 'NONE',  ( 5.858941820532026057, 118.8838138049209050, -1.014455745328361802 ) ) ;
#37915 = CARTESIAN_POINT ( 'NONE',  ( -0.09082259786515388400, 105.9597790263619146, -5.306270932934927131 ) ) ;
#37916 = CARTESIAN_POINT ( 'NONE',  ( 4.899517741242162217, 117.6566515308719829, 0.9517905942164465172 ) ) ;
#37917 = DIRECTION ( 'NONE',  ( -0.1715592850456333085, 0.1224830539174543292, -0.9775302108976914317 ) ) ;
#37918 = CARTESIAN_POINT ( 'NONE',  ( -0.7687070661362833679, 118.7604188656930120, 0.8775891873661260112 ) ) ;
#37919 = AXIS2_PLACEMENT_3D ( 'NONE', #16762, #39793, #23565 ) ;
#37920 = CARTESIAN_POINT ( 'NONE',  ( -17.14500000000466784, 71.11999999999886768, -1.524000000000000909 ) ) ;
#37921 = CARTESIAN_POINT ( 'NONE',  ( -4.774057941417253481, 114.7514248375596111, 1.662848932301731031 ) ) ;
#37922 = DIRECTION ( 'NONE',  ( -4.017660918040594346E-17, 1.000000000000000000, 2.376309959284834438E-19 ) ) ;
#37923 = CARTESIAN_POINT ( 'NONE',  ( 2.851896361732738860, -14.59419570037479019, 4.638016276237491020 ) ) ;
#37924 = CARTESIAN_POINT ( 'NONE',  ( 7.563607548680719717, 124.2956292408697863, 0.1420234171030815562 ) ) ;
#37925 = CARTESIAN_POINT ( 'NONE',  ( -11.90495122372371384, 153.4554508723442439, -1.948344234133813080 ) ) ;
#37926 = CARTESIAN_POINT ( 'NONE',  ( 7.000096156874491271, 121.9564310754924321, 0.1322597535296755333 ) ) ;
#37927 = CARTESIAN_POINT ( 'NONE',  ( -0.01632536679074437017, 38.84944212800221663, 1.323018725044087018 ) ) ;
#37928 = CARTESIAN_POINT ( 'NONE',  ( -0.08720133927422249465, 115.7029491485439792, 1.760460350643238581 ) ) ;
#37929 = CARTESIAN_POINT ( 'NONE',  ( 1.719524320724281852, 5.915668354077111779, 4.300554535892874064 ) ) ;
#37931 = ORIENTED_EDGE ( 'NONE', *, *, #33723, .T. ) ;
#37930 = CARTESIAN_POINT ( 'NONE',  ( 22.52188062635569565, 150.6069110094195764, 1.039808695286016382 ) ) ;
#37932 = CARTESIAN_POINT ( 'NONE',  ( -1.649594635467665826, 104.6144662015457527, -4.544680953048276351 ) ) ;
#37933 = CARTESIAN_POINT ( 'NONE',  ( 3.954393197012034733, -15.56809308616131915, 2.853032214330836869 ) ) ;
#37934 = CARTESIAN_POINT ( 'NONE',  ( -2.359155998022535172, 118.9063233352275972, 0.7056007782052504673 ) ) ;
#37935 = CARTESIAN_POINT ( 'NONE',  ( -0.03357488772870852872, 24.54038786010652728, -0.9749811203568246043 ) ) ;
#37936 = CARTESIAN_POINT ( 'NONE',  ( 0.1941685572964340079, 16.06069190514159928, 0.9568941237268799860 ) ) ;
#37937 = ORIENTED_EDGE ( 'NONE', *, *, #5220, .F. ) ;
#37938 = EDGE_LOOP ( 'NONE', ( #88, #3359, #40922, #2680 ) ) ;
#37939 = DIRECTION ( 'NONE',  ( -0.000000000000000000, -0.000000000000000000, -1.000000000000000000 ) ) ;
#37940 = CIRCLE ( 'NONE', #26347, 0.7620000000000015650 ) ;
#37941 = CARTESIAN_POINT ( 'NONE',  ( 3.617430929662223349, 113.7286232773062125, 2.299356966923025158 ) ) ;
#37942 =( LENGTH_UNIT ( ) NAMED_UNIT ( * ) SI_UNIT ( .MILLI., .METRE. ) );
#37943 = CARTESIAN_POINT ( 'NONE',  ( -16.32790441640426238, 146.1553843108282820, 0.7912819366082540773 ) ) ;
#37944 = DIRECTION ( 'NONE',  ( 5.188838149069472160E-16, -1.699382548006136559E-16, -1.000000000000000000 ) ) ;
#37945 = EDGE_CURVE ( 'NONE', #1503, #5200, #11889, .T. ) ;
#37946 = CARTESIAN_POINT ( 'NONE',  ( 2.175557056806384448, -14.94057515128023539, 5.440454282391695706 ) ) ;
#37947 = CARTESIAN_POINT ( 'NONE',  ( 7.718355369771759733, 156.1362479297160348, -1.656311413603696936 ) ) ;
#37948 = CARTESIAN_POINT ( 'NONE',  ( -12.93098116229908001, 122.2940260782629451, -1.802317002068888785 ) ) ;
#37949 = FACE_OUTER_BOUND ( 'NONE', #636, .T. ) ;
#37950 = EDGE_CURVE ( 'NONE', #12622, #38820, #33416, .T. ) ;
#37951 = CARTESIAN_POINT ( 'NONE',  ( -15.72550100231863368, 145.6881679641610674, -0.3142329346387550681 ) ) ;
#37952 = CARTESIAN_POINT ( 'NONE',  ( -4.970415085658511423, 32.57053289346710301, 3.417355655074298948 ) ) ;
#37953 = CARTESIAN_POINT ( 'NONE',  ( 6.107944937931459428, 155.3491548655973133, -0.3423801154807229463 ) ) ;
#37954 = VERTEX_POINT ( 'NONE', #11050 ) ;
#37955 = CARTESIAN_POINT ( 'NONE',  ( 2.232013814210268343, -15.18320146713449148, 5.067049754691558050 ) ) ;
#37956 = DIRECTION ( 'NONE',  ( 0.1469470846586743706, -1.414713986243376972E-17, -0.9891443546370348727 ) ) ;
#37957 = FACE_OUTER_BOUND ( 'NONE', #28740, .T. ) ;
#37958 = PRESENTATION_LAYER_ASSIGNMENT (  '', '', ( #28430 ) ) ;
#37959 = CARTESIAN_POINT ( 'NONE',  ( -58.44555280191302415, -0.4200408777295304152, 0.3231375529342178643 ) ) ;
#37960 = CARTESIAN_POINT ( 'NONE',  ( 3.573240411403531436, -4.819783300376494495, -2.961220487682876268 ) ) ;
#37961 = CARTESIAN_POINT ( 'NONE',  ( 16.69533394573240770, 146.9696287467501179, 1.777152765835339876 ) ) ;
#37962 = DIRECTION ( 'NONE',  ( -0.000000000000000000, -0.000000000000000000, -1.000000000000000000 ) ) ;
#37963 = CARTESIAN_POINT ( 'NONE',  ( -5.736215069875440165, 118.4654530710369329, 0.4324765805296821308 ) ) ;
#37964 = CARTESIAN_POINT ( 'NONE',  ( -2.983771112188844832, -5.329111280313512999, 3.548611825089460048 ) ) ;
#37965 = CARTESIAN_POINT ( 'NONE',  ( 13.59117098933499790, 150.2425924485890505, 0.2715839415562140702 ) ) ;
#37966 = CARTESIAN_POINT ( 'NONE',  ( -3.806420843250353681, -2.673146571556306750, -7.510622214715559686 ) ) ;
#37967 = CARTESIAN_POINT ( 'NONE',  ( -57.43023524350843445, 1.739013888464230329, -1.477089945056109910 ) ) ;
#37968 = CARTESIAN_POINT ( 'NONE',  ( 5.541113904439527005, 116.8730092650452974, -0.3263445822601490076 ) ) ;
#37969 = CARTESIAN_POINT ( 'NONE',  ( 0.04081796247057428717, 114.7739974199301969, -2.042697753608746059 ) ) ;
#37970 = DIRECTION ( 'NONE',  ( -0.8745520943968250194, 0.4849315768086534528, -5.361993529360573944E-16 ) ) ;
#37971 = CARTESIAN_POINT ( 'NONE',  ( -4.873850642958228008, 32.38564726215445688, 3.744354677719523572 ) ) ;
#37972 = CARTESIAN_POINT ( 'NONE',  ( -3.290491044589036740, 30.52917213649525507, -3.264312889705288878 ) ) ;
#37973 = CARTESIAN_POINT ( 'NONE',  ( 3.153090565069621487, 117.9394477917076784, 1.303659228010183080 ) ) ;
#37974 = CYLINDRICAL_SURFACE ( 'NONE', #4935, 5.334000000000001407 ) ;
#37975 = FACE_OUTER_BOUND ( 'NONE', #3994, .T. ) ;
#37976 = CARTESIAN_POINT ( 'NONE',  ( 0.4103500344925852250, 124.0591982226670211, -0.08506156519360527635 ) ) ;
#37977 = CARTESIAN_POINT ( 'NONE',  ( -14.51632629332725699, 120.3567457872619997, 0.2133257594814961799 ) ) ;
#37978 = B_SPLINE_CURVE_WITH_KNOTS ( 'NONE', 3,
 ( #27888, #34507, #28312, #41320, #12124, #25114 ),
 .UNSPECIFIED., .F., .F.,
 ( 4, 2, 4 ),
 ( 0.000000000000000000, 0.0003611586812565004178, 0.0007223173625130008355 ),
 .UNSPECIFIED. ) ;
#37979 = EDGE_LOOP ( 'NONE', ( #4290, #37637, #19720, #5971 ) ) ;
#37980 = CARTESIAN_POINT ( 'NONE',  ( -58.03428750496626520, 2.144022121626010247, -1.074202927763570110E-14 ) ) ;
#37981 = ORIENTED_EDGE ( 'NONE', *, *, #27362, .T. ) ;
#37982 = DIRECTION ( 'NONE',  ( 5.188838149069472160E-16, -1.699382548006136559E-16, -1.000000000000000000 ) ) ;
#37983 = CARTESIAN_POINT ( 'NONE',  ( -15.26437740606669458, 148.0206351893604619, -0.2384670674966477832 ) ) ;
#37984 = CARTESIAN_POINT ( 'NONE',  ( 2.643346398695107347, -15.60183157139904964, 5.704389875863137505 ) ) ;
#37985 = CARTESIAN_POINT ( 'NONE',  ( -15.69714418277277268, 125.4375369430449609, 1.335551531390729130 ) ) ;
#37986 = PRODUCT_DEFINITION_FORMATION_WITH_SPECIFIED_SOURCE ( 'ANY', '', #29310, .NOT_KNOWN. ) ;
#37987 = CARTESIAN_POINT ( 'NONE',  ( 12.68208805480593604, 156.8164516032445306, -1.015108139269342402 ) ) ;
#37988 = CARTESIAN_POINT ( 'NONE',  ( 4.256838582791900194, 16.71066835407712858, 1.825063967593055558 ) ) ;
#37989 = CARTESIAN_POINT ( 'NONE',  ( -5.687008767712567803, 159.1209727096294273, -0.4156250475054875659 ) ) ;
#37990 = CARTESIAN_POINT ( 'NONE',  ( -57.26545915665239050, 2.636046494217942016, -1.996990251079107770 ) ) ;
#37991 = VERTEX_POINT ( 'NONE', #2106 ) ;
#37992 = CARTESIAN_POINT ( 'NONE',  ( -5.562874253636517885, 116.7208863047924012, 0.03685954551894467940 ) ) ;
#37993 = CARTESIAN_POINT ( 'NONE',  ( -23.49500000000000455, 71.11999999999999034, -5.016499999999999737 ) ) ;
#37994 = CARTESIAN_POINT ( 'NONE',  ( -10.76607124212195288, 123.2317624570580534, 1.067040512904773975 ) ) ;
#37995 = CARTESIAN_POINT ( 'NONE',  ( -50.47963954645450713, 15.37956391664342171, -4.696064106192690879 ) ) ;
#37996 = CARTESIAN_POINT ( 'NONE',  ( 13.42639911875428815, 154.0568829568526041, -1.747011766586976655 ) ) ;
#37997 = CARTESIAN_POINT ( 'NONE',  ( -1.123502178401431850, 117.8708904510121016, -0.6147983682407555106 ) ) ;
#37998 = CARTESIAN_POINT ( 'NONE',  ( -54.32300027520380326, 9.724537220608771904, -3.743864951777645445 ) ) ;
#37999 = B_SPLINE_CURVE_WITH_KNOTS ( 'NONE', 3,
 ( #9734, #15690, #35732, #22702, #19518, #15901, #3357, #16324, #29327, #13350 ),
 .UNSPECIFIED., .F., .F.,
 ( 4, 2, 2, 2, 4 ),
 ( 1.172921298844514755E-05, 0.0004645486371682156618, 0.0006909583492580865160, 0.0008041632053030119956, 0.0009173680613479374751 ),
 .UNSPECIFIED. ) ;
#38000 = EDGE_CURVE ( 'NONE', #3009, #4929, #11672, .T. ) ;
#38001 = CARTESIAN_POINT ( 'NONE',  ( 5.197063283114264465, 120.9449653624321144, -0.4048198106261541307 ) ) ;
#38002 = ORIENTED_EDGE ( 'NONE', *, *, #31641, .T. ) ;
#38003 = CARTESIAN_POINT ( 'NONE',  ( -17.63007963961423386, 148.6960320134204210, -2.325091492104032209 ) ) ;
#38004 = CARTESIAN_POINT ( 'NONE',  ( 1.896617635523351053, -15.61750365820154052, 5.464805439086081407 ) ) ;
#38005 = CIRCLE ( 'NONE', #3326, 6.350000000000004974 ) ;
#38006 = CARTESIAN_POINT ( 'NONE',  ( -4.160092557021775939, 118.2392543099457782, -0.3840812368330563942 ) ) ;
#38007 = CARTESIAN_POINT ( 'NONE',  ( -57.71946847630993460, 1.146847591362354368, -1.351507486235954403 ) ) ;
#38008 = CARTESIAN_POINT ( 'NONE',  ( -4.980827880492125992, 117.4083494260662661, 0.8692259800077603016 ) ) ;
#38009 = CARTESIAN_POINT ( 'NONE',  ( 10.58192191572908669, 122.8495954190337898, 1.525858888728604867 ) ) ;
#38010 = CARTESIAN_POINT ( 'NONE',  ( -11.67683074431529988, 78.22376516830392745, 1.270000000000000018 ) ) ;
#38011 = CARTESIAN_POINT ( 'NONE',  ( 5.949252453048933909, -3.155934468320678921, 5.972130579448434951 ) ) ;
#38012 = CARTESIAN_POINT ( 'NONE',  ( 15.41061421316642033, 147.8340308814284754, 0.6362464400602068082 ) ) ;
#38013 = CARTESIAN_POINT ( 'NONE',  ( -57.80205714066466527, 2.371715784325115095, -1.753227392946310470 ) ) ;
#38014 = CIRCLE ( 'NONE', #15535, 0.2540000000000000036 ) ;
#38016 = ORIENTED_EDGE ( 'NONE', *, *, #37945, .T. ) ;
#38015 = CARTESIAN_POINT ( 'NONE',  ( -41.05189575270515689, 23.09451173561988924, -0.6632222222222277086 ) ) ;
#38017 = CARTESIAN_POINT ( 'NONE',  ( -17.64290547347870941, 83.78857423953914463, 1.523999999999996247 ) ) ;
#38018 = DIRECTION ( 'NONE',  ( 0.6825627711659461028, 0.7308269722843185878, 2.299753143848302396E-16 ) ) ;
#38019 = CARTESIAN_POINT ( 'NONE',  ( -7.889001465740365759, 122.0455370848547290, -0.9156369006618222395 ) ) ;
#38020 = CARTESIAN_POINT ( 'NONE',  ( -5.241362157049148429, 88.73331249999999670, -5.310945289804168468 ) ) ;
#38021 = CARTESIAN_POINT ( 'NONE',  ( -50.95401363114979176, 21.69085172357045010, -9.625367201313238999E-15 ) ) ;
#38022 = CARTESIAN_POINT ( 'NONE',  ( -5.797208421814709745, 116.9567987913546006, 0.006983082090869513134 ) ) ;
#38023 = ORIENTED_EDGE ( 'NONE', *, *, #13028, .F. ) ;
#38024 = CARTESIAN_POINT ( 'NONE',  ( -49.85168879002940656, 22.56840098298264152, -0.7122439767497329433 ) ) ;
#38025 = CARTESIAN_POINT ( 'NONE',  ( 6.006691951566636156, 121.4393142041827787, 0.03230195852056535338 ) ) ;
#38026 = EDGE_CURVE ( 'NONE', #9800, #38197, #39900, .T. ) ;
#38027 = LINE ( 'NONE', #8210, #12178 ) ;
#38028 = ORIENTED_EDGE ( 'NONE', *, *, #33827, .F. ) ;
#38029 = CARTESIAN_POINT ( 'NONE',  ( 3.475237304863611154, 115.7029637511447646, -1.501298408546675178 ) ) ;
#38030 = CARTESIAN_POINT ( 'NONE',  ( 0.002455802209154075121, 120.8958299794632438, -0.1228983847502210514 ) ) ;
#38031 = CARTESIAN_POINT ( 'NONE',  ( 5.381753124113789255, -12.14417964010665330, 1.193960664996519094 ) ) ;
#38032 = CARTESIAN_POINT ( 'NONE',  ( -21.94752568715520979, 149.4141677464492091, 1.146579238551070468 ) ) ;
#38033 = CARTESIAN_POINT ( 'NONE',  ( -3.841520934845505941, 71.62889921741444255, -1.523999999999994026 ) ) ;
#38034 = CARTESIAN_POINT ( 'NONE',  ( 22.69169950426937987, 137.3157656003441787, 0.5971823736698287366 ) ) ;
#38035 = CARTESIAN_POINT ( 'NONE',  ( 15.26171895222979735, 148.0206345167940469, 0.3715023683812953004 ) ) ;
#38036 = DIRECTION ( 'NONE',  ( -1.000000000000000000, 0.000000000000000000, 0.000000000000000000 ) ) ;
#38037 = CARTESIAN_POINT ( 'NONE',  ( -0.4212773433310383342, 21.23346528477927819, -0.8800754956890687319 ) ) ;
#38038 = CARTESIAN_POINT ( 'NONE',  ( -5.748481425938979150, 159.1178304044242964, -0.1659167284945112786 ) ) ;
#38039 = CARTESIAN_POINT ( 'NONE',  ( -44.39753738666030358, 21.50835220694079197, -3.136200265191924075 ) ) ;
#38040 = EDGE_CURVE ( 'NONE', #20172, #11776, #27824, .T. ) ;
#38041 = DIRECTION ( 'NONE',  ( -0.8745520943968243532, 0.4849315768086547296, -5.361993529360573944E-16 ) ) ;
#38042 = ORIENTED_EDGE ( 'NONE', *, *, #14937, .F. ) ;
#38043 = CARTESIAN_POINT ( 'NONE',  ( -3.928350486978025469, 118.1770297339553366, 0.8034371862843084910 ) ) ;
#38044 = CARTESIAN_POINT ( 'NONE',  ( -17.31000046771894318, 62.32679794340116786, 1.269999999999999574 ) ) ;
#38045 = CARTESIAN_POINT ( 'NONE',  ( 21.76696383529558432, 149.6930991844618291, 2.018179159957718127 ) ) ;
#38046 = CARTESIAN_POINT ( 'NONE',  ( 20.20415560162845736, 149.0333503175929479, -1.664251383091793546 ) ) ;
#38047 = CARTESIAN_POINT ( 'NONE',  ( -1.997604609866625580, -12.39122764300357105, -4.168859717980781809 ) ) ;
#38048 = CARTESIAN_POINT ( 'NONE',  ( -17.34281104028706721, 125.1846915036903027, -1.498326104650645751 ) ) ;
#38049 = CARTESIAN_POINT ( 'NONE',  ( 4.818088273131546195, 117.7361865335809483, -0.8720296992808537206 ) ) ;
#38050 = EDGE_CURVE ( 'NONE', #25107, #17471, #22190, .T. ) ;
#38051 = CARTESIAN_POINT ( 'NONE',  ( 7.112984908206815504, 122.4243137415680280, 0.2517356677811186105 ) ) ;
#38052 = CARTESIAN_POINT ( 'NONE',  ( -1.582738162022960804, 156.2580631240469415, 0.1078144505905373474 ) ) ;
#38053 = CARTESIAN_POINT ( 'NONE',  ( -14.93497932922885596, 152.9649416503947634, -2.345758529409812443 ) ) ;
#38055 = CARTESIAN_POINT ( 'NONE',  ( 5.672040739448011237, -14.80640238898532601, 2.735881018706089129 ) ) ;
#38054 = CIRCLE ( 'NONE', #15573, 2.539999999999996483 ) ;
#38056 = VECTOR ( 'NONE', #4518, 1000.000000000000000 ) ;
#38057 = CARTESIAN_POINT ( 'NONE',  ( -6.515206564940426254E-14, 69.43546620154573645, -8.744632320494937509E-18 ) ) ;
#38058 = CARTESIAN_POINT ( 'NONE',  ( -43.82859865241511699, 24.63416949198730421, -1.524000000000007127 ) ) ;
#38059 = EDGE_CURVE ( 'NONE', #18509, #35273, #4683, .T. ) ;
#38060 = ORIENTED_EDGE ( 'NONE', *, *, #33646, .T. ) ;
#38061 = CARTESIAN_POINT ( 'NONE',  ( 5.834721624102704673, 119.7498067647950961, 1.158144809029191924 ) ) ;
#38062 = CARTESIAN_POINT ( 'NONE',  ( -6.566230858599542383E-14, 82.13546620154573930, -5.726718672203201028E-18 ) ) ;
#38063 = CARTESIAN_POINT ( 'NONE',  ( 1.406077420118782567E-15, 14.60500000000000220, 0.000000000000000000 ) ) ;
#38064 = CARTESIAN_POINT ( 'NONE',  ( -3.233068332335842676, 124.0549386377059307, -0.01378491165287840797 ) ) ;
#38065 = CARTESIAN_POINT ( 'NONE',  ( 8.407117359195193984, -5.923529430292941989, 0.7350785369227282873 ) ) ;
#38066 = CARTESIAN_POINT ( 'NONE',  ( 1.544162262333905522, 120.7289827521893670, 0.2751094044070052647 ) ) ;
#38067 = CARTESIAN_POINT ( 'NONE',  ( -4.726878620523991437, 118.5930653697794384, -1.020485165756037205 ) ) ;
#38068 = CARTESIAN_POINT ( 'NONE',  ( 13.22272649419657142, 119.7880570645780978, -0.3832108753485273245 ) ) ;
#38069 = EDGE_CURVE ( 'NONE', #29870, #22529, #14442, .T. ) ;
#38070 = FACE_OUTER_BOUND ( 'NONE', #30628, .T. ) ;
#38071 = CARTESIAN_POINT ( 'NONE',  ( -58.21877897856138873, 0.03104753578543094361, 0.5212065818953967034 ) ) ;
#38072 = CARTESIAN_POINT ( 'NONE',  ( 8.797993348169676153, 117.6946419546766833, 0.07291966862306284436 ) ) ;
#38073 = EDGE_CURVE ( 'NONE', #26298, #25879, #4543, .T. ) ;
#38074 = DIRECTION ( 'NONE',  ( -0.9998004120163610509, -4.016384292689131511E-17, -0.01997839162482749689 ) ) ;
#38076 = CARTESIAN_POINT ( 'NONE',  ( -5.450166374333774044, 56.51499999999997215, 4.451212169035321686 ) ) ;
#38075 = VECTOR ( 'NONE', #6316, 1000.000000000000114 ) ;
#38077 = CARTESIAN_POINT ( 'NONE',  ( -22.98488057257204886, 150.1591296352320910, -0.4592926148156235011 ) ) ;
#38078 = VERTEX_POINT ( 'NONE', #34275 ) ;
#38079 = CARTESIAN_POINT ( 'NONE',  ( -47.71508057896579658, 20.49549959222711593, 5.111566084959459744 ) ) ;
#38080 = AXIS2_PLACEMENT_3D ( 'NONE', #39997, #30797, #23560 ) ;
#38081 = CARTESIAN_POINT ( 'NONE',  ( 8.228572315554057326, 120.5845575724618186, -1.087623535237762784 ) ) ;
#38082 = CARTESIAN_POINT ( 'NONE',  ( -13.17422243436020857, 17.14500000000000668, 5.016499999999999737 ) ) ;
#38083 = CARTESIAN_POINT ( 'NONE',  ( -0.6895396258586810045, 156.3865044363621450, -0.6062415235663758395 ) ) ;
#38084 = DIRECTION ( 'NONE',  ( 0.9998004120163610509, 4.016384292689131511E-17, 0.01997839162482749689 ) ) ;
#38085 = DIRECTION ( 'NONE',  ( -0.8572391118119511155, -0.5149185422762101449, -3.573031421855331076E-16 ) ) ;
#38086 = EDGE_CURVE ( 'NONE', #25039, #6518, #5104, .T. ) ;
#38087 = ORIENTED_EDGE ( 'NONE', *, *, #22936, .T. ) ;
#38088 = CARTESIAN_POINT ( 'NONE',  ( 4.573446973487649281, 17.56025517495590904, -0.6989348988664985107 ) ) ;
#38089 = CARTESIAN_POINT ( 'NONE',  ( -5.285086173029821310, 105.1224018833269440, 0.7974957520148617807 ) ) ;
#38090 = CARTESIAN_POINT ( 'NONE',  ( -3.671158984043940170E-14, 57.78499999999999659, 0.000000000000000000 ) ) ;
#38091 = CARTESIAN_POINT ( 'NONE',  ( 7.213960532363571154, 78.77618639008812806, -1.904999999999999583 ) ) ;
#38092 = DIRECTION ( 'NONE',  ( -5.188838149069472160E-16, 1.699382548006136559E-16, 1.000000000000000000 ) ) ;
#38093 = CARTESIAN_POINT ( 'NONE',  ( -7.787533413562373497, 122.6196154471950024, -0.09973116279183735777 ) ) ;
#38094 = CARTESIAN_POINT ( 'NONE',  ( 4.518289034361447243, 23.24227448397437001, -0.9983406360900147769 ) ) ;
#38095 = CARTESIAN_POINT ( 'NONE',  ( 17.89857548597107950, 125.1504969321615164, 1.218861057454597052 ) ) ;
#38096 = CARTESIAN_POINT ( 'NONE',  ( -23.91048590848665611, 81.84235438443283783, -1.270000000000006235 ) ) ;
#38098 = CARTESIAN_POINT ( 'NONE',  ( 21.36781924117688192, 148.2102652567764380, -1.461444809879598017 ) ) ;
#38097 = CARTESIAN_POINT ( 'NONE',  ( 2.669030664778226480, -13.79969672238709499, -0.04828590215123814561 ) ) ;
#38099 = CARTESIAN_POINT ( 'NONE',  ( -7.441788261791943526, 120.6159063994810055, 0.9748553081951376598 ) ) ;
#38100 = CARTESIAN_POINT ( 'NONE',  ( -4.621022795674669226, 27.76579825817536218, 0.1735962381356405959 ) ) ;
#38101 = CARTESIAN_POINT ( 'NONE',  ( -7.798299699696711329, 158.6358315003295161, -0.8787250540639036656 ) ) ;
#38102 = CARTESIAN_POINT ( 'NONE',  ( -0.5824522774871869757, -3.319493544524417583, -0.7801697309090062094 ) ) ;
#38103 = ORIENTED_EDGE ( 'NONE', *, *, #5598, .F. ) ;
#38104 = CARTESIAN_POINT ( 'NONE',  ( -57.40070531792823516, 1.672101763895803117, 0.9705777051857996662 ) ) ;
#38105 = CARTESIAN_POINT ( 'NONE',  ( -11.48476400923512131, 128.2561452373498980, 0.2810130423614018436 ) ) ;
#38106 = CARTESIAN_POINT ( 'NONE',  ( 4.746351668907457189, -13.71804649124164222, 3.839566941389735977 ) ) ;
#38107 = CARTESIAN_POINT ( 'NONE',  ( 9.584070499013346733, 122.7780075402122151, -0.8664194973949995715 ) ) ;
#38108 = ORIENTED_EDGE ( 'NONE', *, *, #11578, .F. ) ;
#38109 = CARTESIAN_POINT ( 'NONE',  ( 3.160156207961041019, 115.7029629711633021, 1.658234469206849804 ) ) ;
#38110 = ORIENTED_EDGE ( 'NONE', *, *, #12017, .F. ) ;
#38111 = CARTESIAN_POINT ( 'NONE',  ( -4.861882094779772068, 117.7423377195431726, -0.9144347828526824262 ) ) ;
#38112 = ADVANCED_FACE ( 'NONE', ( #22084 ), #20824, .F. ) ;
#38113 = CARTESIAN_POINT ( 'NONE',  ( 10.40273896401435039, 153.1126597504080280, 0.1617772828476139180 ) ) ;
#38114 = AXIS2_PLACEMENT_3D ( 'NONE', #22573, #16621, #13228 ) ;
#38115 = VERTEX_POINT ( 'NONE', #38720 ) ;
#38116 = CARTESIAN_POINT ( 'NONE',  ( 4.978738709155149600, 118.8869175073591578, 1.099525347370199135 ) ) ;
#38117 = FACE_OUTER_BOUND ( 'NONE', #16187, .T. ) ;
#38118 = CARTESIAN_POINT ( 'NONE',  ( 4.801216665947148243, 117.4032681888235459, -1.015537427445656782 ) ) ;
#38119 = CARTESIAN_POINT ( 'NONE',  ( 0.003073183581685161574, 116.5806198863164838, -0.1537946732117060067 ) ) ;
#38120 = DIRECTION ( 'NONE',  ( 0.9998501190848634312, 0.01731298258488012456, 8.537024980200823790E-16 ) ) ;
#38121 = CARTESIAN_POINT ( 'NONE',  ( -11.97180806971945977, 56.20439414706015668, 5.016499999999999737 ) ) ;
#38122 = FACE_OUTER_BOUND ( 'NONE', #19081, .T. ) ;
#38123 = VECTOR ( 'NONE', #7721, 1000.000000000000000 ) ;
#38124 = CARTESIAN_POINT ( 'NONE',  ( 1.720531155625569797, -15.47675250719444939, 5.459092711723419811 ) ) ;
#38125 = CARTESIAN_POINT ( 'NONE',  ( -46.25688858429102623, 20.73875112231587892, 4.700046123029338219 ) ) ;
#38126 = CARTESIAN_POINT ( 'NONE',  ( 4.581716828367337513, -15.30239761468843973, -0.5121115983836379559 ) ) ;
#38127 = CARTESIAN_POINT ( 'NONE',  ( -4.745831499507636941, 117.9479565618830463, 0.6405143620768928292 ) ) ;
#38128 = ORIENTED_EDGE ( 'NONE', *, *, #8199, .F. ) ;
#38129 = ORIENTED_EDGE ( 'NONE', *, *, #37837, .T. ) ;
#38130 = CARTESIAN_POINT ( 'NONE',  ( 4.964802256754270893, 115.7029491485453150, -1.257203431686519712 ) ) ;
#38131 = EDGE_CURVE ( 'NONE', #15145, #24767, #8596, .T. ) ;
#38132 = CARTESIAN_POINT ( 'NONE',  ( 8.484504387306683881, 119.3307393024920202, -1.028660563731210731 ) ) ;
#38133 = CARTESIAN_POINT ( 'NONE',  ( -1.486515533886103801, 107.1743931308027129, -4.786382923486936392 ) ) ;
#38135 = CARTESIAN_POINT ( 'NONE',  ( 4.773560218005917122, 117.6391202506862044, 1.128671190400995616 ) ) ;
#38134 = CIRCLE ( 'NONE', #21780, 0.7620000000000000107 ) ;
#38136 = CARTESIAN_POINT ( 'NONE',  ( -46.60530155212502734, 26.17382724835478314, -1.397000000000007791 ) ) ;
#38137 = CARTESIAN_POINT ( 'NONE',  ( -0.4220321208937833357, 124.6436471961814050, 0.02396868521112080139 ) ) ;
#38138 = CARTESIAN_POINT ( 'NONE',  ( 4.560281875334545099, -11.68902278883368595, 0.6958564903332965512 ) ) ;
#38139 = EDGE_CURVE ( 'NONE', #6464, #40376, #16053, .T. ) ;
#38140 = CARTESIAN_POINT ( 'NONE',  ( -54.50298212578950796, 9.515077312548310573, 3.630897911711898018 ) ) ;
#38141 = DIRECTION ( 'NONE',  ( 5.188838149069472160E-16, -1.699382548006136559E-16, -1.000000000000000000 ) ) ;
#38142 = CARTESIAN_POINT ( 'NONE',  ( 3.722123463297008605, -13.62806973238828157, 3.608531954378976891 ) ) ;
#38143 = CARTESIAN_POINT ( 'NONE',  ( 4.933025141171929029, 117.5302216577071874, -0.6666291745611303554 ) ) ;
#38144 = CARTESIAN_POINT ( 'NONE',  ( -7.307041242074705956, 120.9764928074160082, -1.161154363956387492 ) ) ;
#38145 = CARTESIAN_POINT ( 'NONE',  ( -5.249547376985638891, 56.51499999999994373, 4.563748390655216980 ) ) ;
#38146 = CARTESIAN_POINT ( 'NONE',  ( -17.14500000000466784, 71.11999999999886768, 1.269999999999998241 ) ) ;
#38147 = CARTESIAN_POINT ( 'NONE',  ( -0.8976751760525136792, 115.7028555646716370, 1.718879955640483015 ) ) ;
#38148 = CARTESIAN_POINT ( 'NONE',  ( -0.8823465807374654135, 5.041073445128725794, 4.537322665494407659 ) ) ;
#38150 = EDGE_LOOP ( 'NONE', ( #35106, #17861, #17758, #28343 ) ) ;
#38149 = CARTESIAN_POINT ( 'NONE',  ( 6.903056240601945781, 117.3320596397172721, 0.5256612950045382870 ) ) ;
#38151 = CARTESIAN_POINT ( 'NONE',  ( 4.130052816961541140, 104.6144662015457811, -2.503261204555655706 ) ) ;
#38152 = CARTESIAN_POINT ( 'NONE',  ( 4.521904862512733381, -15.32733325190937990, -0.1948396341466702986 ) ) ;
#38153 = CARTESIAN_POINT ( 'NONE',  ( -6.185003182635424146, 157.2590385278250267, 1.713690555389224324 ) ) ;
#38154 = CARTESIAN_POINT ( 'NONE',  ( 0.05984739657028866761, 19.78266025878678391, 0.9748693421377304658 ) ) ;
#38155 = CARTESIAN_POINT ( 'NONE',  ( -0.4793318477812648082, 11.74037758575859058, -0.8492235504747065455 ) ) ;
#38156 = VERTEX_POINT ( 'NONE', #2945 ) ;
#38157 = ORIENTED_EDGE ( 'NONE', *, *, #30316, .F. ) ;
#38158 = CARTESIAN_POINT ( 'NONE',  ( -41.05189575270519242, 23.09451173561983239, -4.677211348804838536E-15 ) ) ;
#38159 = CARTESIAN_POINT ( 'NONE',  ( 5.704032853997349939, 123.8402959710505087, 0.1558735912124265544 ) ) ;
#38160 = FILL_AREA_STYLE ('',( #24728 ) ) ;
#38161 = CARTESIAN_POINT ( 'NONE',  ( -15.22619620759370918, 139.4722935914273307, 0.9828944228028649865 ) ) ;
#38162 = CYLINDRICAL_SURFACE ( 'NONE', #19800, 0.5080000000000000071 ) ;
#38163 = CARTESIAN_POINT ( 'NONE',  ( 3.475384634610537038, -12.95405113104661154, 1.817132104271814264 ) ) ;
#38164 = CARTESIAN_POINT ( 'NONE',  ( 14.06576283519498460, 128.5416456306063253, -1.400350009575090038 ) ) ;
#38165 = CARTESIAN_POINT ( 'NONE',  ( -20.12154232503860740, 149.0333503175929479, -2.470054797493931975 ) ) ;
#38166 = CARTESIAN_POINT ( 'NONE',  ( -5.639506490940112471, 64.42185452804264401, 1.270000000000004681 ) ) ;
#38167 = VECTOR ( 'NONE', #6723, 1000.000000000000000 ) ;
#38168 = CARTESIAN_POINT ( 'NONE',  ( 2.568134854143032442, -15.02010252187911554, 4.714990346623905815 ) ) ;
#38169 = CARTESIAN_POINT ( 'NONE',  ( 4.074910602682932925, 118.2429491485453354, -0.1454311599470142491 ) ) ;
#38170 = CARTESIAN_POINT ( 'NONE',  ( 15.87385217746171584, 146.2799285973741519, -0.1369075966739883299 ) ) ;
#38171 = VERTEX_POINT ( 'NONE', #9327 ) ;
#38172 = CARTESIAN_POINT ( 'NONE',  ( 2.664052010559913253, -13.52006206191685322, 0.08958796903007473778 ) ) ;
#38173 = DIRECTION ( 'NONE',  ( 5.188838149069472160E-16, -1.699382548006136559E-16, -1.000000000000000000 ) ) ;
#38174 = CIRCLE ( 'NONE', #39547, 3.683000000000001162 ) ;
#38175 = CARTESIAN_POINT ( 'NONE',  ( -10.92199999999999704, 12.96416000000000146, 0.000000000000000000 ) ) ;
#38176 = CARTESIAN_POINT ( 'NONE',  ( -47.85244527695893879, 19.39403540832956807, 5.219971639306655753 ) ) ;
#38177 = CARTESIAN_POINT ( 'NONE',  ( -8.365627035046871995, 27.56796056798338057, -1.282220400777004388 ) ) ;
#38178 = CARTESIAN_POINT ( 'NONE',  ( 8.539651237459528588, 154.7538831414287870, 1.439145765679522793 ) ) ;
#38179 = DIRECTION ( 'NONE',  ( -0.9998004120163609398, -4.016384292689130894E-17, -0.01997839162482749689 ) ) ;
#38180 = CARTESIAN_POINT ( 'NONE',  ( 21.67502463668045110, 132.7302833492884417, 0.4113505826877429938 ) ) ;
#38181 = CARTESIAN_POINT ( 'NONE',  ( -5.187812668267249627, 115.4810986995850755, 1.301936727496811663 ) ) ;
#38182 = CARTESIAN_POINT ( 'NONE',  ( 0.7336086519982951692, 0.2932837538699786251, -4.563195415240439701 ) ) ;
#38183 = CARTESIAN_POINT ( 'NONE',  ( 7.783246152616065672, 154.6561476914895081, 0.1555277812256516956 ) ) ;
#38184 = CARTESIAN_POINT ( 'NONE',  ( 5.585279946883024316, 5.098922668322787288, -6.300588543511215001 ) ) ;
#38185 = CARTESIAN_POINT ( 'NONE',  ( 2.159339310776008602, 116.5957718504302818, -0.3424589834756739393 ) ) ;
#38186 = CARTESIAN_POINT ( 'NONE',  ( -0.3562792453295428041, 120.3637084677653633, -0.5982640298941753754 ) ) ;
#38187 = FACE_OUTER_BOUND ( 'NONE', #10847, .T. ) ;
#38188 = CARTESIAN_POINT ( 'NONE',  ( 0.1058213901577000071, 105.9761915687834772, -5.295735085524063024 ) ) ;
#38189 = ADVANCED_BREP_SHAPE_REPRESENTATION ( '', ( #10787, #3275 ), #32513 ) ;
#38190 = CARTESIAN_POINT ( 'NONE',  ( 1.523114390242035210, -9.429190846093893796, -8.291516064885865234 ) ) ;
#38191 = EDGE_CURVE ( 'NONE', #915, #3540, #32322, .T. ) ;
#38192 = CARTESIAN_POINT ( 'NONE',  ( 3.159224709476080140, 117.3993812142055191, 1.388978621109378198 ) ) ;
#38193 = DIRECTION ( 'NONE',  ( -0.9998004120163609398, 0.000000000000000000, -0.01997839162482749342 ) ) ;
#38194 = CARTESIAN_POINT ( 'NONE',  ( -17.14500000000466784, 71.11999999999886768, -1.270000000000000684 ) ) ;
#38195 = CARTESIAN_POINT ( 'NONE',  ( 0.3929232564620411261, 123.1683257372383054, -0.1777898040562596038 ) ) ;
#38196 = CARTESIAN_POINT ( 'NONE',  ( -22.34885681094302967, 150.7328461917231550, 0.2743282927392731718 ) ) ;
#38197 = VERTEX_POINT ( 'NONE', #22289 ) ;
#38198 = CARTESIAN_POINT ( 'NONE',  ( -58.80872392184672037, -0.02106340533553074934, -0.1867271868312316840 ) ) ;
#38199 = ORIENTED_EDGE ( 'NONE', *, *, #18565, .F. ) ;
#38200 = DIRECTION ( 'NONE',  ( 0.8745520943968235761, -0.4849315768086558398, 0.000000000000000000 ) ) ;
#38202 = CARTESIAN_POINT ( 'NONE',  ( -10.14111963374837444, 125.9557236484601361, -0.1537744135814335389 ) ) ;
#38201 = CIRCLE ( 'NONE', #19808, 0.2539999999999956737 ) ;
#38203 = CARTESIAN_POINT ( 'NONE',  ( 3.960108094477612806, -15.52904141176333930, 4.900792037362536213 ) ) ;
#38204 = CARTESIAN_POINT ( 'NONE',  ( -20.05916364549921127, 149.8444905389382882, 1.617669260345511395 ) ) ;
#38205 = CARTESIAN_POINT ( 'NONE',  ( 0.02156508032615568615, 159.2730288250082538, -1.079204802879467406 ) ) ;
#38206 = CARTESIAN_POINT ( 'NONE',  ( 4.203610184846851894, 17.99761390031315500, -1.968029828111186319 ) ) ;
#38207 = CARTESIAN_POINT ( 'NONE',  ( -23.23349130944704299, 142.6711341654318801, -0.9216821775544485895 ) ) ;
#38208 = CARTESIAN_POINT ( 'NONE',  ( -57.72754330036800496, 1.649358777147267752, -1.624819368011742204 ) ) ;
#38209 = ORIENTED_EDGE ( 'NONE', *, *, #20410, .T. ) ;
#38210 = CARTESIAN_POINT ( 'NONE',  ( -0.09221630143976956850, 107.6766875080336376, 4.614880812453268533 ) ) ;
#38211 = DIRECTION ( 'NONE',  ( -5.206863593109713661E-17, 1.000000000000000000, -1.077750396879097183E-30 ) ) ;
#38212 = CARTESIAN_POINT ( 'NONE',  ( -17.22014391273219047, 144.2986879860016529, 1.480874425454277388 ) ) ;
#38213 = DIRECTION ( 'NONE',  ( 0.9998004120163609398, 0.000000000000000000, 0.01997839162482749689 ) ) ;
#38214 = CARTESIAN_POINT ( 'NONE',  ( 8.556073751109414260, 120.5511696877957775, -1.121754095281913388 ) ) ;
#38215 = AXIS2_PLACEMENT_3D ( 'NONE', #10091, #26275, #13075 ) ;
#38216 = CARTESIAN_POINT ( 'NONE',  ( -15.09010836182855186, 154.7927800759015042, -2.085168164864714235 ) ) ;
#38217 = CARTESIAN_POINT ( 'NONE',  ( -55.03109054507046238, 6.816801101491506643, -3.135084751894932076 ) ) ;
#38218 = CARTESIAN_POINT ( 'NONE',  ( 16.32790441640413093, 146.1553843108282820, -0.7912819366082538552 ) ) ;
#38219 = EDGE_LOOP ( 'NONE', ( #6976, #11308, #18384, #35146 ) ) ;
#38220 = CARTESIAN_POINT ( 'NONE',  ( -15.79265013068004109, 150.9007765090757971, -2.261858994468948225 ) ) ;
#38221 = CARTESIAN_POINT ( 'NONE',  ( 1.871808270187516943, -15.45276866356297418, 5.379583495939216142 ) ) ;
#38222 = CIRCLE ( 'NONE', #26651, 6.985000000000000320 ) ;
#38223 = CARTESIAN_POINT ( 'NONE',  ( -4.246385623344072435, 118.2248598242946827, -0.4674709900806769958 ) ) ;
#38224 = CIRCLE ( 'NONE', #21189, 0.5080000000000002292 ) ;
#38225 = CARTESIAN_POINT ( 'NONE',  ( -58.50860430493789721, 0.7049166599848305514, -0.9756837515128595761 ) ) ;
#38226 = CIRCLE ( 'NONE', #16340, 0.5080000000000002292 ) ;
#38227 = CARTESIAN_POINT ( 'NONE',  ( -4.784818766354882236, 117.7320628736595012, 0.8970813257759844284 ) ) ;
#38228 = CARTESIAN_POINT ( 'NONE',  ( 0.5205939700076258614, 119.6443647996702566, 0.5336935438815136878 ) ) ;
#38229 = CARTESIAN_POINT ( 'NONE',  ( -47.06702646257116385, 25.34112732371118781, 1.513569369951779597 ) ) ;
#38230 = CARTESIAN_POINT ( 'NONE',  ( 0.8402904295469701967, 0.2923264105788614398, -8.379105243356319122 ) ) ;
#38231 = CARTESIAN_POINT ( 'NONE',  ( 11.24781102592741355, 128.1602342495223468, 0.5025223919565851016 ) ) ;
#38232 = CARTESIAN_POINT ( 'NONE',  ( -48.28978369826177186, 19.63653578263564015, -5.206999999995405304 ) ) ;
#38234 = ORIENTED_EDGE ( 'NONE', *, *, #16267, .F. ) ;
#38233 = CARTESIAN_POINT ( 'NONE',  ( -41.05189575270517111, 23.09451173561986081, -1.397000000000004238 ) ) ;
#38235 = DIRECTION ( 'NONE',  ( 0.9998004120163610509, 4.016384292689131511E-17, 0.01997839162482749689 ) ) ;
#38236 = CARTESIAN_POINT ( 'NONE',  ( -57.71946847630993460, 1.146847591362354368, 1.351507486235933975 ) ) ;
#38237 = CARTESIAN_POINT ( 'NONE',  ( -53.84463291498614268, 9.545084226694347862, 3.785192793386291665 ) ) ;
#38238 = CARTESIAN_POINT ( 'NONE',  ( -7.785313187783981626, 122.6175865491890420, -0.2316613915245773481 ) ) ;
#38239 = CARTESIAN_POINT ( 'NONE',  ( -5.177913976931305839, 88.73331249999999670, -5.372100000000000541 ) ) ;
#38240 = CARTESIAN_POINT ( 'NONE',  ( -51.90232906080404263, 16.51944673254565643, 2.845700375512744795 ) ) ;
#38241 = CARTESIAN_POINT ( 'NONE',  ( -3.739900805225333524, 116.6566025657135413, 0.03821340562556417575 ) ) ;
#38242 = VERTEX_POINT ( 'NONE', #22498 ) ;
#38243 = CARTESIAN_POINT ( 'NONE',  ( -48.35471193741586404, 22.70554656608007704, -1.835820227619855416 ) ) ;
#38244 = CARTESIAN_POINT ( 'NONE',  ( 6.954509501169718000, 121.9349451668512927, -0.03177431777482942615 ) ) ;
#38245 = CARTESIAN_POINT ( 'NONE',  ( -8.438003980598709930, 119.5616927475976894, 1.071839762751747749 ) ) ;
#38246 = ORIENTED_EDGE ( 'NONE', *, *, #1749, .F. ) ;
#38247 = CARTESIAN_POINT ( 'NONE',  ( 2.441884256694776933, 115.7029470329614327, -1.605188886483090105 ) ) ;
#38248 = CARTESIAN_POINT ( 'NONE',  ( -0.6475778113726436969, 156.3069099058775748, -0.1429049811405684878 ) ) ;
#38249 = CARTESIAN_POINT ( 'NONE',  ( 4.090168366125579880, -14.63905918998462141, 5.005671547667302157 ) ) ;
#38250 = CARTESIAN_POINT ( 'NONE',  ( -0.02615207601228260181, 159.0391464308674756, 1.308756824028193488 ) ) ;
#38251 = CARTESIAN_POINT ( 'NONE',  ( -26.07365872405947727, 72.73903180058835005, -1.270000000000005791 ) ) ;
#38252 = VECTOR ( 'NONE', #34576, 1000.000000000000114 ) ;
#38253 = CARTESIAN_POINT ( 'NONE',  ( 18.60568445592635456, 154.1511370093759865, 0.5871577710369986214 ) ) ;
#38254 = CARTESIAN_POINT ( 'NONE',  ( 10.09730246939192178, 125.9371240743049611, 0.2994852486458426943 ) ) ;
#38255 = CARTESIAN_POINT ( 'NONE',  ( 1.248107678658480997E-15, 12.96416000000000146, 0.000000000000000000 ) ) ;
#38256 = CARTESIAN_POINT ( 'NONE',  ( 0.9048393610272945642, 9.142100508531621372, -0.3649321582425499311 ) ) ;
#38257 = CARTESIAN_POINT ( 'NONE',  ( 0.0007535234281849903688, 116.4338605912342786, -0.03770939363766603186 ) ) ;
#38258 = DIRECTION ( 'NONE',  ( -0.8745520943968235761, 0.4849315768086558398, 0.000000000000000000 ) ) ;
#38259 = DIRECTION ( 'NONE',  ( -0.6559537821943243197, 0.7548010569845282625, -8.537024980200743918E-16 ) ) ;
#38260 = VERTEX_POINT ( 'NONE', #15909 ) ;
#38261 = CARTESIAN_POINT ( 'NONE',  ( -2.285527320723312439, 116.3691792070813733, 0.1865855086054521439 ) ) ;
#38262 = CARTESIAN_POINT ( 'NONE',  ( -23.75665686005077859, 76.91945007112674659, 1.269999999999994245 ) ) ;
#38263 = CARTESIAN_POINT ( 'NONE',  ( 1.109551233970408335, 117.7697124030934077, 0.5969493375118323231 ) ) ;
#38264 = CARTESIAN_POINT ( 'NONE',  ( 0.01111639779256734344, 118.2594330468507593, -0.5563100024230162033 ) ) ;
#38265 = CARTESIAN_POINT ( 'NONE',  ( -6.300109353874518980, 26.68925120273002705, -5.586516568188822696 ) ) ;
#38266 = CARTESIAN_POINT ( 'NONE',  ( -15.04114430247513035, 121.6710330000183546, -1.338242383117114853 ) ) ;
#38267 = CARTESIAN_POINT ( 'NONE',  ( 4.839331864970178643, 117.8306479882070050, -0.7070860029426544457 ) ) ;
#38268 = CARTESIAN_POINT ( 'NONE',  ( 5.328278062782956681, 116.9387654363850260, 0.9571818161585843310 ) ) ;
#38269 = AXIS2_PLACEMENT_3D ( 'NONE', #12801, #34991, #24961 ) ;
#38270 = CARTESIAN_POINT ( 'NONE',  ( -15.28485850284635283, 148.0141687878753203, -0.07717638215565292281 ) ) ;
#38271 = CARTESIAN_POINT ( 'NONE',  ( -17.07725563869816199, 135.3907879583883869, -2.389267674572352451 ) ) ;
#38272 = CARTESIAN_POINT ( 'NONE',  ( 3.960108094477612806, -15.52904141176333930, 4.900792037362536213 ) ) ;
#38273 = DIRECTION ( 'NONE',  ( 1.000000000000000000, -1.288607544181256449E-16, 0.000000000000000000 ) ) ;
#38274 = CARTESIAN_POINT ( 'NONE',  ( -4.771503349878651434, 117.9496054766768225, -1.116523703797990263 ) ) ;
#38275 = EDGE_LOOP ( 'NONE', ( #29572, #18196, #8735, #22321 ) ) ;
#38276 = CARTESIAN_POINT ( 'NONE',  ( 8.000928410381797917, 156.3870133935118076, 2.044342179695390893 ) ) ;
#38277 = DIRECTION ( 'NONE',  ( 4.017660918040594346E-17, -1.000000000000000000, -2.376309959284834438E-19 ) ) ;
#38278 = DIRECTION ( 'NONE',  ( -0.9998004120163608288, 0.000000000000000000, -0.01997839162482749342 ) ) ;
#38279 = AXIS2_PLACEMENT_3D ( 'NONE', #16157, #38556, #29379 ) ;
#38280 = CARTESIAN_POINT ( 'NONE',  ( -1.397093717039429972, 113.6455945353133643, 2.337579097500038561 ) ) ;
#38281 = CARTESIAN_POINT ( 'NONE',  ( -8.384998746481384657, -10.44493509673469767, 0.7792886224267949746 ) ) ;
#38282 = CARTESIAN_POINT ( 'NONE',  ( 1.678671165333015747, 156.3322054215483092, 0.6622483832023354777 ) ) ;
#38283 = CARTESIAN_POINT ( 'NONE',  ( 15.09612904044924697, 120.9194639129320734, -0.3833380168901105445 ) ) ;
#38284 = CARTESIAN_POINT ( 'NONE',  ( 5.941750549330224729, 56.51500000000122270, -5.016499812856827667 ) ) ;
#38285 = CARTESIAN_POINT ( 'NONE',  ( -58.35332038481796957, -0.2570561626924458554, 0.1612409511329637168 ) ) ;
#38286 = CARTESIAN_POINT ( 'NONE',  ( 8.798547045555515922, 117.6874503704031127, 0.1190114001730665366 ) ) ;
#38287 = EDGE_CURVE ( 'NONE', #3139, #7830, #18819, .T. ) ;
#38288 = CARTESIAN_POINT ( 'NONE',  ( -5.223971174379743232, 56.51499999999997215, 4.542495777410084479 ) ) ;
#38289 = CIRCLE ( 'NONE', #6332, 5.334000000000001407 ) ;
#38290 = CARTESIAN_POINT ( 'NONE',  ( -22.66375647020928952, 150.6386093215955100, -0.4528757910175258972 ) ) ;
#38291 = ORIENTED_EDGE ( 'NONE', *, *, #20565, .T. ) ;
#38292 = CARTESIAN_POINT ( 'NONE',  ( -6.379245509003030890, 120.1349722450784725, -1.192449620425102941 ) ) ;
#38293 = CARTESIAN_POINT ( 'NONE',  ( 5.336610043934060243, 104.6144662015457527, -0.07732958313162717479 ) ) ;
#38294 = CARTESIAN_POINT ( 'NONE',  ( -8.816380758798688433, 123.2701452714374568, -0.6637701367642925288 ) ) ;
#38295 = CARTESIAN_POINT ( 'NONE',  ( -28.96638701358144985, 63.08302880246334610, 1.523999999999992916 ) ) ;
#38296 = CARTESIAN_POINT ( 'NONE',  ( 22.53492722140441629, 150.7843406352268687, 0.4757920170715053132 ) ) ;
#38297 = EDGE_LOOP ( 'NONE', ( #33423, #32562, #31214, #13628 ) ) ;
#38298 = CARTESIAN_POINT ( 'NONE',  ( -3.158589313471108273, 4.191505055319898254, 3.400481138232230194 ) ) ;
#38299 = CARTESIAN_POINT ( 'NONE',  ( -29.30242189345354831, 66.59148765006932535, 1.524000000000569344 ) ) ;
#38300 = CARTESIAN_POINT ( 'NONE',  ( -1.421603664355800101, 159.6054662015457666, -0.02840702444251828190 ) ) ;
#38301 = CARTESIAN_POINT ( 'NONE',  ( -17.14500000000466784, 71.11999999999886768, -1.524000000000000909 ) ) ;
#38302 = CARTESIAN_POINT ( 'NONE',  ( -36.65473259702432784, 28.27472347546385123, -1.270000000000003570 ) ) ;
#38303 = CARTESIAN_POINT ( 'NONE',  ( -6.064067160211926932, 121.4300801654758146, 0.02073022162667565588 ) ) ;
#38304 = CARTESIAN_POINT ( 'NONE',  ( 1.677595020332960152, 24.74158224480939339, -4.309653081027373211 ) ) ;
#38305 = CARTESIAN_POINT ( 'NONE',  ( 9.554367121731589307, 118.3624989119526418, 0.8896461348445369177 ) ) ;
#38306 = DIRECTION ( 'NONE',  ( 1.000000000000000000, 0.000000000000000000, 0.000000000000000000 ) ) ;
#38308 = CARTESIAN_POINT ( 'NONE',  ( 4.024684254631489821, 117.9114980025989752, -0.7134393008021913118 ) ) ;
#38307 = CARTESIAN_POINT ( 'NONE',  ( 5.322370863981891631, 57.14999999999997726, 5.239063870260719291 ) ) ;
#38309 =( GEOMETRIC_REPRESENTATION_CONTEXT ( 3 ) GLOBAL_UNCERTAINTY_ASSIGNED_CONTEXT ( ( #3137 ) ) GLOBAL_UNIT_ASSIGNED_CONTEXT ( ( #37495, #35990, #6389 ) ) REPRESENTATION_CONTEXT ( 'NONE', 'WORKASPACE' ) );
#38310 = CARTESIAN_POINT ( 'NONE',  ( -11.32523555543272487, 123.0403929720162495, 1.197004354367268153 ) ) ;
#38311 = CARTESIAN_POINT ( 'NONE',  ( -4.384008014420753163, 17.61986127277741332, -1.463615122064717111 ) ) ;
#38312 = CARTESIAN_POINT ( 'NONE',  ( -3.843811238687901533, 117.0275016673472663, -0.5328274117395519482 ) ) ;
#38313 = AXIS2_PLACEMENT_3D ( 'NONE', #38773, #29171, #229 ) ;
#38314 = B_SPLINE_CURVE_WITH_KNOTS ( 'NONE', 3,
 ( #30772, #2458, #21583, #17984, #27582, #34611, #24168, #40590, #38013, #30981, #1821, #8835, #14785, #40797, #34825, #11597, #37586, #32672, #9258, #35451, #16044, #2875, #22631, #28630, #9870, #31830, #38232 ),
 .UNSPECIFIED., .F., .F.,
 ( 4, 1, 1, 1, 1, 1, 1, 1, 1, 1, 1, 1, 1, 1, 1, 1, 1, 1, 1, 1, 1, 1, 1, 1, 4 ),
 ( 0.000000000000000000, 0.02298233349012935092, 0.04596466698025847980, 0.05745583372532304944, 0.06894700047038783419, 0.08043816721545261894, 0.09192933396051740369, 0.1034205007055817582, 0.1149116674506463209, 0.1264028341957113277, 0.1378940009407758904, 0.1838586679210341412, 0.2298233349012926419, 0.2757880018815508927, 0.3217526688618093655, 0.3677173358420680049, 0.4136820028223265333, 0.4596466698025850617, 0.5056113367828434235, 0.5515760037631017854, 0.5975406707433603692, 0.6435053377236188421, 0.6664876712137480785, 0.6894700047038772039, 0.7354344192538664338 ),
 .UNSPECIFIED. ) ;
#38315 = CARTESIAN_POINT ( 'NONE',  ( -0.8659212883131867100, -1.167510040683709560, 0.4517697218592801600 ) ) ;
#38316 = ORIENTED_EDGE ( 'NONE', *, *, #38000, .F. ) ;
#38317 = CARTESIAN_POINT ( 'NONE',  ( -54.95604735203036029, 6.474113128985478305, 1.942216106931671904 ) ) ;
#38318 = CARTESIAN_POINT ( 'NONE',  ( -7.078188358610653985, 121.9740017686541194, 0.1969649471280498776 ) ) ;
#38319 = CARTESIAN_POINT ( 'NONE',  ( 5.778079093609060024, -12.78747091716041240, 1.651671850763037463 ) ) ;
#38320 = CARTESIAN_POINT ( 'NONE',  ( 12.96210878518737708, 128.4900567078429390, -1.108396809849303777 ) ) ;
#38321 = DIRECTION ( 'NONE',  ( 0.4849315768086535638, 0.8745520943968251304, 2.742148322653192551E-14 ) ) ;
#38322 = AXIS2_PLACEMENT_3D ( 'NONE', #33207, #17829, #33627 ) ;
#38323 = CARTESIAN_POINT ( 'NONE',  ( -4.903208392033640450, 117.6536421438997451, -0.9409563386690815712 ) ) ;
#38324 = EDGE_CURVE ( 'NONE', #36953, #4283, #31727, .T. ) ;
#38325 = CARTESIAN_POINT ( 'NONE',  ( 0.0005468344958423734022, 156.3034662015456604, -0.02736583427618467443 ) ) ;
#38326 = VERTEX_POINT ( 'NONE', #5937 ) ;
#38327 = CARTESIAN_POINT ( 'NONE',  ( 17.65052098649041667, 151.6044147853587845, 2.418251502674879649 ) ) ;
#38328 = DIRECTION ( 'NONE',  ( -0.9998004120163609398, 0.000000000000000000, -0.01997839162482749689 ) ) ;
#38329 = DIRECTION ( 'NONE',  ( -0.9998004120163608288, 0.000000000000000000, -0.01997839162482749342 ) ) ;
#38330 = CARTESIAN_POINT ( 'NONE',  ( -9.712308604790296229, 65.53852105402241079, -1.523999999999996025 ) ) ;
#38331 = CARTESIAN_POINT ( 'NONE',  ( 23.32076472591247196, 148.8446908248229477, 0.1342014517686429820 ) ) ;
#38332 = CARTESIAN_POINT ( 'NONE',  ( 0.07157677169882613322, 110.3683645023726569, -3.581994345755985076 ) ) ;
#38333 = CIRCLE ( 'NONE', #14509, 0.2539999999999937863 ) ;
#38334 = CARTESIAN_POINT ( 'NONE',  ( -46.85748110696954427, 25.55033861525921779, 1.599144941528299224 ) ) ;
#38335 = CARTESIAN_POINT ( 'NONE',  ( -47.31580374228550312, 25.16323110364244897, 0.6294670755810632956 ) ) ;
#38336 = CARTESIAN_POINT ( 'NONE',  ( 1.736649427362045861, -15.40716104390517316, 5.430039758140377870 ) ) ;
#38337 = CARTESIAN_POINT ( 'NONE',  ( -47.87216941255763203, 19.82042534259524658, 5.426529464407925829 ) ) ;
#38338 = FACE_OUTER_BOUND ( 'NONE', #5363, .T. ) ;
#38339 = ADVANCED_FACE ( 'NONE', ( #18897 ), #31906, .F. ) ;
#38340 = TOROIDAL_SURFACE ( 'NONE', #19963, 5.080000000000005400, 0.5080000000000000071 ) ;
#38341 = CARTESIAN_POINT ( 'NONE',  ( -4.575171740070761217, 118.0742775853333768, 0.6029512648002022246 ) ) ;
#38342 = VERTEX_POINT ( 'NONE', #6347 ) ;
#38343 = DIRECTION ( 'NONE',  ( -0.8138664877804109299, -0.5810519254489895369, 0.000000000000000000 ) ) ;
#38344 = CARTESIAN_POINT ( 'NONE',  ( -5.913856609602897940, 119.1282656376870364, -1.263485629223820794 ) ) ;
#38345 = CARTESIAN_POINT ( 'NONE',  ( -5.397835693418398861, 119.2618716387835747, -0.5632668535983702540 ) ) ;
#38346 = CARTESIAN_POINT ( 'NONE',  ( 4.625168964342468492, 117.9841153801070561, 0.8982682689321210834 ) ) ;
#38347 = CARTESIAN_POINT ( 'NONE',  ( 2.857130780617909149, -14.87311083204414786, 4.269097905712053276 ) ) ;
#38348 = CARTESIAN_POINT ( 'NONE',  ( -0.3869134157277939190, 116.4813942609866899, 1.514588684444738709 ) ) ;
#38349 = TOROIDAL_SURFACE ( 'NONE', #19967, 0.7620000000000000107, 0.2540000000000000036 ) ;
#38350 = SURFACE_SIDE_STYLE ('',( #34950 ) ) ;
#38351 = LINE ( 'NONE', #29160, #5409 ) ;
#38352 = LINE ( 'NONE', #24708, #24631 ) ;
#38353 = CARTESIAN_POINT ( 'NONE',  ( 6.476067766296546679, 120.6581566633936404, -0.1355830077277814794 ) ) ;
#38354 = CARTESIAN_POINT ( 'NONE',  ( -10.68802918394767687, 123.5542795626547417, -1.432819001183019969 ) ) ;
#38355 = EDGE_CURVE ( 'NONE', #3641, #19292, #3054, .T. ) ;
#38356 = CARTESIAN_POINT ( 'NONE',  ( 16.18905205736044906, 121.2598130428683447, 0.3234957879086921562 ) ) ;
#38357 = CARTESIAN_POINT ( 'NONE',  ( -6.003866115224264277, 28.47055935836900176, 0.6261310066654243167 ) ) ;
#38358 = CARTESIAN_POINT ( 'NONE',  ( -3.961103147347932119, 115.7035856650175418, 1.436382292835700625 ) ) ;
#38359 = CARTESIAN_POINT ( 'NONE',  ( 4.364008504204949013, 7.202613900313124873, 1.580794030135405537 ) ) ;
#38361 = VERTEX_POINT ( 'NONE', #25085 ) ;
#38360 = CARTESIAN_POINT ( 'NONE',  ( 15.70934801585141116, 121.2535323456646523, 0.8362899507430230361 ) ) ;
#38362 = CARTESIAN_POINT ( 'NONE',  ( 0.9340703678216289996, 104.6144662015456674, -5.263168525813664900 ) ) ;
#38363 = AXIS2_PLACEMENT_3D ( 'NONE', #19806, #3653, #16620 ) ;
#38364 = CARTESIAN_POINT ( 'NONE',  ( 2.947576629936649706, -15.31278845794613375, 4.223034005107467515 ) ) ;
#38365 = CARTESIAN_POINT ( 'NONE',  ( -0.03256023585726924852, 157.9544661776888290, 1.629447346748784664 ) ) ;
#38366 = CARTESIAN_POINT ( 'NONE',  ( -0.8940008744714061928, 26.26452439613007428, -0.3861867617640990513 ) ) ;
#38367 = CARTESIAN_POINT ( 'NONE',  ( -0.8857237343455648393, 3.096269703755229141, -0.4102451188256627801 ) ) ;
#38368 = ORIENTED_EDGE ( 'NONE', *, *, #9517, .T. ) ;
#38369 = ORIENTED_EDGE ( 'NONE', *, *, #27356, .T. ) ;
#38370 = DIRECTION ( 'NONE',  ( -0.9998004120163608288, -4.016384292689131511E-17, -0.01997839162482749342 ) ) ;
#38371 = CARTESIAN_POINT ( 'NONE',  ( 3.281580062219306093, 118.9685052735122355, 0.6847577310700790898 ) ) ;
#38372 =( NAMED_UNIT ( * ) SI_UNIT ( $, .STERADIAN. ) SOLID_ANGLE_UNIT ( ) );
#38373 = CARTESIAN_POINT ( 'NONE',  ( -5.197063283114393251, 120.9449653624321144, 0.4048198106261542417 ) ) ;
#38374 = CARTESIAN_POINT ( 'NONE',  ( -15.21351360038775802, 143.4186079242255119, -0.3040022078858783949 ) ) ;
#38375 = CARTESIAN_POINT ( 'NONE',  ( 3.260250311156894121, -12.89034478651954174, 1.323980178024680043 ) ) ;
#38376 = CARTESIAN_POINT ( 'NONE',  ( 2.123774309200863630, 157.0334531201187644, -1.456117127909798192 ) ) ;
#38377 = CIRCLE ( 'NONE', #34975, 0.2539999999999973390 ) ;
#38378 = CARTESIAN_POINT ( 'NONE',  ( -20.22999339756081838, 148.7458375694471044, -2.474301912364147871 ) ) ;
#38379 = CARTESIAN_POINT ( 'NONE',  ( -41.05189575270516400, 23.09451173561988213, -0.7620000000000052287 ) ) ;
#38380 = CARTESIAN_POINT ( 'NONE',  ( 8.631261618837783089, 118.4117623764986007, 1.057671270618954829 ) ) ;
#38381 = CARTESIAN_POINT ( 'NONE',  ( -3.044072069279135206, 34.44269722464345307, 3.574075509920750626 ) ) ;
#38382 = EDGE_CURVE ( 'NONE', #6660, #21896, #42136, .T. ) ;
#38383 = CARTESIAN_POINT ( 'NONE',  ( 8.625872078176229252, 123.3364012560002578, -0.04702935286775003498 ) ) ;
#38384 = ORIENTED_EDGE ( 'NONE', *, *, #5633, .F. ) ;
#38385 = CARTESIAN_POINT ( 'NONE',  ( 0.1058213901578615862, 105.9761915687788729, -5.295735085525930863 ) ) ;
#38386 = EDGE_CURVE ( 'NONE', #5419, #22830, #19317, .T. ) ;
#38387 = CARTESIAN_POINT ( 'NONE',  ( 4.867434175510519268, 117.7629967458994287, 0.8046164465094345353 ) ) ;
#38388 = EDGE_CURVE ( 'NONE', #120, #30637, #28240, .T. ) ;
#38389 = CARTESIAN_POINT ( 'NONE',  ( -13.34597544948414161, 17.14500000000000313, 5.016499999999998849 ) ) ;
#38390 = CARTESIAN_POINT ( 'NONE',  ( -7.817010796087602742, 17.61996943312679775, -3.135079784279759085 ) ) ;
#38391 = CARTESIAN_POINT ( 'NONE',  ( 15.81386139960065051, 149.2064892436030163, 1.885719434888957879 ) ) ;
#38392 = PLANE ( 'NONE',  #40998 ) ;
#38393 = CARTESIAN_POINT ( 'NONE',  ( 20.69945920510660997, 152.5542719854981044, 0.3887601451951304132 ) ) ;
#38394 = CARTESIAN_POINT ( 'NONE',  ( -2.162697817503842934, 106.7001829816230725, 4.879784414745867771 ) ) ;
#38395 = AXIS2_PLACEMENT_3D ( 'NONE', #32187, #26417, #19799 ) ;
#38396 = B_SPLINE_CURVE_WITH_KNOTS ( 'NONE', 3,
 ( #6352, #6986, #39357, #9745, #16119, #12936, #22502, #182, #26144, #13362, #10161, #35532 ),
 .UNSPECIFIED., .F., .F.,
 ( 4, 1, 1, 1, 1, 1, 1, 1, 1, 4 ),
 ( 0.5426758968252777260, 0.5876249999999998419, 0.6700999999999999179, 0.7525749999999999940, 0.7938125000000000320, 0.8350499999999998479, 0.8762874999999994419, 0.9175249999999994799, 0.9587624999999999620, 0.9957666935384927864 ),
 .UNSPECIFIED. ) ;
#38397 = PLANE ( 'NONE',  #23037 ) ;
#38398 = CARTESIAN_POINT ( 'NONE',  ( 1.562757238090025202, 156.2577446057484281, 0.06075558507430143390 ) ) ;
#38399 = CARTESIAN_POINT ( 'NONE',  ( 11.89465070410498093, 120.7721054874162974, 1.583610710261881049 ) ) ;
#38400 = CARTESIAN_POINT ( 'NONE',  ( -5.729511908840139611, -2.247816343263548511, -6.181412921048518250 ) ) ;
#38401 = CARTESIAN_POINT ( 'NONE',  ( 5.511179323772147143, 117.2417087625145626, -0.6038106809302513645 ) ) ;
#38402 = CARTESIAN_POINT ( 'NONE',  ( -0.3561418115365337367, 119.9741034315941732, -0.6738560125758273900 ) ) ;
#38403 = TOROIDAL_SURFACE ( 'NONE', #310, 0.3809999999999995057, 0.2540000000000000036 ) ;
#38404 = LINE ( 'NONE', #18991, #32549 ) ;
#38405 = CARTESIAN_POINT ( 'NONE',  ( 2.306944209869228768, 107.0587059723494860, -4.722744024792687512 ) ) ;
#38406 = CARTESIAN_POINT ( 'NONE',  ( -4.212901951478492890, -8.356617434558033963, -7.328762184035659821 ) ) ;
#38407 = CARTESIAN_POINT ( 'NONE',  ( 0.7953399164170903424, 117.3993835805238035, 1.485889010799970489 ) ) ;
#38408 = CARTESIAN_POINT ( 'NONE',  ( -4.854186777038641765, 117.7557277303023966, -0.9091791526384296329 ) ) ;
#38409 = CARTESIAN_POINT ( 'NONE',  ( 2.827333099181600584, -13.37427733298611443, 0.6166582517569209054 ) ) ;
#38410 = CARTESIAN_POINT ( 'NONE',  ( 0.1065646865914870178, 105.8844662015456919, -5.332932678536313809 ) ) ;
#38411 = CARTESIAN_POINT ( 'NONE',  ( -15.19762206999210186, 120.8830733721255370, 0.2994679608661980907 ) ) ;
#38412 = ORIENTED_EDGE ( 'NONE', *, *, #830, .F. ) ;
#38413 = CARTESIAN_POINT ( 'NONE',  ( 6.059261036834384662, 77.01756249999996840, 5.016499999999999737 ) ) ;
#38414 = ORIENTED_EDGE ( 'NONE', *, *, #10530, .T. ) ;
#38415 = CARTESIAN_POINT ( 'NONE',  ( -42.66890350025449408, 21.80565315997039733, -1.797223148892109545 ) ) ;
#38416 = CARTESIAN_POINT ( 'NONE',  ( 2.105506875138051459, -15.57594099408041188, 5.887502213194136580 ) ) ;
#38417 = CARTESIAN_POINT ( 'NONE',  ( -6.741874166124567580, 157.8130281244853279, 1.606654124060122424 ) ) ;
#38418 = CARTESIAN_POINT ( 'NONE',  ( 5.873718653373081189, 117.7475948868982698, -0.6546600694323944092 ) ) ;
#38419 = CARTESIAN_POINT ( 'NONE',  ( 4.326043401919948295, 8.289558097378858292, -1.648119079657388353 ) ) ;
#38420 = CARTESIAN_POINT ( 'NONE',  ( -54.46595390896940359, 8.352818827531990564, -3.537195888581306402 ) ) ;
#38421 = EDGE_CURVE ( 'NONE', #22644, #32069, #15303, .T. ) ;
#38422 = VERTEX_POINT ( 'NONE', #21022 ) ;
#38423 = CARTESIAN_POINT ( 'NONE',  ( -0.005099097581101574329, 122.5569158606516993, 0.2551796940110860890 ) ) ;
#38424 = DIRECTION ( 'NONE',  ( 0.9998004120163609398, 4.016384292689130894E-17, 0.01997839162482749689 ) ) ;
#38425 = CARTESIAN_POINT ( 'NONE',  ( -12.26974321764567932, 126.0625018263836807, 1.123002009909297660 ) ) ;
#38426 = DIRECTION ( 'NONE',  ( -1.000000000000000000, -9.933992704233682996E-16, 0.000000000000000000 ) ) ;
#38427 = CARTESIAN_POINT ( 'NONE',  ( 8.076210525097339499, 156.3870133935118076, -1.723082682300313806 ) ) ;
#38428 = CARTESIAN_POINT ( 'NONE',  ( -20.60480707444014570, 141.5323519391372997, -2.354057365763566168 ) ) ;
#38429 = CARTESIAN_POINT ( 'NONE',  ( -51.09990735641632398, 14.52648110433587370, -4.713018929684125169 ) ) ;
#38430 = CARTESIAN_POINT ( 'NONE',  ( 8.149220328376060252, 154.6259123219959690, -0.6607633090041662438 ) ) ;
#38431 = ORIENTED_EDGE ( 'NONE', *, *, #14841, .T. ) ;
#38432 = CARTESIAN_POINT ( 'NONE',  ( -17.44789039799423591, 148.6234142586927476, -2.276312578826294342 ) ) ;
#38433 = CARTESIAN_POINT ( 'NONE',  ( 3.716361853963529249, -15.42594482578084403, 2.788391211141477921 ) ) ;
#38434 = CARTESIAN_POINT ( 'NONE',  ( -4.229144778596610976, 118.2245657482411474, -0.4851207049587970555 ) ) ;
#38435 = ADVANCED_FACE ( 'NONE', ( #2087 ), #41061, .F. ) ;
#38436 = DIRECTION ( 'NONE',  ( -1.000000000000000000, 0.000000000000000000, 0.000000000000000000 ) ) ;
#38437 = EDGE_CURVE ( 'NONE', #38156, #450, #30273, .T. ) ;
#38438 = CARTESIAN_POINT ( 'NONE',  ( -4.937121216058332429, 117.6323291441971861, 0.7898849711784506900 ) ) ;
#38439 = CARTESIAN_POINT ( 'NONE',  ( 14.65736332902321060, 131.2156652454908112, 2.020252246219832681 ) ) ;
#38440 = CARTESIAN_POINT ( 'NONE',  ( -46.81030548986588968, 25.80411194895121341, 1.573461678943545161 ) ) ;
#38441 = CARTESIAN_POINT ( 'NONE',  ( 6.518667233416390872, -10.50300228728784901, -5.332001816399940530 ) ) ;
#38442 = CARTESIAN_POINT ( 'NONE',  ( 3.721623402434252714, 121.0563512343167645, 0.1807651092205457555 ) ) ;
#38443 = CARTESIAN_POINT ( 'NONE',  ( -6.096037513970406607, 78.08166987308820239, 1.270000000000003126 ) ) ;
#38444 = CARTESIAN_POINT ( 'NONE',  ( -48.50421218116022004, 14.67712143704007133, -0.4105607596418053284 ) ) ;
#38445 = CARTESIAN_POINT ( 'NONE',  ( -16.60960244842765832, 17.14499999999999957, 0.000000000000000000 ) ) ;
#38446 = CARTESIAN_POINT ( 'NONE',  ( -57.80205714066466527, 2.371715784325115095, 1.753227392946289598 ) ) ;
#38447 = CARTESIAN_POINT ( 'NONE',  ( -52.49023018389913631, 12.05517075480290679, 4.265271142760512113 ) ) ;
#38448 = DIRECTION ( 'NONE',  ( 0.1469470846586743706, 0.000000000000000000, -0.9891443546370348727 ) ) ;
#38449 = CARTESIAN_POINT ( 'NONE',  ( -5.664977208693910526, 77.01756249999996840, -5.033228321271210781 ) ) ;
#38450 = CARTESIAN_POINT ( 'NONE',  ( -57.66243511465493299, 3.255537196535568611, -1.046671340306231880E-14 ) ) ;
#38451 = CARTESIAN_POINT ( 'NONE',  ( -23.17968947452053996, 149.6103952014060212, -0.1325215592567119405 ) ) ;
#38452 = ORIENTED_EDGE ( 'NONE', *, *, #36077, .F. ) ;
#38453 = CARTESIAN_POINT ( 'NONE',  ( -50.95401362087786623, 21.69085173448186055, -0.3723302588259480572 ) ) ;
#38454 = CARTESIAN_POINT ( 'NONE',  ( -5.981523321826031747, 121.4283444620903367, -0.2204012826164671313 ) ) ;
#38455 = CARTESIAN_POINT ( 'NONE',  ( 4.828520450080895365, 117.4049894591484673, -1.009733177510003799 ) ) ;
#38456 = ORIENTED_EDGE ( 'NONE', *, *, #16476, .F. ) ;
#38457 = CARTESIAN_POINT ( 'NONE',  ( 0.9904753432905314403, 115.7029491485453008, -1.712273171734945976 ) ) ;
#38458 = CARTESIAN_POINT ( 'NONE',  ( -9.115443861534034298, 124.0847320388339625, -0.2671161660598813103 ) ) ;
#38459 = CARTESIAN_POINT ( 'NONE',  ( 4.834931622272050866, -13.60668467239417545, 3.655623996717635382 ) ) ;
#38460 = CARTESIAN_POINT ( 'NONE',  ( -1.113991634874509806, 117.6437429425539420, 0.5281592773360505033 ) ) ;
#38461 = DIRECTION ( 'NONE',  ( -5.188838149069471174E-16, 1.699382548006136313E-16, 1.000000000000000000 ) ) ;
#38462 = CARTESIAN_POINT ( 'NONE',  ( 23.08789804466225704, 149.8924475812327159, 0.6911741358207285080 ) ) ;
#38463 = CARTESIAN_POINT ( 'NONE',  ( 5.334492475561027902, 121.3506618966597728, 0.2156469154756605611 ) ) ;
#38464 = CARTESIAN_POINT ( 'NONE',  ( 7.213960532367366341, 78.77618639008778700, 1.904999999999999583 ) ) ;
#38465 = CARTESIAN_POINT ( 'NONE',  ( 0.9253733321238560849, 8.064964547470342637, 0.3089666344597190029 ) ) ;
#38466 = CARTESIAN_POINT ( 'NONE',  ( -15.93236088550710861, 121.0320206851898206, -0.3693416020086464080 ) ) ;
#38467 = FACE_OUTER_BOUND ( 'NONE', #17817, .T. ) ;
#38468 = ORIENTED_EDGE ( 'NONE', *, *, #5800, .F. ) ;
#38469 = VECTOR ( 'NONE', #41294, 1000.000000000000000 ) ;
#38470 = CARTESIAN_POINT ( 'NONE',  ( 2.362235608990936431, 116.5348030743598287, 0.3959731454556020824 ) ) ;
#38471 = CARTESIAN_POINT ( 'NONE',  ( -4.377002418771855474, 72.24507371176854065, 1.270000000000004015 ) ) ;
#38472 = CARTESIAN_POINT ( 'NONE',  ( 9.211590693262500906, 119.0402042963619351, 1.266790605762086575 ) ) ;
#38473 = CARTESIAN_POINT ( 'NONE',  ( 10.16662615958531291, 120.4647147465577461, -1.171017801134732084 ) ) ;
#38474 = CARTESIAN_POINT ( 'NONE',  ( 8.270632439779459943, 13.09856730479051912, 1.690137114335896751 ) ) ;
#38475 = CARTESIAN_POINT ( 'NONE',  ( -14.52885936862958793, 121.1548589120785095, -1.307706137645302302 ) ) ;
#38476 = CARTESIAN_POINT ( 'NONE',  ( 4.691175111891225491, 117.9633576474440986, -0.7151038522473830428 ) ) ;
#38477 = CARTESIAN_POINT ( 'NONE',  ( 7.694725746745239015, 124.7202454748262710, 0.1536377669325636464 ) ) ;
#38478 = CARTESIAN_POINT ( 'NONE',  ( -15.54908666625173730, 147.5346097818530211, -0.08167737433607544228 ) ) ;
#38479 = CARTESIAN_POINT ( 'NONE',  ( -17.96932707993158473, 150.0321773811041339, -2.460285709456810022 ) ) ;
#38480 = EDGE_CURVE ( 'NONE', #35121, #40763, #3478, .T. ) ;
#38481 = CARTESIAN_POINT ( 'NONE',  ( 6.046978665186544255, -14.69723126592269224, 0.3844556930898083702 ) ) ;
#38482 = DIRECTION ( 'NONE',  ( -1.000000000000000000, 0.000000000000000000, -0.000000000000000000 ) ) ;
#38483 = EDGE_CURVE ( 'NONE', #32528, #33565, #24797, .T. ) ;
#38484 = CARTESIAN_POINT ( 'NONE',  ( -43.83556092231052048, 21.45200552150719631, -2.811646013901254015 ) ) ;
#38485 = VERTEX_POINT ( 'NONE', #18037 ) ;
#38486 = CARTESIAN_POINT ( 'NONE',  ( 18.13772925547819170, 148.8986565181125457, 2.425799293919265853 ) ) ;
#38487 = DIRECTION ( 'NONE',  ( 1.000000000000000000, -1.044409991968847179E-16, 0.000000000000000000 ) ) ;
#38488 = DIRECTION ( 'NONE',  ( 0.9575201071113178530, -0.2883665106726683858, 8.537024980200786319E-16 ) ) ;
#38489 = CARTESIAN_POINT ( 'NONE',  ( -3.904686386324561997, 121.5791280715047122, 0.1678698840778540258 ) ) ;
#38490 = CARTESIAN_POINT ( 'NONE',  ( 6.343129774801278487, 27.92810111164739340, -5.540698593559898910 ) ) ;
#38491 = CARTESIAN_POINT ( 'NONE',  ( 10.15204665306222687, 124.8647468421599598, 0.8418846390287858528 ) ) ;
#38492 = TOROIDAL_SURFACE ( 'NONE', #35093, 0.3809999999999990616, 0.2540000000000000036 ) ;
#38493 = CARTESIAN_POINT ( 'NONE',  ( 0.3417028577847283088, 116.8490449975401617, -0.2775575361029120613 ) ) ;
#38494 = CARTESIAN_POINT ( 'NONE',  ( -23.91048590848665611, 81.84235438443283783, -1.524000000000006239 ) ) ;
#38496 = B_SPLINE_CURVE_WITH_KNOTS ( 'NONE', 3,
 ( #25370, #38374, #15562, #35175, #10168, #22144, #22352, #6002, #3805, #18964, #39364, #31971, #28774, #23137, #41363, #36175, #16767, #35377 ),
 .UNSPECIFIED., .F., .F.,
 ( 4, 1, 1, 1, 1, 1, 2, 1, 1, 1, 2, 1, 1, 4 ),
 ( 0.000000000000000000, 0.1631003137318065010, 0.3262006274636130021, 0.4077507843295162804, 0.4893009411954195031, 0.5708510980613228369, 0.6524012549272261152, 0.6576100072399927443, 0.6628187595527594844, 0.6680275118655262245, 0.6732362641782929646, 0.7053937736304702888, 0.7375512830826476129, 0.7543499533659702161 ),
 .UNSPECIFIED. ) ;
#38495 = CARTESIAN_POINT ( 'NONE',  ( -2.032601633563780229E-14, 30.83083951148100255, -1.904999999999999805 ) ) ;
#38497 = UNCERTAINTY_MEASURE_WITH_UNIT (LENGTH_MEASURE( 1.000000000000000082E-05 ), #8767, 'distance_accuracy_value', 'NONE');
#38498 = CARTESIAN_POINT ( 'NONE',  ( -16.86202032626315628, 155.2029898760372646, -0.3369432954968343275 ) ) ;
#38499 = EDGE_LOOP ( 'NONE', ( #40523, #34582, #21884, #39340 ) ) ;
#38500 = CARTESIAN_POINT ( 'NONE',  ( -8.208076046625514266, 120.4389588540418714, -1.432247049196957667 ) ) ;
#38501 = DIRECTION ( 'NONE',  ( -5.188838149069471174E-16, 1.699382548006136313E-16, 1.000000000000000000 ) ) ;
#38502 = CARTESIAN_POINT ( 'NONE',  ( -15.44906575790740888, 148.0679034673509875, -1.029643479621237256 ) ) ;
#38503 = FACE_OUTER_BOUND ( 'NONE', #9270, .T. ) ;
#38504 = CARTESIAN_POINT ( 'NONE',  ( 23.11076619426176393, 149.9001102426712748, 0.4874744954944871811 ) ) ;
#38505 = ORIENTED_EDGE ( 'NONE', *, *, #18547, .T. ) ;
#38506 = CARTESIAN_POINT ( 'NONE',  ( -3.366035089439492811, 13.68705809737886447, 3.178168622443589886 ) ) ;
#38507 = CARTESIAN_POINT ( 'NONE',  ( -29.35321562997442513, 61.36487289457124206, 1.523999999999994470 ) ) ;
#38508 = CARTESIAN_POINT ( 'NONE',  ( -15.19604463793445959, 156.0859089222169587, -0.3036531364422413448 ) ) ;
#38509 = FACE_OUTER_BOUND ( 'NONE', #16776, .T. ) ;
#38510 = DIRECTION ( 'NONE',  ( 0.000000000000000000, 0.000000000000000000, -1.000000000000000000 ) ) ;
#38511 = CARTESIAN_POINT ( 'NONE',  ( 6.989499183820137240, 121.3060156903671043, 0.9293008224528782613 ) ) ;
#38512 = CARTESIAN_POINT ( 'NONE',  ( -3.128764270554720728, 7.249652477310866594, -3.416742352092642321 ) ) ;
#38513 = CARTESIAN_POINT ( 'NONE',  ( 20.32146383345304130, 132.1502320877631007, 1.598207211936853556 ) ) ;
#38514 = DIRECTION ( 'NONE',  ( -5.188838149069472160E-16, 1.699382548006136559E-16, 1.000000000000000000 ) ) ;
#38516 = CARTESIAN_POINT ( 'NONE',  ( 20.89924265627218603, 149.3152741295656369, -1.514357740512880968 ) ) ;
#38515 = CARTESIAN_POINT ( 'NONE',  ( 3.075357915497110017, -13.94103813162880989, 1.416127232796946966 ) ) ;
#38517 = CARTESIAN_POINT ( 'NONE',  ( -11.83945725349124878, 123.3160021321619695, 1.255757047829674011 ) ) ;
#38518 = CARTESIAN_POINT ( 'NONE',  ( -3.469956624915944587, 9.623539240006554252, 3.074419811715999984 ) ) ;
#38519 = CARTESIAN_POINT ( 'NONE',  ( -22.70904429024585980, 149.7444054411783441, -1.421740456058895985 ) ) ;
#38520 = ORIENTED_EDGE ( 'NONE', *, *, #9741, .F. ) ;
#38521 = AXIS2_PLACEMENT_3D ( 'NONE', #26057, #32255, #25643 ) ;
#38522 = CARTESIAN_POINT ( 'NONE',  ( -15.86984883002240387, 146.9522167609303267, 0.2762592943789939914 ) ) ;
#38523 = CARTESIAN_POINT ( 'NONE',  ( 5.936869294410564990, -12.97241973064336484, 1.608696005067407953 ) ) ;
#38524 = DIRECTION ( 'NONE',  ( -0.8745520943968235761, 0.4849315768086558398, -5.691349986800547879E-16 ) ) ;
#38525 = CARTESIAN_POINT ( 'NONE',  ( -4.563637803650490099, 118.0730259387059391, -0.7686314647840511993 ) ) ;
#38526 = B_SPLINE_CURVE_WITH_KNOTS ( 'NONE', 3,
 ( #37140, #23702, #20721, #1369 ),
 .UNSPECIFIED., .F., .F.,
 ( 4, 4 ),
 ( 0.001532986024144806884, 0.001758754979876016875 ),
 .UNSPECIFIED. ) ;
#38527 = CARTESIAN_POINT ( 'NONE',  ( 5.308493528853203358, 121.3525139070573147, 0.1060763342189517539 ) ) ;
#38528 = EDGE_CURVE ( 'NONE', #18529, #15597, #17621, .T. ) ;
#38529 = EDGE_LOOP ( 'NONE', ( #27102, #38110, #15300, #13770 ) ) ;
#38530 = CARTESIAN_POINT ( 'NONE',  ( 12.43266001442890278, 122.1796674805547980, 1.793313828261402287 ) ) ;
#38531 = CARTESIAN_POINT ( 'NONE',  ( 14.50851225146812595, 78.09971119798316863, 1.904999999999988258 ) ) ;
#38532 = DIRECTION ( 'NONE',  ( 0.01997839162482749689, 1.040247600000945640E-18, -0.9998004120163610509 ) ) ;
#38533 = CARTESIAN_POINT ( 'NONE',  ( -0.006370369177395581589, 117.0014201992989058, 0.3187993231787208948 ) ) ;
#38534 = CARTESIAN_POINT ( 'NONE',  ( 4.971096433842443041, 117.4753406598250223, -0.8637816793092503165 ) ) ;
#38535 = MANIFOLD_SOLID_BREP ( 'Stock-MAS-162-1', #26468 ) ;
#38536 = CARTESIAN_POINT ( 'NONE',  ( 8.206428610460235973, 117.5568930537867800, -0.09596530983984018215 ) ) ;
#38537 = DIRECTION ( 'NONE',  ( 0.9998004120163608288, 0.000000000000000000, 0.01997839162482736852 ) ) ;
#38538 = CARTESIAN_POINT ( 'NONE',  ( -46.85405389106658447, 25.56320314331479437, 1.590520987398670982 ) ) ;
#38539 = CARTESIAN_POINT ( 'NONE',  ( -46.60530155212502734, 26.17382724835478314, 1.396999999999990472 ) ) ;
#38540 = CARTESIAN_POINT ( 'NONE',  ( 1.964815052535200168, -15.28087767662020191, 5.362322688996490783 ) ) ;
#38541 = CARTESIAN_POINT ( 'NONE',  ( -47.65206802627297833, 20.46304711373551299, 5.210715034831059356 ) ) ;
#38542 = PLANE ( 'NONE',  #10462 ) ;
#38543 = CIRCLE ( 'NONE', #9301, 3.683000000000001162 ) ;
#38544 = CARTESIAN_POINT ( 'NONE',  ( -4.620544706279255287, 118.0223899981905618, 0.6740461278582655646 ) ) ;
#38545 = VECTOR ( 'NONE', #941, 1000.000000000000000 ) ;
#38546 = ORIENTED_EDGE ( 'NONE', *, *, #32124, .T. ) ;
#38547 = VERTEX_POINT ( 'NONE', #14214 ) ;
#38548 = DIRECTION ( 'NONE',  ( -5.188838149069472160E-16, 1.699382548006136559E-16, 1.000000000000000000 ) ) ;
#38549 = CARTESIAN_POINT ( 'NONE',  ( -5.896308022760929468, 119.0874697000712388, -1.261715751646591999 ) ) ;
#38550 = CARTESIAN_POINT ( 'NONE',  ( -4.040061035763231168, 117.6466181296975151, -0.9125624508345165919 ) ) ;
#38551 = CARTESIAN_POINT ( 'NONE',  ( 4.780600333925313805, 117.8746637532869670, 0.8584492858400551984 ) ) ;
#38552 = LINE ( 'NONE', #6386, #9350 ) ;
#38553 = CARTESIAN_POINT ( 'NONE',  ( -12.30032609686878153, 128.4316967252784991, -1.345898664372764175 ) ) ;
#38554 = CARTESIAN_POINT ( 'NONE',  ( -3.601659165084134973, 115.7029493297849285, -1.622342836042594216 ) ) ;
#38555 = CARTESIAN_POINT ( 'NONE',  ( -3.222237999455158430, 108.4800421235064363, 4.089189990378621964 ) ) ;
#38556 = DIRECTION ( 'NONE',  ( -0.6825627711659234542, -0.7308269722843399041, -2.299753143848148568E-16 ) ) ;
#38557 = CARTESIAN_POINT ( 'NONE',  ( 4.473299935328610033, 111.2795884869231173, -2.951234740152492986 ) ) ;
#38558 = CARTESIAN_POINT ( 'NONE',  ( -1.975234429548569537, 156.8313070664539168, -1.415192030232628850 ) ) ;
#38559 = DIRECTION ( 'NONE',  ( -0.9998004120163608288, 0.000000000000000000, -0.01997839162482749342 ) ) ;
#38560 = DIRECTION ( 'NONE',  ( -0.1728608224830406603, 0.000000000000000000, -0.9849462604886047856 ) ) ;
#38561 = CARTESIAN_POINT ( 'NONE',  ( -2.569109746590555687, 115.7029491485453150, 1.594660097005825117 ) ) ;
#38562 = CARTESIAN_POINT ( 'NONE',  ( -4.374560056058969693, 13.03735028915297534, 1.504755201125916875 ) ) ;
#38564 = ORIENTED_EDGE ( 'NONE', *, *, #26871, .F. ) ;
#38563 = CARTESIAN_POINT ( 'NONE',  ( 23.01936977803462625, 148.9204423966469335, 1.315221278248082548 ) ) ;
#38565 = CARTESIAN_POINT ( 'NONE',  ( 0.9339135649851527665, 105.1229431022307779, -5.262705770857304621 ) ) ;
#38566 = CARTESIAN_POINT ( 'NONE',  ( 3.824421424077324883, -15.38127155850414773, 2.203493915304267858 ) ) ;
#38567 = CARTESIAN_POINT ( 'NONE',  ( -14.55733092780593019, 125.6573275863457866, 1.461954306844538864 ) ) ;
#38568 = CARTESIAN_POINT ( 'NONE',  ( 0.6142125404598580696, 23.44653936994281906, -0.7587870835084352672 ) ) ;
#38569 = CIRCLE ( 'NONE', #22207, 9.048749999999998295 ) ;
#38570 = CARTESIAN_POINT ( 'NONE',  ( -0.2244654480080381653, 11.31155722793083918, -0.9512810396025579429 ) ) ;
#38571 = ORIENTED_EDGE ( 'NONE', *, *, #20697, .T. ) ;
#38572 = EDGE_CURVE ( 'NONE', #26682, #11267, #7849, .T. ) ;
#38573 = EDGE_LOOP ( 'NONE', ( #4576, #25001, #40399, #40579, #41619, #3258, #1452, #5997, #147, #25287, #16619, #21629, #23416, #21419, #29713, #28470, #4524, #24838, #29699, #27514, #2386, #10152, #9886, #9445, #22855, #9564, #28872, #20630, #20891, #31893, #5579, #11884, #33850, #34740, #17285, #14290, #22028, #9774, #30002, #21799, #29774, #5211, #34810, #36517, #7759, #1959, #18408, #17922, #7410, #13376, #9184, #36020, #22360, #21774, #22203, #38884, #37463, #21443, #13295, #1287, #24295, #42081, #41332, #18425, #39239, #2637, #378, #22485, #39770, #5475, #18720, #8527, #11147, #17450, #7549, #19312 ) ) ;
#38574 = FACE_OUTER_BOUND ( 'NONE', #1952, .T. ) ;
#38575 = CARTESIAN_POINT ( 'NONE',  ( 6.294717182677755041, 121.9812576474260055, 0.2818399057506481009 ) ) ;
#38576 = CARTESIAN_POINT ( 'NONE',  ( -12.09414715658302875, 128.3964238929853252, 0.7197952935306337618 ) ) ;
#38577 = DIRECTION ( 'NONE',  ( 0.01731298258488003436, -0.9998501190848634312, 0.000000000000000000 ) ) ;
#38578 = CARTESIAN_POINT ( 'NONE',  ( 3.537338181458673070, -13.91857904597952533, 4.048280000481319973 ) ) ;
#38579 = CARTESIAN_POINT ( 'NONE',  ( 10.94646760555348308, 123.1276765127550021, -1.119819633367153067 ) ) ;
#38580 = CIRCLE ( 'NONE', #27680, 5.080000000000006288 ) ;
#38581 = CARTESIAN_POINT ( 'NONE',  ( -8.716850226171729332, 156.9002828235886966, -2.058648441535007478 ) ) ;
#38582 = LINE ( 'NONE', #2812, #12534 ) ;
#38583 = ADVANCED_FACE ( 'NONE', ( #33836 ), #4664, .T. ) ;
#38584 = CARTESIAN_POINT ( 'NONE',  ( 8.060526367258390223, 121.1727610582439780, 1.293028985890418925 ) ) ;
#38585 = CARTESIAN_POINT ( 'NONE',  ( -5.478259115505812460, 32.09053017494222360, 1.574172154844436289 ) ) ;
#38586 = CARTESIAN_POINT ( 'NONE',  ( 15.60869185768498113, 147.5518517437054982, -0.1389895172399196188 ) ) ;
#38587 = AXIS2_PLACEMENT_3D ( 'NONE', #28384, #2418, #18356 ) ;
#38588 = EDGE_LOOP ( 'NONE', ( #34912, #2797, #35453, #15123 ) ) ;
#38589 = CYLINDRICAL_SURFACE ( 'NONE', #21063, 0.5080000000000000071 ) ;
#38590 = DIRECTION ( 'NONE',  ( 0.000000000000000000, 0.000000000000000000, -1.000000000000000000 ) ) ;
#38591 = DIRECTION ( 'NONE',  ( 0.8745520943968235761, -0.4849315768086558398, 4.268512490100410909E-16 ) ) ;
#38592 = EDGE_CURVE ( 'NONE', #7084, #27091, #24427, .T. ) ;
#38593 = CARTESIAN_POINT ( 'NONE',  ( -8.398906084147393258, 18.04027321918359306, -0.8732425085428288103 ) ) ;
#38594 = CARTESIAN_POINT ( 'NONE',  ( 5.862724111891608025, 121.1554468101848130, 0.6631653705238501617 ) ) ;
#38595 = CARTESIAN_POINT ( 'NONE',  ( -6.637366883016756296E-14, 101.1854662015457365, -1.207165459283692464E-19 ) ) ;
#38596 = CARTESIAN_POINT ( 'NONE',  ( 23.11138188961074746, 149.8995197111492814, 0.3848215369211052117 ) ) ;
#38597 = CARTESIAN_POINT ( 'NONE',  ( -5.927223324825597217, 118.9825038774357466, 0.3493763292145123378 ) ) ;
#38598 = AXIS2_PLACEMENT_3D ( 'NONE', #3959, #4166, #30130 ) ;
#38599 = CARTESIAN_POINT ( 'NONE',  ( -3.682264917456323783, 82.64346620154573486, -0.07358041635423923088 ) ) ;
#38600 = CARTESIAN_POINT ( 'NONE',  ( 0.02537255736346739551, 39.20946620154573026, -1.269746523260778970 ) ) ;
#38601 = CARTESIAN_POINT ( 'NONE',  ( 20.78747236883564398, 145.7124547906547889, 2.408930808681182256 ) ) ;
#38602 = EDGE_CURVE ( 'NONE', #4128, #29982, #25527, .T. ) ;
#38603 = CARTESIAN_POINT ( 'NONE',  ( 6.343129774801278487, 27.92810111164739340, -5.540698593559898910 ) ) ;
#38604 = CARTESIAN_POINT ( 'NONE',  ( 8.753617840798051830, 117.9548258552378002, -0.3763906928539145214 ) ) ;
#38605 = CARTESIAN_POINT ( 'NONE',  ( 0.1065646865915095692, 105.8844662015456919, -5.332932678536313809 ) ) ;
#38606 = DIRECTION ( 'NONE',  ( -1.000000000000000000, 0.000000000000000000, 3.035386659626960118E-16 ) ) ;
#38607 = DIRECTION ( 'NONE',  ( -0.8745520943968241312, 0.4849315768086548406, -5.691349986800536046E-16 ) ) ;
#38608 = CARTESIAN_POINT ( 'NONE',  ( -3.347088983057015632, 104.6144662015458096, 3.489637925356170456 ) ) ;
#38609 = CARTESIAN_POINT ( 'NONE',  ( 0.9564925537785137211, 29.00497265395555857, -4.523030980006896407 ) ) ;
#38610 = PLANE ( 'NONE',  #37526 ) ;
#38611 = DIRECTION ( 'NONE',  ( -0.6559537821943239866, 0.7548010569845283735, -4.686333752532408853E-16 ) ) ;
#38612 = CARTESIAN_POINT ( 'NONE',  ( 2.569204629087775693, -14.95572128602136530, 4.738577790166504933 ) ) ;
#38613 = EDGE_CURVE ( 'NONE', #19493, #41093, #20748, .T. ) ;
#38614 = CARTESIAN_POINT ( 'NONE',  ( 1.593197492609314647, 110.3135721340718334, -3.506749948187484200 ) ) ;
#38615 = CARTESIAN_POINT ( 'NONE',  ( -0.9832365512849939870, 116.8374933757159795, 0.2893350595372073952 ) ) ;
#38616 = AXIS2_PLACEMENT_3D ( 'NONE', #19000, #22391, #16217 ) ;
#38617 = VERTEX_POINT ( 'NONE', #5714 ) ;
#38618 = CARTESIAN_POINT ( 'NONE',  ( 5.028141926494226865, 117.3993840561512485, -0.6263463072690832467 ) ) ;
#38619 = EDGE_CURVE ( 'NONE', #27003, #15597, #31282, .T. ) ;
#38620 = VERTEX_POINT ( 'NONE', #19875 ) ;
#38621 = DIRECTION ( 'NONE',  ( -0.8745520943968235761, 0.4849315768086558398, -5.691349986800547879E-16 ) ) ;
#38622 = CARTESIAN_POINT ( 'NONE',  ( 4.515093156845158440, -15.50826969562475810, 4.181389551362865831 ) ) ;
#38623 = CARTESIAN_POINT ( 'NONE',  ( -10.28923284337283661, 120.3038588096988803, 1.141564125291498311 ) ) ;
#38624 = CARTESIAN_POINT ( 'NONE',  ( 0.3839177515434519794, 117.3568105388816321, -0.4297925318014834684 ) ) ;
#38625 = EDGE_CURVE ( 'NONE', #37552, #29590, #18033, .T. ) ;
#38626 = CARTESIAN_POINT ( 'NONE',  ( 4.513502956352341222, 8.064680226961385756, -0.9949261897555528034 ) ) ;
#38627 = CARTESIAN_POINT ( 'NONE',  ( -56.27576540577094732, 4.709657678713138118, -2.637635859394501292 ) ) ;
#38628 = ORIENTED_EDGE ( 'NONE', *, *, #19707, .F. ) ;
#38629 = CARTESIAN_POINT ( 'NONE',  ( -58.34386316732116740, -0.2371896724559646730, -0.2005938501612954394 ) ) ;
#38630 = CARTESIAN_POINT ( 'NONE',  ( -0.01254005783545543429, 120.1716774721351157, 0.6275557724548022076 ) ) ;
#38631 = CARTESIAN_POINT ( 'NONE',  ( -4.747830334022490106, 117.7228629901014614, 0.9149653662667899257 ) ) ;
#38632 = CARTESIAN_POINT ( 'NONE',  ( -17.30282355392138172, 146.5563353440282981, 1.366477706345458287 ) ) ;
#38633 = CARTESIAN_POINT ( 'NONE',  ( 5.138887090645153144, 116.8853669287380797, 0.2852080145627308716 ) ) ;
#38634 = CARTESIAN_POINT ( 'NONE',  ( 18.16172641238590657, 140.6071502257508143, -1.752259283733317297 ) ) ;
#38635 = CARTESIAN_POINT ( 'NONE',  ( -20.83122434882630003, 148.6614476615901594, -2.397187407820276395 ) ) ;
#38636 = CARTESIAN_POINT ( 'NONE',  ( -58.24807683554808335, 1.288543178753334573, -1.357556113208963744 ) ) ;
#38637 = AXIS2_PLACEMENT_3D ( 'NONE', #34380, #2012, #31385 ) ;
#38638 = EDGE_LOOP ( 'NONE', ( #9729, #18785, #40614, #21136 ) ) ;
#38639 = CARTESIAN_POINT ( 'NONE',  ( 9.542276680740265249, 123.9284174147966269, -0.4124357159827418684 ) ) ;
#38640 = ORIENTED_EDGE ( 'NONE', *, *, #16727, .F. ) ;
#38641 = CARTESIAN_POINT ( 'NONE',  ( -3.383623802199918984, 119.6896249646678569, -0.8128912582704552747 ) ) ;
#38642 = CARTESIAN_POINT ( 'NONE',  ( 3.491209331645790837, -14.97137451562302601, 1.144833103274278230 ) ) ;
#38643 = DIRECTION ( 'NONE',  ( 0.9998004120163610509, 4.016384292689131511E-17, 0.01997839162482749689 ) ) ;
#38644 = DIRECTION ( 'NONE',  ( 1.000000000000000000, -9.466894658874049451E-17, 0.000000000000000000 ) ) ;
#38645 = CARTESIAN_POINT ( 'NONE',  ( -4.781588677966720269, 117.7629110891638362, 0.8765192077237911050 ) ) ;
#38646 = CARTESIAN_POINT ( 'NONE',  ( 12.10021064141416502, 153.5325627063460843, 2.025425248842404269 ) ) ;
#38647 = CARTESIAN_POINT ( 'NONE',  ( -0.7387659178326326792, 32.94979111317254450, 0.8178967711910595240 ) ) ;
#38648 = CARTESIAN_POINT ( 'NONE',  ( -4.460028654926622593, 22.53297844546955631, 1.214995109042491528 ) ) ;
#38649 = CARTESIAN_POINT ( 'NONE',  ( 8.124409605001838841, 122.8458379852381910, 0.3720714147651332793 ) ) ;
#38650 = CARTESIAN_POINT ( 'NONE',  ( -18.35410564743290607, 77.35382415001784295, 5.016499999999999737 ) ) ;
#38651 = EDGE_CURVE ( 'NONE', #31590, #19292, #23058, .T. ) ;
#38653 = ADVANCED_FACE ( 'NONE', ( #39492 ), #14015, .T. ) ;
#38652 = CARTESIAN_POINT ( 'NONE',  ( -45.43219756685621036, 19.09711438432238495, -1.200471166368914933 ) ) ;
#38654 = DIRECTION ( 'NONE',  ( -0.8745520943968250194, 0.4849315768086535083, -5.424246918827963022E-16 ) ) ;
#38655 = CARTESIAN_POINT ( 'NONE',  ( -47.16890147375944764, 22.20336809214633433, 4.187060126831872786 ) ) ;
#38656 = CARTESIAN_POINT ( 'NONE',  ( -53.84782375693468737, 9.539003880032991489, 3.783945623633715893 ) ) ;
#38657 = CARTESIAN_POINT ( 'NONE',  ( -8.232873692804936638, 120.3172065538984015, -1.441392283162307830 ) ) ;
#38658 = AXIS2_PLACEMENT_3D ( 'NONE', #6617, #19175, #19380 ) ;
#38659 = DIRECTION ( 'NONE',  ( 1.000000000000000000, -9.466894658874049451E-17, 0.000000000000000000 ) ) ;
#38660 = CARTESIAN_POINT ( 'NONE',  ( -54.56940519185135230, 9.666406039105165604, 3.302709833357596381 ) ) ;
#38661 = CARTESIAN_POINT ( 'NONE',  ( -3.277668934457586669, 159.4655167044000166, 0.1355973003551880496 ) ) ;
#38662 = ORIENTED_EDGE ( 'NONE', *, *, #23309, .T. ) ;
#38663 = CARTESIAN_POINT ( 'NONE',  ( -52.46220839783629941, 13.84563717269405458, -4.010158452165651255 ) ) ;
#38664 = CARTESIAN_POINT ( 'NONE',  ( -6.954920274790141299, 121.9415326885807929, -0.2649906444065315281 ) ) ;
#38665 = EDGE_CURVE ( 'NONE', #7253, #2316, #34387, .T. ) ;
#38666 = ORIENTED_EDGE ( 'NONE', *, *, #25378, .T. ) ;
#38667 = CARTESIAN_POINT ( 'NONE',  ( 0.7269968954376242465, 115.7031256804406780, -1.730797724436444307 ) ) ;
#38668 = CARTESIAN_POINT ( 'NONE',  ( -15.64343260727715013, 147.2205073051419504, -0.4407941163815355390 ) ) ;
#38669 = CARTESIAN_POINT ( 'NONE',  ( 3.596007053926196573, -14.96754207850672991, 5.407624617413868684 ) ) ;
#38670 = CARTESIAN_POINT ( 'NONE',  ( -13.76672422736547396, 155.7522398296385404, 1.402631553274309439 ) ) ;
#38671 = CARTESIAN_POINT ( 'NONE',  ( 6.059261036833980540, 78.87450423423040036, -5.016499999999999737 ) ) ;
#38672 = CARTESIAN_POINT ( 'NONE',  ( 18.63890302240343999, 125.2334963081946313, 0.6306532867605573189 ) ) ;
#38673 = EDGE_CURVE ( 'NONE', #30834, #20737, #13966, .T. ) ;
#38674 = CARTESIAN_POINT ( 'NONE',  ( 2.863236596730719619, 121.0282055654512163, 0.1599167813194848631 ) ) ;
#38675 = CARTESIAN_POINT ( 'NONE',  ( 4.844094425375155666, 115.6909491485453145, -1.283570666956070694 ) ) ;
#38676 = CARTESIAN_POINT ( 'NONE',  ( -0.4248780512631177841, 5.470267980206036107, 0.8793239699972363876 ) ) ;
#38677 = CARTESIAN_POINT ( 'NONE',  ( -23.10027255048459693, 149.8968678342272653, -0.6153025774343640064 ) ) ;
#38678 = LINE ( 'NONE', #6095, #518 ) ;
#38679 = CARTESIAN_POINT ( 'NONE',  ( -17.14500000000466784, 71.11999999999886768, 1.523999999999998689 ) ) ;
#38680 = EDGE_LOOP ( 'NONE', ( #29075, #9233, #7151, #30653 ) ) ;
#38681 = CARTESIAN_POINT ( 'NONE',  ( -2.485165897956930880, 116.7121408797957400, 0.3916859838625323387 ) ) ;
#38682 = ORIENTED_EDGE ( 'NONE', *, *, #38528, .F. ) ;
#38683 = CARTESIAN_POINT ( 'NONE',  ( -58.37116772670351850, -0.2940390518722524327, -2.603646672650065119E-13 ) ) ;
#38684 = CARTESIAN_POINT ( 'NONE',  ( 3.034986042679733487, 117.6993298527280984, 0.7527370910433335283 ) ) ;
#38685 = CARTESIAN_POINT ( 'NONE',  ( 8.792132358471045350, 156.9002828235886966, -1.708777300431143509 ) ) ;
#38686 = CARTESIAN_POINT ( 'NONE',  ( 4.144591825430580911, 15.01708852069707945, -7.363685156706923252 ) ) ;
#38687 = CARTESIAN_POINT ( 'NONE',  ( -5.210988722241271631, 158.8115599018184412, -1.325654878232527478 ) ) ;
#38688 = CARTESIAN_POINT ( 'NONE',  ( 4.674864129759326303, 117.9626304797967720, -0.7310746242011807450 ) ) ;
#38689 = CARTESIAN_POINT ( 'NONE',  ( 15.47023807670824525, 120.6682698389898576, 0.3091321738930620788 ) ) ;
#38690 = CARTESIAN_POINT ( 'NONE',  ( -8.507314851146933421, 123.3280575159016905, -0.1373787248657619975 ) ) ;
#38691 = CARTESIAN_POINT ( 'NONE',  ( -0.9722352627953847470, 157.7941190989783991, -1.644571785473255998 ) ) ;
#38692 = CARTESIAN_POINT ( 'NONE',  ( 2.911953930276938607, -15.74143402046077078, 5.333341296191352221 ) ) ;
#38693 = DIRECTION ( 'NONE',  ( 5.188838149069472160E-16, -1.699382548006136559E-16, -1.000000000000000000 ) ) ;
#38694 = CARTESIAN_POINT ( 'NONE',  ( -47.00787117332040310, 24.49876931072293829, -2.333946431867834015 ) ) ;
#38695 = ORIENTED_EDGE ( 'NONE', *, *, #19649, .T. ) ;
#38696 = CARTESIAN_POINT ( 'NONE',  ( 11.80606196054485579, 122.9427978038690270, 1.750206178813383806 ) ) ;
#38697 = CARTESIAN_POINT ( 'NONE',  ( -12.21488373879589240, 55.24499999999999034, -5.016499999999999737 ) ) ;
#38698 = CIRCLE ( 'NONE', #24376, 0.2539999999999998925 ) ;
#38699 = AXIS2_PLACEMENT_3D ( 'NONE', #6298, #3106, #16067 ) ;
#38700 = CARTESIAN_POINT ( 'NONE',  ( -29.81357423954495189, 70.62209452652477637, -1.270000000000007123 ) ) ;
#38701 = CARTESIAN_POINT ( 'NONE',  ( -4.022785008251061889, 122.0441497943765370, 0.1183375255305478546 ) ) ;
#38702 = CARTESIAN_POINT ( 'NONE',  ( 8.340720164204880049, -15.19402286670749191, -1.049415519506536665 ) ) ;
#38703 = CARTESIAN_POINT ( 'NONE',  ( 10.85076598842368334, 126.1616406593870607, 0.8982697194533709739 ) ) ;
#38704 = CARTESIAN_POINT ( 'NONE',  ( 2.917496378899068432, 117.0242007548465608, -0.3950530357975749474 ) ) ;
#38705 = CARTESIAN_POINT ( 'NONE',  ( -17.14500000000466784, 71.11999999999886768, -1.524000000000000909 ) ) ;
#38706 = DIRECTION ( 'NONE',  ( 0.8745520943968250194, -0.4849315768086534528, 5.361993529360573944E-16 ) ) ;
#38707 = CARTESIAN_POINT ( 'NONE',  ( -23.36108720469573186, 148.8745345081378559, -0.4410421544236567959 ) ) ;
#38708 = ORIENTED_EDGE ( 'NONE', *, *, #9148, .T. ) ;
#38709 = CARTESIAN_POINT ( 'NONE',  ( 8.198008058078954718, 120.7314922977370912, -1.065926864482704683 ) ) ;
#38710 = CARTESIAN_POINT ( 'NONE',  ( 5.586884702347365561, 75.27746620154573520, 0.1116392523995368286 ) ) ;
#38711 = CARTESIAN_POINT ( 'NONE',  ( -15.93611381433512264, 145.8030804522035737, -1.048911189365803631 ) ) ;
#38712 = DIRECTION ( 'NONE',  ( -5.188838149069471174E-16, 1.699382548006136313E-16, 1.000000000000000000 ) ) ;
#38713 = CARTESIAN_POINT ( 'NONE',  ( 23.45208337669170007, 146.8499405026647651, 0.4686284387228156212 ) ) ;
#38714 = ADVANCED_FACE ( 'NONE', ( #7761 ), #14330, .F. ) ;
#38715 = ORIENTED_EDGE ( 'NONE', *, *, #36768, .T. ) ;
#38716 = CARTESIAN_POINT ( 'NONE',  ( 2.003160574663116034, 15.61121511114846960, 4.187759092076685619 ) ) ;
#38717 = CARTESIAN_POINT ( 'NONE',  ( -23.34372044207216845, 149.0681261006882039, -0.4664630893996629113 ) ) ;
#38718 = CARTESIAN_POINT ( 'NONE',  ( -4.901945799063080145, 117.4108088126838112, 0.9677811563769884717 ) ) ;
#38719 = DIRECTION ( 'NONE',  ( -1.000000000000000000, 1.288607544181256696E-16, 0.000000000000000000 ) ) ;
#38720 = CARTESIAN_POINT ( 'NONE',  ( -10.28897677580358305, 56.51499999999998636, 4.381500000000000838 ) ) ;
#38721 = CARTESIAN_POINT ( 'NONE',  ( 5.726410507774571279, 120.0273765416552578, 1.077413901059734114 ) ) ;
#38722 = AXIS2_PLACEMENT_3D ( 'NONE', #2889, #12669, #29859 ) ;
#38723 = CARTESIAN_POINT ( 'NONE',  ( -0.5507456681092424144, 15.89564879194059799, -4.587442282481805300 ) ) ;
#38724 = CARTESIAN_POINT ( 'NONE',  ( 10.35357550766347678, 157.8614378686282862, 1.168524991271691738 ) ) ;
#38725 = DIRECTION ( 'NONE',  ( -4.017660918040594346E-17, 1.000000000000000000, 2.376309959284834438E-19 ) ) ;
#38727 = CARTESIAN_POINT ( 'NONE',  ( 20.68240061501449389, 141.5323519391372997, -1.529040698034871637 ) ) ;
#38726 = CARTESIAN_POINT ( 'NONE',  ( 3.543852116809842467, 109.5877551946028632, 3.777766483051805846 ) ) ;
#38728 = CLOSED_SHELL ( 'NONE', ( #10522, #29273, #33205, #39316, #40508, #3197, #28770, #30290, #35300, #155, #1111, #3711, #13923, #7743, #24211, #21571, #22765, #37582, #1384, #16236, #6164, #29529, #22980, #35491, #5600, #34915, #12882, #10048, #17226, #35705, #31052, #35399, #3818, #3979, #33520, #29759, #22415, #1515, #14696, #23441, #16298, #19331, #3500, #29829, #9244, #1971, #13409, #18393, #21609, #30919, #6063, #33165, #4018, #37175, #36300, #13397, #39476, #20568, #6020, #21756, #24711, #10232, #19120, #33192, #39435, #698, #11588, #11762, #25951, #14617, #27453, #19597, #14831, #16199, #42028, #32955, #12742, #15418, #36790, #41025, #33582, #24542, #21212, #9240, #31883, #28668, #11872, #25152, #38435, #35302, #22813, #29988, #3995, #17763, #38339, #7866, #16538, #11289, #17748, #20933, #3232, #7852, #35011, #39486, #17252, #111, #34978, #23784, #1622, #13359, #1602, #27370, #13985, #1705, #33402, #36067, #30923, #15173, #6356, #23798, #32405, #20948, #34019, #101, #36803, #15981, #8988, #30510, #29484, #3773, #20959, #41707, #41167, #3181, #1672, #35760, #9758, #23051, #25623, #37895, #19703, #13470, #26929, #29433, #4697, #22484, #39720, #23591, #12791, #15734, #24263, #18288, #9698, #41515, #28273, #30026, #32886, #31024, #2030, #32394, #11229, #17456, #23817, #35543, #32714, #21595, #40430, #11805, #4005, #12799, #1612, #16932, #22230, #14461, #30756, #7447, #22005, #7363, #26584, #37616, #23525, #5497, #8935, #8468, #618, #6945, #32651, #3334, #23450, #29187, #24270, #2121, #26391, #6122, #23463, #16828, #27739, #35836, #9048, #35247, #25325, #8646, #2664, #9044, #1407, #2028, #11510, #2171, #20275, #41805, #22463, #18601, #36843, #24353, #23249, #35818, #31382, #29330, #13135, #3730, #31152, #41734, #32228, #28577, #40713, #5809, #13354, #6628, #9658, #28938, #21894, #16758, #8143, #31742, #37306, #6947, #33699, #7106, #40188, #31244, #32656, #16521, #22240, #25391, #31695, #40553 ) ) ;
#38729 = CARTESIAN_POINT ( 'NONE',  ( -0.5165578309945342284, 6.287656885725535716, -4.620190224396742984 ) ) ;
#38730 = CARTESIAN_POINT ( 'NONE',  ( -6.888626713468250173, 117.5201695557886410, -0.7016588733424086177 ) ) ;
#38731 = ORIENTED_EDGE ( 'NONE', *, *, #29800, .T. ) ;
#38732 = CARTESIAN_POINT ( 'NONE',  ( -11.98620439842969887, 151.9649008058812569, 0.3157042427443432775 ) ) ;
#38733 = CARTESIAN_POINT ( 'NONE',  ( 5.096701352355580639, -14.12304281641942083, 3.871056799387667002 ) ) ;
#38734 = CARTESIAN_POINT ( 'NONE',  ( -29.94429436251954613, 71.80236127745905605, -1.524000000000007571 ) ) ;
#38735 = CARTESIAN_POINT ( 'NONE',  ( -4.537028399616379382, 118.0323947479856770, -0.8637156260805385344 ) ) ;
#38736 = CARTESIAN_POINT ( 'NONE',  ( 15.72781737677511593, 145.6903699455376113, 0.2627434299976846854 ) ) ;
#38737 = VERTEX_POINT ( 'NONE', #37716 ) ;
#38738 = CARTESIAN_POINT ( 'NONE',  ( 8.716850226171599658, 156.9002828235886966, 2.058648441535007922 ) ) ;
#38739 = DIRECTION ( 'NONE',  ( -0.6850534820564764260, 0.7284927773988544297, 1.146843430008119832E-15 ) ) ;
#38740 = DIRECTION ( 'NONE',  ( -0.9876665170007968841, 0.1565721916417945614, -2.874959381037663881E-15 ) ) ;
#38741 = CARTESIAN_POINT ( 'NONE',  ( -22.70688998881783505, 149.0844379882532849, 0.7271790501850814437 ) ) ;
#38742 = CARTESIAN_POINT ( 'NONE',  ( 4.815708689467896875, 117.5416844730284680, -0.9797437855538944085 ) ) ;
#38743 = AXIS2_PLACEMENT_3D ( 'NONE', #29729, #3557, #16516 ) ;
#38744 = CARTESIAN_POINT ( 'NONE',  ( 13.30261597551684360, 156.9705208988102640, -0.2305920065817561315 ) ) ;
#38745 = CIRCLE ( 'NONE', #2711, 2.540000000000000480 ) ;
#38746 = CARTESIAN_POINT ( 'NONE',  ( -11.05715273818225164, 82.67346420587206524, -1.523999999999999577 ) ) ;
#38747 = CARTESIAN_POINT ( 'NONE',  ( -48.09020259270877062, 19.08749025517105480, 5.202481609175432453 ) ) ;
#38748 = DIRECTION ( 'NONE',  ( -9.627370216492862708E-17, -1.000000000000000000, 0.000000000000000000 ) ) ;
#38749 = CARTESIAN_POINT ( 'NONE',  ( 1.877026549479959172, -15.08352304062032800, 5.583147605863830520 ) ) ;
#38750 = CARTESIAN_POINT ( 'NONE',  ( -45.91718695868514288, 25.22619731686664224, 1.578102078770057037 ) ) ;
#38751 = CARTESIAN_POINT ( 'NONE',  ( -58.81095673130623425, -0.2799022426899211990, 0.1165709727617455505 ) ) ;
#38752 = CARTESIAN_POINT ( 'NONE',  ( -4.614943955948183074, 118.0411468392323400, 0.6409247712607968328 ) ) ;
#38753 = CARTESIAN_POINT ( 'NONE',  ( -58.28497307353767809, -0.1385909279409680561, -1.048413496073990905E-14 ) ) ;
#38754 = VERTEX_POINT ( 'NONE', #5358 ) ;
#38755 = EDGE_LOOP ( 'NONE', ( #6116, #4855, #9545, #15056, #6920, #34446 ) ) ;
#38756 = CARTESIAN_POINT ( 'NONE',  ( -0.7730009467963616654, 115.6909491485452435, -1.757285791594641822 ) ) ;
#38757 = CARTESIAN_POINT ( 'NONE',  ( -8.352514336526260408, 119.7346528407997255, -1.431646670230054541 ) ) ;
#38758 = CARTESIAN_POINT ( 'NONE',  ( -5.553235467069472797, 117.9513286348681476, -0.7459228754688890239 ) ) ;
#38759 = CARTESIAN_POINT ( 'NONE',  ( 4.623035167900726883, 118.0214275984946113, 0.8252090714975102159 ) ) ;
#38760 = CARTESIAN_POINT ( 'NONE',  ( 3.212496809824684441, -14.25148094350509353, 2.370051959060230473 ) ) ;
#38761 = CARTESIAN_POINT ( 'NONE',  ( -11.38067935084468552, 126.1532465342912985, -1.245950066931532874 ) ) ;
#38762 = CARTESIAN_POINT ( 'NONE',  ( -2.906692822798004006, 115.7029491485453576, -1.674875336659100489 ) ) ;
#38763 = CARTESIAN_POINT ( 'NONE',  ( -6.059261036834476144, 56.51499999999998636, 4.547742611252458822 ) ) ;
#38764 = CARTESIAN_POINT ( 'NONE',  ( -6.439703808512989190E-14, 63.33946620154573282, 4.464395889055755859E-29 ) ) ;
#38765 = CARTESIAN_POINT ( 'NONE',  ( 5.398477100378374693, 117.1940586887245388, -0.6826447346010610095 ) ) ;
#38766 = CARTESIAN_POINT ( 'NONE',  ( -16.41634355132965695, 139.9843038322558186, -2.146987391100668496 ) ) ;
#38767 = CYLINDRICAL_SURFACE ( 'NONE', #10567, 1.270000000000000240 ) ;
#38768 = CARTESIAN_POINT ( 'NONE',  ( -0.01289612358334801118, 159.5048567107479585, 0.6453747585945883714 ) ) ;
#38769 = DIRECTION ( 'NONE',  ( -5.188838149069471174E-16, 1.699382548006136313E-16, 1.000000000000000000 ) ) ;
#38770 = CARTESIAN_POINT ( 'NONE',  ( -2.948169924849943335, 1.592661447142720732, -3.562413953034572867 ) ) ;
#38772 = ORIENTED_EDGE ( 'NONE', *, *, #26151, .F. ) ;
#38771 = CARTESIAN_POINT ( 'NONE',  ( 1.907136510351249870, 116.7789519286944966, 0.3469662120689608886 ) ) ;
#38773 = CARTESIAN_POINT ( 'NONE',  ( -24.32950799593924884, 77.42192949967211746, 1.523999999999993804 ) ) ;
#38774 = CARTESIAN_POINT ( 'NONE',  ( 2.939911579247540541, -15.51555475658629391, 4.434558482745560859 ) ) ;
#38775 = CARTESIAN_POINT ( 'NONE',  ( -19.35587726549920262, 148.6897983921382433, 1.735459330159159208 ) ) ;
#38776 = CARTESIAN_POINT ( 'NONE',  ( -0.2928493810785644524, 9.627489959316354984, 0.9317482488014678932 ) ) ;
#38777 = CARTESIAN_POINT ( 'NONE',  ( -0.9401033786448180773, 4.191251494893229790, 0.2723526238743522732 ) ) ;
#38778 = ORIENTED_EDGE ( 'NONE', *, *, #25566, .F. ) ;
#38779 = AXIS2_PLACEMENT_3D ( 'NONE', #17041, #674, #26635 ) ;
#38780 = ORIENTED_EDGE ( 'NONE', *, *, #17244, .T. ) ;
#38781 = CARTESIAN_POINT ( 'NONE',  ( -20.83467972660109169, 65.95194780259438971, 5.016499999999999737 ) ) ;
#38782 = CARTESIAN_POINT ( 'NONE',  ( -0.1065646865916382163, 105.8844662015457061, 5.332932678536314697 ) ) ;
#38783 = DIRECTION ( 'NONE',  ( 1.000000000000000000, 0.000000000000000000, 0.000000000000000000 ) ) ;
#38784 = CARTESIAN_POINT ( 'NONE',  ( -4.453624852893828034, 120.7762672505206041, 0.3811677228292795205 ) ) ;
#38785 = CARTESIAN_POINT ( 'NONE',  ( 4.304563788583176454, -12.55325912034982494, 2.095985231258857162 ) ) ;
#38786 = CARTESIAN_POINT ( 'NONE',  ( 13.85457725998112011, 128.5353789189983900, -1.357273257441080849 ) ) ;
#38787 = CARTESIAN_POINT ( 'NONE',  ( -4.389113801267393811, 157.7533977378147654, -1.847790720561485411 ) ) ;
#38788 = DIRECTION ( 'NONE',  ( -4.017660918040594346E-17, 1.000000000000000000, 2.376309959284834438E-19 ) ) ;
#38789 = CARTESIAN_POINT ( 'NONE',  ( 8.243466591241450203, 120.2651585749115668, 1.445033792603914513 ) ) ;
#38790 = CARTESIAN_POINT ( 'NONE',  ( -5.541434792369814843, 31.48360339932893126, -0.006023868707823998130 ) ) ;
#38791 = CARTESIAN_POINT ( 'NONE',  ( 9.165091971927566306, 123.9989874199980022, -0.04717021870285740409 ) ) ;
#38792 = ORIENTED_EDGE ( 'NONE', *, *, #26678, .F. ) ;
#38793 = DIRECTION ( 'NONE',  ( 1.254648257879299356E-08, -1.000000000000000000, 2.507086335409856190E-10 ) ) ;
#38794 = CARTESIAN_POINT ( 'NONE',  ( 11.58677707360137532, 55.98894877578617724, -4.474811398758259173 ) ) ;
#38795 = CARTESIAN_POINT ( 'NONE',  ( -4.583145339712576316, 27.87760190724945275, 0.5120832130390071679 ) ) ;
#38796 = CARTESIAN_POINT ( 'NONE',  ( 11.02756477914268629, 153.1537610418535849, 1.395931567138233298 ) ) ;
#38797 = FACE_OUTER_BOUND ( 'NONE', #11075, .T. ) ;
#38798 = CARTESIAN_POINT ( 'NONE',  ( 1.417759636995359784, 159.6040221172770259, -0.05833233067434073077 ) ) ;
#38799 = CARTESIAN_POINT ( 'NONE',  ( -5.274668375481318172, 116.0897965414613964, 1.029904101180854514 ) ) ;
#38800 = CIRCLE ( 'NONE', #20415, 0.5080000000000002292 ) ;
#38801 = CARTESIAN_POINT ( 'NONE',  ( -4.466782427718574588, 71.06098887363195615, -1.523999999999994248 ) ) ;
#38802 = CARTESIAN_POINT ( 'NONE',  ( -5.177913976931291629, 64.41499993257284018, -5.372099999999999653 ) ) ;
#38803 = CARTESIAN_POINT ( 'NONE',  ( -3.257474687714740913, 31.88364938939399096, 0.8587021535642015424 ) ) ;
#38804 = CARTESIAN_POINT ( 'NONE',  ( 20.39340916383837055, 150.0074677946399504, 2.333577254436574044 ) ) ;
#38805 = CARTESIAN_POINT ( 'NONE',  ( -4.282102574861781363, 27.11529131024228434, -1.748715980913516876 ) ) ;
#38806 = CARTESIAN_POINT ( 'NONE',  ( 7.184910528696541121, -14.53812136005497280, -4.413989948622978332 ) ) ;
#38807 = CARTESIAN_POINT ( 'NONE',  ( -2.164707726640842544, 116.7454174419857935, -0.4974148364468519712 ) ) ;
#38808 = CARTESIAN_POINT ( 'NONE',  ( -1.507062556099493245, 116.9323294830472122, -1.352967057238088300 ) ) ;
#38809 = CARTESIAN_POINT ( 'NONE',  ( -23.29144772315980916, 149.3526176766912101, -0.4654185560736369132 ) ) ;
#38810 = CARTESIAN_POINT ( 'NONE',  ( 1.151906140154263847, 104.6144662015478843, 5.219791793463544494 ) ) ;
#38811 = CARTESIAN_POINT ( 'NONE',  ( -4.191205975170537279, 21.45845178295031630, -1.961646697876042511 ) ) ;
#38812 = CARTESIAN_POINT ( 'NONE',  ( -10.28897677580358305, 56.51499999999998636, -4.381499999999999950 ) ) ;
#38813 = PLANE ( 'NONE',  #32129 ) ;
#38814 = CARTESIAN_POINT ( 'NONE',  ( 3.197553254331486183, -13.99644925588092192, 2.254757065552156714 ) ) ;
#38815 = AXIS2_PLACEMENT_3D ( 'NONE', #7492, #33896, #20452 ) ;
#38816 = EDGE_CURVE ( 'NONE', #1088, #11005, #19381, .T. ) ;
#38817 = EDGE_CURVE ( 'NONE', #929, #10591, #30301, .T. ) ;
#38818 = CARTESIAN_POINT ( 'NONE',  ( 1.559908931542361099, 116.9323294830472122, -1.291681667928520794 ) ) ;
#38819 = CARTESIAN_POINT ( 'NONE',  ( -23.05353557640037820, 148.9204423966469335, 0.3945749818456248392 ) ) ;
#38820 = VERTEX_POINT ( 'NONE', #41347 ) ;
#38821 = CARTESIAN_POINT ( 'NONE',  ( 5.871452009091314039, 53.58606249999999704, 5.016499999999999737 ) ) ;
#38822 = ORIENTED_EDGE ( 'NONE', *, *, #5838, .T. ) ;
#38823 = CARTESIAN_POINT ( 'NONE',  ( -3.148524768479886937, 30.89467502894793327, -0.4672404312464801812 ) ) ;
#38824 = CARTESIAN_POINT ( 'NONE',  ( 5.741009826001572947, -15.03722989464144355, 1.207582410354154145 ) ) ;
#38825 = CARTESIAN_POINT ( 'NONE',  ( -0.03067001211942338088, 158.6015251912307633, 1.534852821454057770 ) ) ;
#38826 = CIRCLE ( 'NONE', #69, 0.2540000000000000591 ) ;
#38827 = CARTESIAN_POINT ( 'NONE',  ( 2.090077592200443313, 117.5043770775735510, -0.5427014567576282644 ) ) ;
#38828 = CARTESIAN_POINT ( 'NONE',  ( 4.586363120317823672, -1.655842793181455663, -0.6244342276643227718 ) ) ;
#38829 = CARTESIAN_POINT ( 'NONE',  ( -58.17934017679519343, 0.6739543484516548055, -1.160953350562855091 ) ) ;
#38830 = VERTEX_POINT ( 'NONE', #12149 ) ;
#38831 = CARTESIAN_POINT ( 'NONE',  ( -58.26714162322899426, -0.07371858623886340389, -0.4245910480433032763 ) ) ;
#38832 = CARTESIAN_POINT ( 'NONE',  ( 0.3558893179480882574, 120.1716774721349168, 0.6349178681961805681 ) ) ;
#38833 = B_SPLINE_SURFACE_WITH_KNOTS ( 'NONE', 1, 3, ( 
 ( #11402, #14380, #5041, #37189, #30994, #14799, #7811, #18201, #18413, #17996, #10990, #40195, #37810, #24389, #27389, #20773, #8211, #5453 ),
 ( #1835, #21598, #1423, #31202, #30584, #31420, #27802, #23972, #24595, #34626, #11194, #37394, #40810, #15010, #14588, #11611, #33797, #21183 ) ),
 .UNSPECIFIED., .F., .F., .F.,
 ( 2, 2 ),
 ( 4, 2, 2, 2, 2, 2, 2, 2, 4 ),
 ( 0.000000000000000000, 1.000000000000000000 ),
 ( 0.000000000000000000, 0.2500000000000000000, 0.5000000000000000000, 0.6250000000000000000, 0.7500000000000000000, 0.8125000000000000000, 0.8750000000000000000, 0.9375000000000000000, 1.000000000000000000 ),
 .UNSPECIFIED. ) ;
#38834 = CARTESIAN_POINT ( 'NONE',  ( -10.62684080304162393, 123.4307455932968765, 0.9978443992970126297 ) ) ;
#38835 = DIRECTION ( 'NONE',  ( -0.8745520943968251304, 0.4849315768086532863, -5.424246918827961050E-16 ) ) ;
#38836 = CARTESIAN_POINT ( 'NONE',  ( 11.99432760026347466, 123.0912118827050108, -1.285395851362399755 ) ) ;
#38837 = AXIS2_PLACEMENT_3D ( 'NONE', #252, #19392, #10025 ) ;
#38838 = CARTESIAN_POINT ( 'NONE',  ( -20.91256836843385614, 148.0559997909317644, -2.401931445155506939 ) ) ;
#38839 = CARTESIAN_POINT ( 'NONE',  ( -58.20820809768403592, 1.420579653404085985, -1.355822160094614759 ) ) ;
#38840 = EDGE_LOOP ( 'NONE', ( #5235, #35033, #4484, #41408, #11813, #31832, #5330, #33264, #8123, #24777, #25975, #18695 ) ) ;
#38841 = CARTESIAN_POINT ( 'NONE',  ( 4.459839028410091721, 118.1598638495170377, -0.4314496914423903151 ) ) ;
#38842 = CARTESIAN_POINT ( 'NONE',  ( 0.01133107913638646547, 156.3792106723807649, -0.5670535347366656431 ) ) ;
#38843 = ORIENTED_EDGE ( 'NONE', *, *, #5865, .F. ) ;
#38844 = CARTESIAN_POINT ( 'NONE',  ( -2.483060992037719572, 119.7126118883416410, -0.6995635895845424557 ) ) ;
#38845 = CARTESIAN_POINT ( 'NONE',  ( 3.489657270499090025, -15.47349394630789732, 3.491754635552897668 ) ) ;
#38846 = EDGE_CURVE ( 'NONE', #27765, #19376, #33875, .T. ) ;
#38847 = CARTESIAN_POINT ( 'NONE',  ( -6.591743005429100447E-14, 88.48546620154573361, -4.217761848057333172E-18 ) ) ;
#38848 = CARTESIAN_POINT ( 'NONE',  ( -4.865414317926856747, 117.7603977766165571, 0.7856990298424358921 ) ) ;
#38849 = CARTESIAN_POINT ( 'NONE',  ( 9.877803879600188353, 122.5082557396031291, 1.415055850893564449 ) ) ;
#38850 = CARTESIAN_POINT ( 'NONE',  ( -46.84426172109978381, 25.74287342672570844, 1.326046531035948828 ) ) ;
#38851 = CIRCLE ( 'NONE', #30034, 3.175000000000001155 ) ;
#38852 = CARTESIAN_POINT ( 'NONE',  ( 4.619096255015035624, 27.05588869245799089, -0.3994036469054788596 ) ) ;
#38853 = CARTESIAN_POINT ( 'NONE',  ( 5.992274430538982344, 155.3621521873626534, 0.2980204051088304884 ) ) ;
#38854 = CARTESIAN_POINT ( 'NONE',  ( -30.20416046766209917, 71.17241488000101413, 1.269999999999991580 ) ) ;
#38856 = ORIENTED_EDGE ( 'NONE', *, *, #15449, .T. ) ;
#38855 = CARTESIAN_POINT ( 'NONE',  ( -45.58494389689082738, 18.10922195552005221, -0.2974575429725926368 ) ) ;
#38857 = DIRECTION ( 'NONE',  ( 1.011795553208986377E-16, 1.000000000000000000, -0.000000000000000000 ) ) ;
#38858 = CIRCLE ( 'NONE', #36832, 5.080000000000006288 ) ;
#38859 = CARTESIAN_POINT ( 'NONE',  ( -47.07934102874912696, 22.98505637820354153, 3.579966862081923828 ) ) ;
#38860 = CARTESIAN_POINT ( 'NONE',  ( -52.68752125517421092, 11.69862226064154065, 4.201349328611278189 ) ) ;
#38861 = DIRECTION ( 'NONE',  ( 1.000000000000000000, 6.353134868986659519E-16, 0.000000000000000000 ) ) ;
#38862 = CARTESIAN_POINT ( 'NONE',  ( -5.241362157049125337, 65.30181249999996851, 5.310945289804168468 ) ) ;
#38863 = LINE ( 'NONE', #9674, #12375 ) ;
#38864 = CARTESIAN_POINT ( 'NONE',  ( -54.06930887699937216, 11.98206827348202808, 2.380698788532457311 ) ) ;
#38865 = CARTESIAN_POINT ( 'NONE',  ( -56.78650302187183740, 3.241477563879227475, 2.205756828360251109 ) ) ;
#38866 = CARTESIAN_POINT ( 'NONE',  ( -4.773421586889413426, 116.8420656028321218, 0.1264526730306987090 ) ) ;
#38867 = EDGE_LOOP ( 'NONE', ( #32337, #4959 ) ) ;
#38868 = CARTESIAN_POINT ( 'NONE',  ( -52.43464216547582879, 18.97776253636583732, -1.102323479587938957E-14 ) ) ;
#38869 = CARTESIAN_POINT ( 'NONE',  ( 6.015849376199521537, 121.4427344782352947, 0.04688609515921689230 ) ) ;
#38870 = ORIENTED_EDGE ( 'NONE', *, *, #37098, .T. ) ;
#38871 = CARTESIAN_POINT ( 'NONE',  ( 1.708365387639474431, 115.7028613512742226, -1.661208468116264214 ) ) ;
#38872 = CARTESIAN_POINT ( 'NONE',  ( -2.908234975202577122, 156.0868537499222839, -0.2102064236019247079 ) ) ;
#38873 = CARTESIAN_POINT ( 'NONE',  ( 4.359322289182287591, -14.87073230766630694, 4.862486896750754184 ) ) ;
#38874 = CARTESIAN_POINT ( 'NONE',  ( -1.249041419371764716, 159.0162744061759099, 1.301773431059132680 ) ) ;
#38875 = DIRECTION ( 'NONE',  ( 1.000000000000000000, -1.288607544181256449E-16, 0.000000000000000000 ) ) ;
#38876 = CARTESIAN_POINT ( 'NONE',  ( 22.96225337745231343, 150.1545470440437953, 0.6883021358963680170 ) ) ;
#38877 = CARTESIAN_POINT ( 'NONE',  ( 7.529841678698274698, 122.4254555285577339, 0.2702288470472028470 ) ) ;
#38878 = CARTESIAN_POINT ( 'NONE',  ( 5.275990361836075060, 115.6909491485453145, -0.8142983086533037707 ) ) ;
#38879 = CARTESIAN_POINT ( 'NONE',  ( 0.6724949529566155437, 16.91434809748496804, 0.7070771739444717818 ) ) ;
#38880 = CARTESIAN_POINT ( 'NONE',  ( -10.80923569951307250, 157.9177219752764358, -0.3353067243844871093 ) ) ;
#38881 = CARTESIAN_POINT ( 'NONE',  ( 5.078986093043053707, 78.83346620154574680, 0.1014902294541244060 ) ) ;
#38882 = EDGE_CURVE ( 'NONE', #29870, #4305, #8541, .T. ) ;
#38883 = LINE ( 'NONE', #29288, #3716 ) ;
#38884 = ORIENTED_EDGE ( 'NONE', *, *, #34679, .T. ) ;
#38885 = CARTESIAN_POINT ( 'NONE',  ( 8.512041645113450627, 118.9720402044547996, 1.274280440602515441 ) ) ;
#38886 = ORIENTED_EDGE ( 'NONE', *, *, #34929, .T. ) ;
#38887 = CARTESIAN_POINT ( 'NONE',  ( -58.36310612058592540, -0.2775539044676491041, -0.1022538777131802717 ) ) ;
#38888 = CARTESIAN_POINT ( 'NONE',  ( 7.089439975188524201, 158.1912585135832785, 1.657816039754273607 ) ) ;
#38889 = CARTESIAN_POINT ( 'NONE',  ( 12.64706598677940974, 155.2353133052689032, -1.715565181845534415 ) ) ;
#38890 = CARTESIAN_POINT ( 'NONE',  ( -5.321447747238043036, 7.245273219182337243, -6.556399146060885919 ) ) ;
#38891 = CARTESIAN_POINT ( 'NONE',  ( -5.844042411599879472, 117.9059190437751141, -0.9510131463654530881 ) ) ;
#38892 = CARTESIAN_POINT ( 'NONE',  ( 4.657082998918331107, 117.9833643526148705, -0.7124481076139314029 ) ) ;
#38893 = VECTOR ( 'NONE', #4363, 1000.000000000000000 ) ;
#38894 = DIRECTION ( 'NONE',  ( 0.9876665170007968841, -0.1565721916417935344, 5.390917751951443929E-16 ) ) ;
#38895 = CARTESIAN_POINT ( 'NONE',  ( -10.40273896401448006, 153.1126597504080280, -0.1617772828476136959 ) ) ;
#38896 = EDGE_CURVE ( 'NONE', #35057, #20737, #5153, .T. ) ;
#38897 = VERTEX_POINT ( 'NONE', #39184 ) ;
#38898 = CARTESIAN_POINT ( 'NONE',  ( -11.80606196054498369, 122.9427978038690270, -1.750206178813383584 ) ) ;
#38899 = CARTESIAN_POINT ( 'NONE',  ( 5.836094479182562189, -14.94293577981173371, 0.6207079514943552034 ) ) ;
#38900 = CIRCLE ( 'NONE', #33465, 0.5556250000000014788 ) ;
#38901 = FACE_OUTER_BOUND ( 'NONE', #38755, .T. ) ;
#38902 = CARTESIAN_POINT ( 'NONE',  ( -46.91604881613255174, 25.30076613767161220, -1.786867259277528985 ) ) ;
#38903 = VERTEX_POINT ( 'NONE', #9785 ) ;
#38904 = CARTESIAN_POINT ( 'NONE',  ( 1.339510839693822453, 119.4570717772418220, 0.6353817622545780974 ) ) ;
#38905 = ADVANCED_FACE ( 'NONE', ( #3198 ), #38767, .F. ) ;
#38906 = DIRECTION ( 'NONE',  ( 0.6594218222380214822, 0.7517731442105972661, 4.341145124518715900E-16 ) ) ;
#38907 = CARTESIAN_POINT ( 'NONE',  ( -5.705706447001241521, 123.8402959710505087, -0.07212015369193661152 ) ) ;
#38908 = EDGE_CURVE ( 'NONE', #5996, #18705, #3111, .T. ) ;
#38909 = CARTESIAN_POINT ( 'NONE',  ( -2.203247880972440065, 24.02835216854757405, 8.161197317184477384 ) ) ;
#38910 = CARTESIAN_POINT ( 'NONE',  ( 0.6802018490771016834, 156.3636429644085695, 0.5246204485115754101 ) ) ;
#38911 = CARTESIAN_POINT ( 'NONE',  ( 9.616121018674252952, 118.2964180356302961, -0.4479623223841151525 ) ) ;
#38912 = PLANE ( 'NONE',  #21264 ) ;
#38913 = CARTESIAN_POINT ( 'NONE',  ( -58.36919919733277595, -0.2903088519664511757, 0.02951549999211592473 ) ) ;
#38914 = AXIS2_PLACEMENT_3D ( 'NONE', #41177, #11981, #34784 ) ;
#38915 = B_SPLINE_CURVE_WITH_KNOTS ( 'NONE', 3,
 ( #29761, #13779, #37200, #5051, #34015, #4634, #4843, #18211, #31431, #21608, #27400, #20992, #17798, #1645, #38039, #5257, #18007, #14598, #27604, #31212, #11412, #37613, #41030, #34636, #24608, #30593, #30794, #21195 ),
 .UNSPECIFIED., .F., .F.,
 ( 4, 2, 2, 2, 2, 2, 2, 2, 2, 2, 2, 2, 2, 4 ),
 ( -6.000000002036711361E-08, 0.0002743568420867710956, 0.0005487736841735625431, 0.001097607368347123212, 0.001646441052520683773, 0.002195274736694244333, 0.003292942105041382368, 0.004390609473388520402, 0.005488276841735658003, 0.006585944210082795604, 0.007134777894256365272, 0.007683611578429934072, 0.008232445262603502872, 0.008781278946777071673 ),
 .UNSPECIFIED. ) ;
#38916 = UNCERTAINTY_MEASURE_WITH_UNIT (LENGTH_MEASURE( 1.000000000000000082E-05 ), #19777, 'distance_accuracy_value', 'NONE');
#38917 = CARTESIAN_POINT ( 'NONE',  ( -23.11179153581203494, 149.9001102426712748, -0.4361622115260938015 ) ) ;
#38918 = EDGE_CURVE ( 'NONE', #9144, #31688, #26897, .T. ) ;
#38919 = ORIENTED_EDGE ( 'NONE', *, *, #7643, .T. ) ;
#38920 = CARTESIAN_POINT ( 'NONE',  ( 4.403632403658274796, 119.4899321720584737, -0.7529549363037313370 ) ) ;
#38921 = LINE ( 'NONE', #13138, #18975 ) ;
#38922 = CARTESIAN_POINT ( 'NONE',  ( -3.666883307181661777, 120.9289264519876070, -0.3209655359951389952 ) ) ;
#38923 = CARTESIAN_POINT ( 'NONE',  ( 4.087908758852305091, -13.37781719547838399, 3.422002167429263331 ) ) ;
#38924 = DIRECTION ( 'NONE',  ( -5.188838149069471174E-16, 1.699382548006136313E-16, 1.000000000000000000 ) ) ;
#38925 = CARTESIAN_POINT ( 'NONE',  ( 22.53527615164620101, 150.7831677823008363, 0.4503084484864737225 ) ) ;
#38926 = EDGE_LOOP ( 'NONE', ( #25021, #23362, #34918, #21386 ) ) ;
#38927 = CARTESIAN_POINT ( 'NONE',  ( -2.136650056307613621, 10.86338872207680950, -4.114640003288728920 ) ) ;
#38928 = CARTESIAN_POINT ( 'NONE',  ( 5.332935397695205637, 105.1224662015457199, 0.1065647409268305201 ) ) ;
#38929 = CARTESIAN_POINT ( 'NONE',  ( -3.302029177305334073, 159.4671159221996959, -0.06598240135525369754 ) ) ;
#38930 = DIRECTION ( 'NONE',  ( -0.8745520943968236871, 0.4849315768086559508, -6.829619984160659032E-16 ) ) ;
#38931 = CARTESIAN_POINT ( 'NONE',  ( 6.875583424705200564, 120.7192244753876338, 1.121239711753028168 ) ) ;
#38932 = CIRCLE ( 'NONE', #30082, 3.683000000000001162 ) ;
#38933 = CARTESIAN_POINT ( 'NONE',  ( 4.198131962423935271, 12.64715247731088787, 1.959332076845688553 ) ) ;
#38934 = CARTESIAN_POINT ( 'NONE',  ( 19.15327062675849135, 128.6826163344482268, 1.506695251711823058 ) ) ;
#38936 = CARTESIAN_POINT ( 'NONE',  ( 14.04756362465202280, 122.1591959312462592, -1.132115996748545239 ) ) ;
#38935 = CARTESIAN_POINT ( 'NONE',  ( 5.256666790930580646, 56.51499999999976609, 5.296388420400072405 ) ) ;
#38937 = CARTESIAN_POINT ( 'NONE',  ( -2.972019672840211513, 9.848453565018933986, 3.538668892428941781 ) ) ;
#38938 = CARTESIAN_POINT ( 'NONE',  ( -22.03992273305667382, 150.6352520364973486, -1.509874617927602802 ) ) ;
#38939 = ORIENTED_EDGE ( 'NONE', *, *, #12282, .T. ) ;
#38940 = EDGE_CURVE ( 'NONE', #33497, #27131, #18947, .T. ) ;
#38941 = EDGE_CURVE ( 'NONE', #11376, #35682, #35359, .T. ) ;
#38942 = CARTESIAN_POINT ( 'NONE',  ( -0.003052472355933761282, 120.8426702770480148, 0.1527581987772201888 ) ) ;
#38943 = CARTESIAN_POINT ( 'NONE',  ( 2.663994046441380270, -15.36521416583532051, 5.826768514169494040 ) ) ;
#38944 = FACE_OUTER_BOUND ( 'NONE', #37107, .T. ) ;
#38945 = VECTOR ( 'NONE', #41829, 1000.000000000000000 ) ;
#38946 = ORIENTED_EDGE ( 'NONE', *, *, #39889, .F. ) ;
#38947 = CARTESIAN_POINT ( 'NONE',  ( 19.27109647334602016, 148.6897983921382433, 2.507318192549734981 ) ) ;
#38948 = CARTESIAN_POINT ( 'NONE',  ( 4.792324638247207780, 56.51998046905276141, 4.972049999977001811 ) ) ;
#38949 = CYLINDRICAL_SURFACE ( 'NONE', #13004, 0.6350000000000006750 ) ;
#38950 = CARTESIAN_POINT ( 'NONE',  ( -17.79905452297358437, 125.1550653296939970, 0.5857557929999464008 ) ) ;
#38951 = EDGE_CURVE ( 'NONE', #19534, #24265, #39128, .T. ) ;
#38952 = MANIFOLD_SOLID_BREP ( 'Stock-MAS-162-1', #33294 ) ;
#38953 = AXIS2_PLACEMENT_3D ( 'NONE', #35446, #35241, #15416 ) ;
#38954 = CARTESIAN_POINT ( 'NONE',  ( 9.710933996004669666, 118.1218853900603136, -0.2424195399123781347 ) ) ;
#38955 = CARTESIAN_POINT ( 'NONE',  ( -5.860279866549801042, 57.14999999999999147, -5.019549989156839587 ) ) ;
#38956 = DIRECTION ( 'NONE',  ( -6.353134868986659519E-16, 1.000000000000000000, -0.000000000000000000 ) ) ;
#38957 = CARTESIAN_POINT ( 'NONE',  ( -46.91604881613258016, 25.30076613767155180, 1.786867259277509001 ) ) ;
#38958 = CARTESIAN_POINT ( 'NONE',  ( 1.913223137500898341, -15.30302091211069282, 5.362660726125270116 ) ) ;
#38959 = CARTESIAN_POINT ( 'NONE',  ( -47.19936399096372526, 20.24790404726484283, 5.251082349106850344 ) ) ;
#38960 = DIRECTION ( 'NONE',  ( 4.017660918040594346E-17, -1.000000000000000000, -2.376309959284832031E-19 ) ) ;
#38961 = CARTESIAN_POINT ( 'NONE',  ( -4.523630674469822033, 118.0850806367477190, 0.6137328214149938566 ) ) ;
#38962 = CARTESIAN_POINT ( 'NONE',  ( -58.37241122568488549, -0.2962816677227891882, -1.031899547879545818E-14 ) ) ;
#38963 = ORIENTED_EDGE ( 'NONE', *, *, #5566, .T. ) ;
#38964 = ORIENTED_EDGE ( 'NONE', *, *, #35338, .T. ) ;
#38965 = CARTESIAN_POINT ( 'NONE',  ( 5.078986093043053707, 88.48546620154573361, 0.1014902294541237954 ) ) ;
#38966 = CARTESIAN_POINT ( 'NONE',  ( -8.360168168866218608, 119.6977264182660576, -1.427561477091477737 ) ) ;
#38967 = CARTESIAN_POINT ( 'NONE',  ( -5.451337559846766823, 117.5214873295501405, -0.8265904065678291168 ) ) ;
#38968 = CARTESIAN_POINT ( 'NONE',  ( 4.670575340268697140, 117.8934551130230517, 0.9881073750738181838 ) ) ;
#38969 = LINE ( 'NONE', #15323, #6657 ) ;
#38970 = CARTESIAN_POINT ( 'NONE',  ( -8.439375761976453560, 122.5794309061019618, -0.8715591655942094285 ) ) ;
#38971 = VECTOR ( 'NONE', #14546, 1000.000000000000000 ) ;
#38972 = CARTESIAN_POINT ( 'NONE',  ( -2.413257664290607618, 115.7029552727873352, -1.699853810109273278 ) ) ;
#38973 = CARTESIAN_POINT ( 'NONE',  ( -8.095114962461808616, 74.19100168833409725, 1.524000000000002686 ) ) ;
#38974 = CARTESIAN_POINT ( 'NONE',  ( -4.854186777038641765, 117.7557277303023966, -0.9091791526384296329 ) ) ;
#38975 = CARTESIAN_POINT ( 'NONE',  ( 6.719914377343970457, 121.2247800624193133, -0.07397671124164055534 ) ) ;
#38976 = CARTESIAN_POINT ( 'NONE',  ( -11.93440950959111291, 126.0992317015783328, -1.505959514896210605 ) ) ;
#38977 = CARTESIAN_POINT ( 'NONE',  ( 23.45208337669092913, 146.8499405025503961, 0.4686284387228002446 ) ) ;
#38978 = CARTESIAN_POINT ( 'NONE',  ( -0.03212616895158381530, 157.6269964811067155, 1.607724863813389415 ) ) ;
#38979 = CARTESIAN_POINT ( 'NONE',  ( -19.68500000000000938, 71.11999999999999034, -5.080000000000000959 ) ) ;
#38980 = CARTESIAN_POINT ( 'NONE',  ( -8.012499360674619098, 122.8488795790854766, -0.07767969516895584237 ) ) ;
#38981 = CARTESIAN_POINT ( 'NONE',  ( 3.745621265272091716, -10.50169880513956322, -2.708184146228840294 ) ) ;
#38983 = EDGE_LOOP ( 'NONE', ( #18255, #12068, #1444, #3126 ) ) ;
#38982 = CARTESIAN_POINT ( 'NONE',  ( 18.16683071450844267, 125.1529741258727597, 1.044517495177846422 ) ) ;
#38984 = DIRECTION ( 'NONE',  ( 0.8745520943968235761, -0.4849315768086558398, 4.268512490100410909E-16 ) ) ;
#38985 = CARTESIAN_POINT ( 'NONE',  ( 2.381491173306826248, -15.37068253093559811, 4.932168965620852497 ) ) ;
#38986 = CARTESIAN_POINT ( 'NONE',  ( -2.404146712672539099, 157.7073581658784178, 1.626633079703769358 ) ) ;
#38987 = CARTESIAN_POINT ( 'NONE',  ( 0.2616662591921395387, 4.880059721033824793, -0.9399936778652994152 ) ) ;
#38988 = CARTESIAN_POINT ( 'NONE',  ( -16.79208607122050978, 122.6968688451475771, -0.8807046615161948644 ) ) ;
#38989 = TOROIDAL_SURFACE ( 'NONE', #20590, 0.7620000000000000107, 0.2540000000000000036 ) ;
#38990 = CARTESIAN_POINT ( 'NONE',  ( 0.3959014520675726012, 0.7218480974852773402, -0.8918910426260873159 ) ) ;
#38991 = EDGE_LOOP ( 'NONE', ( #36315, #18110, #596, #5509 ) ) ;
#38992 = ORIENTED_EDGE ( 'NONE', *, *, #23345, .F. ) ;
#38993 = CARTESIAN_POINT ( 'NONE',  ( -41.38112080847943020, 22.74200708568027807, 0.4658591655018960442 ) ) ;
#38994 = CARTESIAN_POINT ( 'NONE',  ( 6.868335724905528572, 121.8312213470058225, 0.2935230024867369059 ) ) ;
#38995 =( LENGTH_UNIT ( ) NAMED_UNIT ( * ) SI_UNIT ( .MILLI., .METRE. ) );
#38996 = CARTESIAN_POINT ( 'NONE',  ( -6.503815726752127269, 121.4942169270607053, 0.3795357812798489383 ) ) ;
#38997 = CARTESIAN_POINT ( 'NONE',  ( 4.031918519141627577, -13.48391852982397410, 3.589295450856327729 ) ) ;
#38998 = CARTESIAN_POINT ( 'NONE',  ( 10.18365381109002854, 122.2967958330617648, -1.106735498401915763 ) ) ;
#38999 = CARTESIAN_POINT ( 'NONE',  ( -12.54651694896177538, 122.2722385251898771, -1.803108555445325223 ) ) ;
#39000 = CARTESIAN_POINT ( 'NONE',  ( -6.650126595083637682, 78.47834120613788400, -1.269999999999996687 ) ) ;
#39001 = CARTESIAN_POINT ( 'NONE',  ( 2.857130780617909149, -14.87311083204414786, 4.269097905712053276 ) ) ;
#39002 = CARTESIAN_POINT ( 'NONE',  ( -1.091745343399155299, 36.70702312047181692, 0.5241475151901328067 ) ) ;
#39003 = CARTESIAN_POINT ( 'NONE',  ( 13.67682410656400727, 150.2105054413494543, -0.1652630162413759318 ) ) ;
#39004 = EDGE_LOOP ( 'NONE', ( #19304, #22218, #13511, #40294 ) ) ;
#39005 = DIRECTION ( 'NONE',  ( -5.188838149069471174E-16, 1.699382548006136313E-16, 1.000000000000000000 ) ) ;
#39006 = CIRCLE ( 'NONE', #39687, 16.60960244842765832 ) ;
#39007 = CARTESIAN_POINT ( 'NONE',  ( -23.21760062652228029, 78.26400813401573942, -1.270000000000004903 ) ) ;
#39008 = CARTESIAN_POINT ( 'NONE',  ( -58.78565887484231212, -0.2971860671465154091, 0.1726678976671059684 ) ) ;
#39009 = AXIS2_PLACEMENT_3D ( 'NONE', #2289, #40837, #1450 ) ;
#39010 = CARTESIAN_POINT ( 'NONE',  ( -6.376221727585796537E-14, 51.14746620154573264, 5.777789833161707559E-29 ) ) ;
#39011 = CARTESIAN_POINT ( 'NONE',  ( 18.76910502294225225, 125.2887878443791294, 0.2589991215523650414 ) ) ;
#39012 = CARTESIAN_POINT ( 'NONE',  ( -5.222556791543373045, 115.4535745449993982, 1.305545271932168960 ) ) ;
#39013 = CIRCLE ( 'NONE', #24705, 5.080000000000006288 ) ;
#39014 = DIRECTION ( 'NONE',  ( 4.017660918040594346E-17, -1.000000000000000000, -2.376309959284834438E-19 ) ) ;
#39015 = DIRECTION ( 'NONE',  ( -0.000000000000000000, -1.000000000000000000, -0.000000000000000000 ) ) ;
#39016 = CARTESIAN_POINT ( 'NONE',  ( -3.738651510184325399, 31.35217495388765840, -0.6318812681667338449 ) ) ;
#39017 = CARTESIAN_POINT ( 'NONE',  ( 20.82206258336668014, 149.3152741295656369, 2.348048710389011973 ) ) ;
#39018 = CARTESIAN_POINT ( 'NONE',  ( 1.391598188199559161, 15.24595356501894017, -4.406646451508545503 ) ) ;
#39019 = CARTESIAN_POINT ( 'NONE',  ( -7.004517537292900720, 30.72436916340981838, -4.697416855195242213 ) ) ;
#39020 = CARTESIAN_POINT ( 'NONE',  ( 2.192952236640623109, 116.7858836396481053, -0.4274597272194167741 ) ) ;
#39021 = CARTESIAN_POINT ( 'NONE',  ( -0.9980778803428626000, 110.6314368487224300, -3.458106935563855622 ) ) ;
#39022 = LINE ( 'NONE', #10039, #16206 ) ;
#39023 = FACE_OUTER_BOUND ( 'NONE', #4151, .T. ) ;
#39024 = CARTESIAN_POINT ( 'NONE',  ( -0.8468149500948856101, 104.6144662015456390, 4.761320281557485323 ) ) ;
#39025 = CARTESIAN_POINT ( 'NONE',  ( -3.453265078539333288, 21.00871511114837276, -3.102408547967784092 ) ) ;
#39026 = CARTESIAN_POINT ( 'NONE',  ( -4.757248700628498916, 117.4032733054477973, -1.206458840162573543 ) ) ;
#39027 = CARTESIAN_POINT ( 'NONE',  ( 0.02983097946976470335, 117.3993836135854707, -1.492864285907033572 ) ) ;
#39028 = CARTESIAN_POINT ( 'NONE',  ( 3.212496809824684441, -14.25148094350509353, 2.370051959060230473 ) ) ;
#39029 = CARTESIAN_POINT ( 'NONE',  ( 1.272828668259097462, 111.9985432423065959, -2.911558293332169089 ) ) ;
#39030 = CARTESIAN_POINT ( 'NONE',  ( -3.845766519666914629, 116.9593488885201538, 0.3368132424836106087 ) ) ;
#39031 = ORIENTED_EDGE ( 'NONE', *, *, #6916, .T. ) ;
#39032 = CARTESIAN_POINT ( 'NONE',  ( 5.241362157049057835, 53.58606249999999704, 5.310945289804168468 ) ) ;
#39033 = ORIENTED_EDGE ( 'NONE', *, *, #29256, .T. ) ;
#39034 = CARTESIAN_POINT ( 'NONE',  ( 2.912792906754999134, 38.59631781016217644, -1.173005823891349220 ) ) ;
#39035 = CIRCLE ( 'NONE', #6370, 0.7620000000000000107 ) ;
#39036 = CARTESIAN_POINT ( 'NONE',  ( 2.040901337265842663, -15.69771917786945359, 5.688463219523050896 ) ) ;
#39037 = CARTESIAN_POINT ( 'NONE',  ( -12.70950188986288154, 122.0451665396574725, 1.271450951352564251 ) ) ;
#39038 = CARTESIAN_POINT ( 'NONE',  ( 13.26523119301593212, 121.0513591912305316, -0.9938426049807239648 ) ) ;
#39039 = CARTESIAN_POINT ( 'NONE',  ( 4.627880361116947228, 7.839802885307131319, -0.3238752845059330032 ) ) ;
#39040 = CARTESIAN_POINT ( 'NONE',  ( -58.67480324322914953, -0.3139011383600042726, -0.3141419669791276625 ) ) ;
#39041 = ORIENTED_EDGE ( 'NONE', *, *, #20706, .F. ) ;
#39042 = CARTESIAN_POINT ( 'NONE',  ( -4.394136353581303389, 70.68697878297604120, -1.523999999999994026 ) ) ;
#39043 = CARTESIAN_POINT ( 'NONE',  ( -0.07157677170311223247, 110.3683645023726569, 3.581994345755902032 ) ) ;
#39044 = CIRCLE ( 'NONE', #13183, 0.2539999999999978386 ) ;
#39045 = CARTESIAN_POINT ( 'NONE',  ( -15.43236126668712949, 134.8939017613128328, 1.443262610673741397 ) ) ;
#39046 = CARTESIAN_POINT ( 'NONE',  ( 4.808131379915038472, 105.1224662015457625, -0.4149153341867673483 ) ) ;
#39047 = CARTESIAN_POINT ( 'NONE',  ( 0.01111639999511693754, 119.1634951276629550, -0.5563101126475827884 ) ) ;
#39048 = CARTESIAN_POINT ( 'NONE',  ( -9.041969115052843620, 119.3941581119689204, -1.378656440977003239 ) ) ;
#39049 = CARTESIAN_POINT ( 'NONE',  ( -57.53497731650991653, 2.247686704661286505, -1.882970859819768306 ) ) ;
#39050 = CIRCLE ( 'NONE', #2990, 0.7620000000000000107 ) ;
#39051 = ORIENTED_EDGE ( 'NONE', *, *, #23543, .T. ) ;
#39052 = CARTESIAN_POINT ( 'NONE',  ( 4.431862760627758746, 118.1653681970028913, -0.4638930779344027089 ) ) ;
#39053 = CARTESIAN_POINT ( 'NONE',  ( 6.498933901768258359, 121.5572409441427482, -0.3210307352789208979 ) ) ;
#39054 = ORIENTED_EDGE ( 'NONE', *, *, #38324, .T. ) ;
#39055 = CARTESIAN_POINT ( 'NONE',  ( -5.074328365123786710, 120.0747842884402132, -0.9638994778299827537 ) ) ;
#39056 = CARTESIAN_POINT ( 'NONE',  ( 3.395721326281507579, -14.88725931823228699, 0.4187095049187871121 ) ) ;
#39057 = TOROIDAL_SURFACE ( 'NONE', #13870, 5.080000000000005400, 0.5080000000000000071 ) ;
#39058 = TOROIDAL_SURFACE ( 'NONE', #37023, 0.7620000000000000107, 0.2540000000000000036 ) ;
#39059 = CARTESIAN_POINT ( 'NONE',  ( -0.8462821048516611100, 105.1230362821993083, -5.276608005300069237 ) ) ;
#39060 = B_SPLINE_CURVE_WITH_KNOTS ( 'NONE', 3,
 ( #6594, #32793, #22961, #19563, #29159, #19153, #3624, #26176, #16372, #16589, #41966, #38554, #32158, #2991, #32572, #41762, #9367, #3404, #29597, #19358, #38762, #3192, #430, #12562, #9573, #13401, #36203, #38972, #5, #29377, #22331, #217, #32364, #12971, #35571, #25964, #13192, #26390, #23169, #15952, #39396, #6184, #7025, #13822, #26820, #27235, #40458, #30634, #36418, #30009, #39827, #10621, #7444, #23603, #1058, #27443, #23386, #14228, #10415, #40038, #36624, #1478, #33642, #39610, #848, #30218, #17009, #7236, #20402, #17426, #29805, #7861, #24027, #33431, #4259, #20196, #20611, #20822, #11248, #40250, #23813, #30424, #17222, #1271, #14022 ),
 .UNSPECIFIED., .F., .F.,
 ( 4, 2, 2, 1, 1, 1, 1, 2, 2, 2, 1, 2, 2, 2, 2, 1, 1, 1, 2, 2, 2, 2, 1, 1, 1, 1, 2, 2, 2, 2, 1, 1, 2, 2, 2, 2, 2, 2, 2, 2, 2, 2, 2, 1, 2, 2, 2, 2, 2, 4 ),
 ( 0.000000000000000000, 0.1250000000000058842, 0.1875000000000088263, 0.2187500000000101308, 0.2343750000000107692, 0.2421875000000111300, 0.2460937500000114631, 0.2480468750000118794, 0.2500000000000122680, 0.3125000000000180411, 0.3437500000000208167, 0.3593750000000222045, 0.3750000000000235922, 0.4375000000000284772, 0.4687500000000308087, 0.4843750000000319189, 0.4921875000000324740, 0.4960937500000326961, 0.4980468750000327516, 0.5000000000000328626, 0.5625000000000327516, 0.5937500000000326406, 0.6093750000000326406, 0.6171875000000326406, 0.6210937500000325295, 0.6230468750000324185, 0.6240234375000324185, 0.6250000000000323075, 0.6875000000000266454, 0.7187500000000239808, 0.7343750000000224265, 0.7421875000000216493, 0.7460937500000212053, 0.7500000000000208722, 0.7812500000000180966, 0.7968750000000167644, 0.8125000000000153211, 0.8281250000000139888, 0.8359375000000132117, 0.8398437500000129896, 0.8437500000000127676, 0.8593750000000114353, 0.8671875000000108802, 0.8710937500000104361, 0.8730468750000103251, 0.8750000000000102141, 0.9062500000000076605, 0.9218750000000064393, 0.9375000000000051070, 1.000000000000000000 ),
 .UNSPECIFIED. ) ;
#39061 = CARTESIAN_POINT ( 'NONE',  ( -50.84949806483948720, 11.71728973011883923, -8.857595425233459675E-15 ) ) ;
#39062 = CARTESIAN_POINT ( 'NONE',  ( -4.869611397611841141, 117.6445991000119022, 0.8937056924343703690 ) ) ;
#39063 = CARTESIAN_POINT ( 'NONE',  ( 8.888678185456905467, 122.0520977060996586, 1.259005013942402940 ) ) ;
#39064 = CARTESIAN_POINT ( 'NONE',  ( -8.584304875092012566, 68.18838345945393087, -1.523999999999995802 ) ) ;
#39065 = AXIS2_PLACEMENT_3D ( 'NONE', #35272, #19687, #36118 ) ;
#39066 = CARTESIAN_POINT ( 'NONE',  ( 4.496586626007489151, 27.28078351817337222, -1.068494511273165193 ) ) ;
#39067 = CARTESIAN_POINT ( 'NONE',  ( 8.997762725187955724, 123.9218113011205986, 0.2640260769295986187 ) ) ;
#39068 = LINE ( 'NONE', #19032, #7269 ) ;
#39069 = CARTESIAN_POINT ( 'NONE',  ( -50.02669608763528686, 12.78473261814649931, -8.449425852006687485E-15 ) ) ;
#39070 = CARTESIAN_POINT ( 'NONE',  ( 5.563856532153242718, 116.6986126813221034, 0.08223999505859086456 ) ) ;
#39071 = DIRECTION ( 'NONE',  ( -0.000000000000000000, -0.000000000000000000, -1.000000000000000000 ) ) ;
#39072 = CARTESIAN_POINT ( 'NONE',  ( -46.74873316577708238, 25.87611666761727847, -1.399911675830463054 ) ) ;
#39073 = DIRECTION ( 'NONE',  ( -0.8745520943968243532, 0.4849315768086547296, -5.361993529360573944E-16 ) ) ;
#39074 = DIRECTION ( 'NONE',  ( 0.9876665170007972172, -0.1565721916417913695, -6.288420277261245215E-16 ) ) ;
#39075 = CARTESIAN_POINT ( 'NONE',  ( -5.664977208693910526, 88.73331249999998249, 5.033228321271210781 ) ) ;
#39076 = CARTESIAN_POINT ( 'NONE',  ( -4.074955089416341991, 118.2429491485453354, 0.1454234154749719787 ) ) ;
#39077 = LINE ( 'NONE', #39286, #19827 ) ;
#39078 = CARTESIAN_POINT ( 'NONE',  ( -57.36672490206960617, 3.909939030509804070, 0.6468086288197671951 ) ) ;
#39079 = CARTESIAN_POINT ( 'NONE',  ( -58.11258158571958177, 1.603013069906233934, 1.501710181103012465 ) ) ;
#39080 = CARTESIAN_POINT ( 'NONE',  ( -1.411700740068628779, 159.5982469381528972, 0.1593474270858734332 ) ) ;
#39081 = ORIENTED_EDGE ( 'NONE', *, *, #15398, .T. ) ;
#39082 = CARTESIAN_POINT ( 'NONE',  ( -49.81807968324856972, 18.07223176367294570, -4.612844822355063990 ) ) ;
#39083 = CARTESIAN_POINT ( 'NONE',  ( -6.977722893427367623, 121.9489747943516420, -0.1966404063935860980 ) ) ;
#39084 = ORIENTED_EDGE ( 'NONE', *, *, #14633, .F. ) ;
#39085 = CARTESIAN_POINT ( 'NONE',  ( -5.326630349062241088, 115.7029491485453718, -0.4164715811699009618 ) ) ;
#39086 = CARTESIAN_POINT ( 'NONE',  ( -14.23422759389739944, 138.9464670490549452, -0.5149110934774580040 ) ) ;
#39087 = CARTESIAN_POINT ( 'NONE',  ( 5.341071565670632459, -14.32387631201759248, 3.633538872802142716 ) ) ;
#39088 = CARTESIAN_POINT ( 'NONE',  ( -4.934953413367899167, 117.8999350694477926, 0.7268823312289468541 ) ) ;
#39089 = CARTESIAN_POINT ( 'NONE',  ( -5.144468029576237278, 116.8626782701987565, -0.2538742916674817662 ) ) ;
#39090 = CARTESIAN_POINT ( 'NONE',  ( 1.872007501980861299, 116.6503132507590124, 0.2654151457657344393 ) ) ;
#39091 = CARTESIAN_POINT ( 'NONE',  ( 13.58790511794221523, 150.2605122904624011, 0.4013236421570368084 ) ) ;
#39092 = DIRECTION ( 'NONE',  ( -0.6878275643654763183, -0.7258741224889179167, -2.335488090154185488E-16 ) ) ;
#39093 = CARTESIAN_POINT ( 'NONE',  ( -0.1566604602083998543, 5.914057227930348049, 0.9647682902456425902 ) ) ;
#39094 = CARTESIAN_POINT ( 'NONE',  ( -23.26558566580239784, 149.3390083238215595, -0.6953334291057010619 ) ) ;
#39095 = CARTESIAN_POINT ( 'NONE',  ( -47.85244527695891037, 19.39403540832952544, -5.219971639306605127 ) ) ;
#39096 = CARTESIAN_POINT ( 'NONE',  ( -0.02983097946891718685, 117.3993836135855418, 1.492864285907047561 ) ) ;
#39097 = ORIENTED_EDGE ( 'NONE', *, *, #36141, .F. ) ;
#39098 = CARTESIAN_POINT ( 'NONE',  ( -2.526976701386534963, 116.7749708623049401, 0.4200550213075466832 ) ) ;
#39099 = EDGE_LOOP ( 'NONE', ( #39799, #34166, #2763, #20779 ) ) ;
#39100 = CARTESIAN_POINT ( 'NONE',  ( -58.34256328868874419, -0.2344693364347718856, -0.2069899249132446384 ) ) ;
#39101 = CARTESIAN_POINT ( 'NONE',  ( 15.17292428814148764, 123.1171956318823533, 1.668999667383225471 ) ) ;
#39102 = CARTESIAN_POINT ( 'NONE',  ( 13.14453721617477733, 122.4605402651681487, -1.292199650740640138 ) ) ;
#39103 = CARTESIAN_POINT ( 'NONE',  ( 0.8080343152487895475, 3.801264818822497560, -0.5430376807499140979 ) ) ;
#39104 = CARTESIAN_POINT ( 'NONE',  ( -7.252988161461171757, 9.422892264050933164, 4.294140714350721311 ) ) ;
#39105 = CARTESIAN_POINT ( 'NONE',  ( -1.070729637574143522, 117.4935207075373569, -0.5386181289574427655 ) ) ;
#39106 = CARTESIAN_POINT ( 'NONE',  ( 4.892581560886663183, 117.7439198456695664, -0.7245015596533974644 ) ) ;
#39107 = CARTESIAN_POINT ( 'NONE',  ( 4.762298162519684297, 112.7561542417671916, 2.571201254457596175 ) ) ;
#39108 = CARTESIAN_POINT ( 'NONE',  ( 14.75676393591414026, 134.6798445586954927, -1.238239479614487770 ) ) ;
#39109 = CARTESIAN_POINT ( 'NONE',  ( -0.6477285649444898263, 156.3042436901572216, 0.05974520555407247802 ) ) ;
#39110 = ORIENTED_EDGE ( 'NONE', *, *, #26623, .F. ) ;
#39111 = CARTESIAN_POINT ( 'NONE',  ( -7.823018779267129297, 156.2605297791399437, -2.010767698085225152 ) ) ;
#39112 = CARTESIAN_POINT ( 'NONE',  ( 6.083905389560601229, -14.65912421694762280, 0.09720023197589457153 ) ) ;
#39113 = FACE_OUTER_BOUND ( 'NONE', #13034, .T. ) ;
#39114 = EDGE_CURVE ( 'NONE', #37003, #28325, #15052, .T. ) ;
#39115 = CARTESIAN_POINT ( 'NONE',  ( -46.30033180095409051, 21.65562830348028456, -4.292083522273610008 ) ) ;
#39116 = ORIENTED_EDGE ( 'NONE', *, *, #9741, .T. ) ;
#39117 = CARTESIAN_POINT ( 'NONE',  ( 5.835067757121013443, 120.0568572605186546, 1.100767069290504940 ) ) ;
#39118 = DIRECTION ( 'NONE',  ( -4.017660918040594346E-17, 1.000000000000000000, 2.376309959284834438E-19 ) ) ;
#39119 = CARTESIAN_POINT ( 'NONE',  ( -7.213960532363670630, 78.77618639008812806, 1.904999999999999583 ) ) ;
#39120 = CARTESIAN_POINT ( 'NONE',  ( -3.173429932895099448, 117.8122656274855871, 0.8370585861429157282 ) ) ;
#39121 = CARTESIAN_POINT ( 'NONE',  ( 2.561087359964590249, 24.90515699240134495, 8.022552078460996938 ) ) ;
#39122 = CARTESIAN_POINT ( 'NONE',  ( 15.44906575790727921, 148.0679034673509875, 1.029643479621237478 ) ) ;
#39123 = EDGE_CURVE ( 'NONE', #21058, #31705, #39992, .T. ) ;
#39124 = CARTESIAN_POINT ( 'NONE',  ( 6.906891541952338009, 117.5897289630162987, -0.4768185843253516798 ) ) ;
#39125 = CARTESIAN_POINT ( 'NONE',  ( -47.32981077577592544, 19.92739019301280834, -5.119713631627043959 ) ) ;
#39126 = FACE_OUTER_BOUND ( 'NONE', #32979, .T. ) ;
#39127 = CARTESIAN_POINT ( 'NONE',  ( -0.2965531742116714331, 116.4333835968663919, 0.03207532894271102747 ) ) ;
#39128 = CIRCLE ( 'NONE', #27570, 18.00660244842765323 ) ;
#39129 = ORIENTED_EDGE ( 'NONE', *, *, #14633, .T. ) ;
#39130 = CARTESIAN_POINT ( 'NONE',  ( -5.130992841088942491, 120.2796509446399398, -0.8476419795031335802 ) ) ;
#39131 = CARTESIAN_POINT ( 'NONE',  ( 4.536516067734830848, -15.04041621514964255, 4.646661483318791142 ) ) ;
#39132 = CARTESIAN_POINT ( 'NONE',  ( -0.6142257358153485614, 120.7813932625355307, -0.2072529566615756436 ) ) ;
#39133 = CARTESIAN_POINT ( 'NONE',  ( 4.057314763829551474, -13.83595378911055285, 4.182047561617943110 ) ) ;
#39134 = CARTESIAN_POINT ( 'NONE',  ( -6.540718711769984318E-14, 75.78546620154573077, -7.235675496349066572E-18 ) ) ;
#39135 = CARTESIAN_POINT ( 'NONE',  ( 16.30293663320032849, 121.4145675751456253, 0.3429698291441256042 ) ) ;
#39136 = ORIENTED_EDGE ( 'NONE', *, *, #458, .T. ) ;
#39137 = CARTESIAN_POINT ( 'NONE',  ( -4.550674770548566173, 2.667180226961371137, -0.8080508602523945871 ) ) ;
#39138 = ADVANCED_FACE ( 'NONE', ( #33014 ), #41168, .F. ) ;
#39139 = CARTESIAN_POINT ( 'NONE',  ( 2.445891218400001232, 105.1244718176544524, 4.749792414014113895 ) ) ;
#39140 = FACE_OUTER_BOUND ( 'NONE', #74, .T. ) ;
#39141 = CARTESIAN_POINT ( 'NONE',  ( 5.237379388564934679, 115.7029491485453292, 1.024072862575109655 ) ) ;
#39142 = CARTESIAN_POINT ( 'NONE',  ( -7.002513491937036427, 121.1574795575269263, 0.7090189476666535207 ) ) ;
#39143 = EDGE_CURVE ( 'NONE', #29332, #7253, #4454, .T. ) ;
#39144 = CARTESIAN_POINT ( 'NONE',  ( 2.551181839206869917, 14.82117702134586779, -3.857898856385788999 ) ) ;
#39145 = CARTESIAN_POINT ( 'NONE',  ( 6.873244579178494185, 117.6856483911789581, 0.8154597436780149922 ) ) ;
#39146 = CARTESIAN_POINT ( 'NONE',  ( -15.47023807670837314, 120.6682698389898434, -0.3091321738930619678 ) ) ;
#39148 = CARTESIAN_POINT ( 'NONE',  ( 9.089826843846916304, 119.3941581119689204, -1.016340006442031152 ) ) ;
#39147 = CARTESIAN_POINT ( 'NONE',  ( 1.146080138889219446, 106.2781093257879803, 5.162130396633914486 ) ) ;
#39149 = CARTESIAN_POINT ( 'NONE',  ( 4.064497669612420871, 2.951628549105334898, 2.233594334442648766 ) ) ;
#39150 = CARTESIAN_POINT ( 'NONE',  ( -1.957152676258903323, 116.9869758084673208, -0.4489687564533212938 ) ) ;
#39151 = ADVANCED_FACE ( 'NONE', ( #30222 ), #25051, .T. ) ;
#39152 = ORIENTED_EDGE ( 'NONE', *, *, #41983, .T. ) ;
#39153 = CARTESIAN_POINT ( 'NONE',  ( -8.172795105213701561, 122.8283871457973362, 0.1257892658093058003 ) ) ;
#39154 = CARTESIAN_POINT ( 'NONE',  ( 5.943076596790061394, -13.74187730036333122, 2.284392803971454278 ) ) ;
#39155 = CARTESIAN_POINT ( 'NONE',  ( -23.94760723868026631, 77.08694321397520355, 1.269999999999992912 ) ) ;
#39156 = CARTESIAN_POINT ( 'NONE',  ( -3.009709740711283388, 107.7307366742582104, -4.394550567200004920 ) ) ;
#39158 = ORIENTED_EDGE ( 'NONE', *, *, #31687, .F. ) ;
#39157 = VECTOR ( 'NONE', #29116, 1000.000000000000000 ) ;
#39159 = CARTESIAN_POINT ( 'NONE',  ( 19.50074546578241907, 147.2819018089465715, 2.521100153936117749 ) ) ;
#39160 = PLANE ( 'NONE',  #4560 ) ;
#39161 = CARTESIAN_POINT ( 'NONE',  ( 8.487687333566158898, 123.3253871723413368, 0.1696041924978713422 ) ) ;
#39162 = CARTESIAN_POINT ( 'NONE',  ( -22.42204277426977299, 149.9331680011685251, 0.7277228188736590830 ) ) ;
#39163 = CARTESIAN_POINT ( 'NONE',  ( 15.83110339195386729, 121.2341309109925334, -0.1099079758964731507 ) ) ;
#39164 = CARTESIAN_POINT ( 'NONE',  ( -29.82321757229076908, 71.17901112636586447, -1.270000000000007123 ) ) ;
#39165 = CARTESIAN_POINT ( 'NONE',  ( -49.98771841168287722, 16.20356568994197843, 4.825110013074525916 ) ) ;
#39166 = CARTESIAN_POINT ( 'NONE',  ( -47.04217617083259029, 23.73857702128102076, 2.948847133965281309 ) ) ;
#39167 = CARTESIAN_POINT ( 'NONE',  ( -4.862674337261732482, 117.4104240214870885, -1.165717098571217747 ) ) ;
#39168 = CARTESIAN_POINT ( 'NONE',  ( -54.39768377094780760, 8.094885465611476150, 3.421923752996821833 ) ) ;
#39169 = CARTESIAN_POINT ( 'NONE',  ( -4.416771755448873904, 71.99420641645033925, -1.523999999999994248 ) ) ;
#39170 = CARTESIAN_POINT ( 'NONE',  ( -4.543708444177163130, 118.0889193232460599, 0.5957003991893521366 ) ) ;
#39171 = CARTESIAN_POINT ( 'NONE',  ( -5.809227842914839179, 77.60418761620948658, -1.269999999999996021 ) ) ;
#39172 = B_SPLINE_SURFACE_WITH_KNOTS ( 'NONE', 3, 3, ( 
 ( #25242, #13880, #6083, #22231, #4107, #25458, #31843, #16643 ),
 ( #29651, #20046, #36263, #35259, #36049, #489, #907, #25658 ),
 ( #23660, #38455, #26661, #33064, #23229, #39669, #7083, #3895 ),
 ( #10473, #19046, #16859, #9273, #12464, #10049, #23442, #5877 ) ),
 .UNSPECIFIED., .F., .F., .F.,
 ( 4, 4 ),
 ( 4, 2, 2, 4 ),
 ( 0.000000000000000000, 1.000000000000000000 ),
 ( 0.000000000000000000, 0.2500000000000000000, 0.5000000000000000000, 1.000000000000000000 ),
 .UNSPECIFIED. ) ;
#39173 = EDGE_LOOP ( 'NONE', ( #23279, #34327, #1248, #14787 ) ) ;
#39174 = CARTESIAN_POINT ( 'NONE',  ( -4.000258988046152098, 115.6909491485452719, -1.587041804271255296 ) ) ;
#39176 = EDGE_CURVE ( 'NONE', #40534, #36287, #23151, .T. ) ;
#39175 = CARTESIAN_POINT ( 'NONE',  ( -5.905050715485153034, 119.1078666374620667, -1.262661138395162697 ) ) ;
#39177 = CARTESIAN_POINT ( 'NONE',  ( -6.094139411022071684, 119.5248422734510427, -0.5163842741021831273 ) ) ;
#39178 = CARTESIAN_POINT ( 'NONE',  ( 4.697508090083865717, 117.7521314560283088, 1.088652043387917434 ) ) ;
#39179 = CARTESIAN_POINT ( 'NONE',  ( -46.97515415817102280, 24.89137758704634962, -2.045406795549905787 ) ) ;
#39180 = CARTESIAN_POINT ( 'NONE',  ( -9.631798221454433317, 123.4354624054469980, -1.070950170652381184 ) ) ;
#39181 = CARTESIAN_POINT ( 'NONE',  ( -3.691024713256037870, 109.5877217411341320, 3.633260444712922865 ) ) ;
#39182 = CARTESIAN_POINT ( 'NONE',  ( 7.614108603649442308, 124.2930771091975117, 0.1432033155151097026 ) ) ;
#39183 = CARTESIAN_POINT ( 'NONE',  ( -16.97388159461598534, 146.7604995623492243, -1.927701477367710803 ) ) ;
#39184 = CARTESIAN_POINT ( 'NONE',  ( -24.23745918283205469, 82.38670122043342303, 1.269999999999992690 ) ) ;
#39185 = CARTESIAN_POINT ( 'NONE',  ( -0.02874440110946554008, 158.8294072187990196, 1.438487372358303595 ) ) ;
#39186 = VECTOR ( 'NONE', #34399, 1000.000000000000114 ) ;
#39187 = CARTESIAN_POINT ( 'NONE',  ( -2.452794397974936036, 115.7029491485453434, 1.604287042619627845 ) ) ;
#39188 = CARTESIAN_POINT ( 'NONE',  ( -15.72516475228267652, 145.6852934652650902, -0.2469506351165625946 ) ) ;
#39189 = CARTESIAN_POINT ( 'NONE',  ( -3.832284926465886254, -5.753926550059754064, 2.584458424559757272 ) ) ;
#39191 = EDGE_LOOP ( 'NONE', ( #29773, #5410, #20573, #31514 ) ) ;
#39190 = CARTESIAN_POINT ( 'NONE',  ( 22.80460045200408814, 149.7823008822066697, 1.306974408439632640 ) ) ;
#39192 = DIRECTION ( 'NONE',  ( -4.017660918040594346E-17, 1.000000000000000000, 2.376309959284834438E-19 ) ) ;
#39193 = CARTESIAN_POINT ( 'NONE',  ( 3.509229686425914707, -14.99732357267335914, 1.369000748440630799 ) ) ;
#39194 = CARTESIAN_POINT ( 'NONE',  ( -18.49981012119521750, 140.7300538122508726, 1.765484999878023098 ) ) ;
#39195 = CARTESIAN_POINT ( 'NONE',  ( -0.01433812918766144522, 10.07226683256953947, 0.9740319587662029654 ) ) ;
#39196 = CARTESIAN_POINT ( 'NONE',  ( -20.55326960831574823, 152.5775223076369400, -0.9856637426460332918 ) ) ;
#39197 = EDGE_CURVE ( 'NONE', #7000, #26382, #853, .T. ) ;
#39198 = CARTESIAN_POINT ( 'NONE',  ( -0.4866770014159069180, -4.230873095947595530, 0.8487236227246106601 ) ) ;
#39199 = ORIENTED_EDGE ( 'NONE', *, *, #34248, .T. ) ;
#39200 = ORIENTED_EDGE ( 'NONE', *, *, #33725, .T. ) ;
#39201 = CARTESIAN_POINT ( 'NONE',  ( -44.40685758373556524, 19.43703734468909516, -5.999789834925398652E-15 ) ) ;
#39202 = CARTESIAN_POINT ( 'NONE',  ( 6.110436517261101486, 121.4157903421748301, 0.3281350463252858951 ) ) ;
#39203 = CARTESIAN_POINT ( 'NONE',  ( 0.000000000000000000, 0.000000000000000000, 0.000000000000000000 ) ) ;
#39204 = CARTESIAN_POINT ( 'NONE',  ( -3.160209531531049887, 156.1781389015385457, 0.7303267873898459106 ) ) ;
#39205 = CARTESIAN_POINT ( 'NONE',  ( 3.526842715273949214, -14.30601272375732513, 4.884018970202873788 ) ) ;
#39206 = CARTESIAN_POINT ( 'NONE',  ( 10.84737219364637362, 123.3109526380878833, -1.071866780254095985 ) ) ;
#39207 = CARTESIAN_POINT ( 'NONE',  ( -3.201321489863747871, 118.6508749770327995, -0.9018090777949858694 ) ) ;
#39208 = EDGE_CURVE ( 'NONE', #22322, #19534, #22792, .T. ) ;
#39209 = DIRECTION ( 'NONE',  ( 1.000000000000000000, 6.353134868986659519E-16, -0.000000000000000000 ) ) ;
#39210 = CARTESIAN_POINT ( 'NONE',  ( 3.150244473240279675, -14.07033042043420146, 1.813758411523331393 ) ) ;
#39211 = CARTESIAN_POINT ( 'NONE',  ( -2.466321628261904042, 35.32195945946419613, 2.380963110963009832 ) ) ;
#39212 = CARTESIAN_POINT ( 'NONE',  ( 7.582677863711187349, 122.4179301937671767, 0.01237541680613138753 ) ) ;
#39213 = ORIENTED_EDGE ( 'NONE', *, *, #15618, .F. ) ;
#39214 = CARTESIAN_POINT ( 'NONE',  ( -4.429001560254139491, 111.0463454453107346, 3.038333220475521124 ) ) ;
#39215 = DIRECTION ( 'NONE',  ( 0.000000000000000000, 1.000000000000000000, -0.000000000000000000 ) ) ;
#39216 = LINE ( 'NONE', #22783, #7551 ) ;
#39217 = VECTOR ( 'NONE', #12311, 1000.000000000000000 ) ;
#39218 = DIRECTION ( 'NONE',  ( 0.9998004120163609398, 0.000000000000000000, 0.01997839162482749689 ) ) ;
#39219 = VECTOR ( 'NONE', #26903, 1000.000000000000000 ) ;
#39220 = CARTESIAN_POINT ( 'NONE',  ( 15.48485754026165750, 120.7065362441885981, 0.2052890747276165107 ) ) ;
#39221 = CARTESIAN_POINT ( 'NONE',  ( -5.335400302754746527, 116.6867539651165373, 0.8102459553323390073 ) ) ;
#39222 = CARTESIAN_POINT ( 'NONE',  ( -4.060687707471794639, 115.6909491485396728, 1.425937899757264926 ) ) ;
#39223 = CARTESIAN_POINT ( 'NONE',  ( -3.113637796910019961, 33.63258992088869093, 1.040732188486675591 ) ) ;
#39224 = CARTESIAN_POINT ( 'NONE',  ( 17.48279436891377969, 128.5781302034472162, 2.030760391889158800 ) ) ;
#39225 = CARTESIAN_POINT ( 'NONE',  ( 2.794707274389933715, 24.31675177525179876, -3.679445548267922916 ) ) ;
#39226 = CARTESIAN_POINT ( 'NONE',  ( -8.418873817481639321, -10.66996252118913091, -0.4581590610697409693 ) ) ;
#39227 = CARTESIAN_POINT ( 'NONE',  ( 5.513305492129709329, 117.1850219934554502, -0.5726549213627184498 ) ) ;
#39228 = CARTESIAN_POINT ( 'NONE',  ( -0.7406220848565643333, 119.3684187487962305, -0.7644009012486648880 ) ) ;
#39229 = CARTESIAN_POINT ( 'NONE',  ( -22.46755768833301303, 150.8526571111528654, -0.4489552724284875951 ) ) ;
#39230 = FACE_OUTER_BOUND ( 'NONE', #34967, .T. ) ;
#39231 = CARTESIAN_POINT ( 'NONE',  ( -3.165966136369845696, 105.1242010218709169, 4.304718551588531561 ) ) ;
#39232 = CARTESIAN_POINT ( 'NONE',  ( 2.332027132427558769, 25.33165720878049498, 3.998286310156994983 ) ) ;
#39233 = LINE ( 'NONE', #26656, #16411 ) ;
#39234 = CARTESIAN_POINT ( 'NONE',  ( -15.97340373827834270, 121.0409387471171101, -0.3191866212789525314 ) ) ;
#39235 = CARTESIAN_POINT ( 'NONE',  ( 2.660183686505937839, -13.21883649654037640, 0.1900507390742080804 ) ) ;
#39236 = CARTESIAN_POINT ( 'NONE',  ( 3.233068332335714334, 124.0549386377059307, 0.01378491165287854328 ) ) ;
#39237 = CARTESIAN_POINT ( 'NONE',  ( -22.71566531765394714, 150.0520759213295889, 0.3958359165339127017 ) ) ;
#39238 = DIRECTION ( 'NONE',  ( -0.000000000000000000, -1.000000000000000000, -0.000000000000000000 ) ) ;
#39239 = ORIENTED_EDGE ( 'NONE', *, *, #13127, .T. ) ;
#39240 = CARTESIAN_POINT ( 'NONE',  ( 5.965356522962860453, 65.30181249999998272, 5.016499999999999737 ) ) ;
#39241 =( BOUNDED_CURVE ( )  B_SPLINE_CURVE ( 3, ( #37051, #8491, #18472, #37250 ),
 .UNSPECIFIED., .F., .T. ) 
 B_SPLINE_CURVE_WITH_KNOTS ( ( 4, 4 ),
 ( 4.712388980384689674, 6.283185307179585344 ),
 .UNSPECIFIED. ) 
 CURVE ( )  GEOMETRIC_REPRESENTATION_ITEM ( )  RATIONAL_B_SPLINE_CURVE ( ( 1.000000000000000000, 0.8047378541243649375, 0.8047378541243649375, 1.000000000000000000 ) ) 
 REPRESENTATION_ITEM ( '' )  );
#39242 = CIRCLE ( 'NONE', #40621, 0.2540000000000002256 ) ;
#39243 = VERTEX_POINT ( 'NONE', #17227 ) ;
#39244 = DIRECTION ( 'NONE',  ( 0.000000000000000000, -1.000000000000000000, 0.000000000000000000 ) ) ;
#39245 = CARTESIAN_POINT ( 'NONE',  ( 5.683854215195817794, -15.08228171793801664, 1.486458664383613293 ) ) ;
#39246 = CARTESIAN_POINT ( 'NONE',  ( -20.17069300908759999, 147.5185649274072830, 1.704009200980389993 ) ) ;
#39247 = B_SPLINE_CURVE_WITH_KNOTS ( 'NONE', 3,
 ( #13309, #1176, #33551, #26296, #39304, #14139 ),
 .UNSPECIFIED., .F., .F.,
 ( 4, 2, 4 ),
 ( 0.000000000000000000, 0.0001537973894545544668, 0.0003075947789091089337 ),
 .UNSPECIFIED. ) ;
#39248 = CARTESIAN_POINT ( 'NONE',  ( 21.13693409061718853, 150.2702755442954583, -1.277357359820448623 ) ) ;
#39249 = EDGE_CURVE ( 'NONE', #39372, #13050, #30297, .T. ) ;
#39250 = CARTESIAN_POINT ( 'NONE',  ( 4.087030650986479330, 6.990161447142720696, 2.163025551504125232 ) ) ;
#39251 = CARTESIAN_POINT ( 'NONE',  ( -58.51800049984071705, -0.05885670287285882374, -0.6510176481063610909 ) ) ;
#39252 = ORIENTED_EDGE ( 'NONE', *, *, #19781, .F. ) ;
#39253 = CARTESIAN_POINT ( 'NONE',  ( -4.757248700628498916, 117.4032733054477973, -1.206458840162573543 ) ) ;
#39254 = AXIS2_PLACEMENT_3D ( 'NONE', #15843, #28637, #41863 ) ;
#39255 = CARTESIAN_POINT ( 'NONE',  ( 0.7702483762745334639, 120.5370721568272216, 0.5278276654545123181 ) ) ;
#39256 = CARTESIAN_POINT ( 'NONE',  ( -0.02400040557479403425, 156.7459281804771365, 1.201078436782489822 ) ) ;
#39257 = CARTESIAN_POINT ( 'NONE',  ( -44.11964021406032543, 21.57970624656428171, 2.906001918892821223 ) ) ;
#39258 = EDGE_CURVE ( 'NONE', #31300, #19961, #7212, .T. ) ;
#39259 = CARTESIAN_POINT ( 'NONE',  ( 14.49813937024303989, 152.7616507467334372, -1.711219460879523924 ) ) ;
#39260 = CARTESIAN_POINT ( 'NONE',  ( 0.02874440110933761117, 158.8294072187990196, -1.438487372358303151 ) ) ;
#39261 = CARTESIAN_POINT ( 'NONE',  ( -57.43854689232674815, 1.757847328446624058, -1.624773336220253217 ) ) ;
#39262 = ORIENTED_EDGE ( 'NONE', *, *, #9466, .F. ) ;
#39263 = CARTESIAN_POINT ( 'NONE',  ( 4.463198846623864569, 118.1257892472388420, -0.5548194780705337781 ) ) ;
#39264 = CARTESIAN_POINT ( 'NONE',  ( 1.703787162446163128, 156.3322054215483092, -0.5946588160098701392 ) ) ;
#39265 = ORIENTED_EDGE ( 'NONE', *, *, #38191, .F. ) ;
#39266 = CARTESIAN_POINT ( 'NONE',  ( -11.27861017918435316, 123.5700555580090594, -1.596916299002706596 ) ) ;
#39267 = CARTESIAN_POINT ( 'NONE',  ( 3.190981477959303980, -15.14443901668413517, 3.594454035019850835 ) ) ;
#39268 = FACE_OUTER_BOUND ( 'NONE', #29029, .T. ) ;
#39269 = VECTOR ( 'NONE', #23777, 1000.000000000000227 ) ;
#39270 = DIRECTION ( 'NONE',  ( -4.017660918040594346E-17, 1.000000000000000000, 2.376309959284834438E-19 ) ) ;
#39271 = CARTESIAN_POINT ( 'NONE',  ( 2.854375549615681962, 5.100648791940559867, -3.633247542873777380 ) ) ;
#39272 = CARTESIAN_POINT ( 'NONE',  ( 11.62460634082105493, 124.4569610989641859, 1.598101315089358154 ) ) ;
#39273 = CARTESIAN_POINT ( 'NONE',  ( -2.571890136738498978, 30.56018956238373363, 0.9273410376875194094 ) ) ;
#39274 = CARTESIAN_POINT ( 'NONE',  ( 8.369638709285570854, -11.69152869469262157, 0.7709884470677680346 ) ) ;
#39275 = CARTESIAN_POINT ( 'NONE',  ( 5.920896852643619646, 121.5237468798633955, 0.2406035128457659489 ) ) ;
#39276 = FACE_OUTER_BOUND ( 'NONE', #14189, .T. ) ;
#39277 = CIRCLE ( 'NONE', #37236, 6.349999999999999645 ) ;
#39278 = CARTESIAN_POINT ( 'NONE',  ( -45.15528325240632057, 20.88806775524793125, -3.529375091719475943 ) ) ;
#39279 = CARTESIAN_POINT ( 'NONE',  ( 2.182419039857114385, 116.2183432897882653, -0.07172189831550286609 ) ) ;
#39280 = DIRECTION ( 'NONE',  ( -1.000000000000000000, 0.000000000000000000, 0.000000000000000000 ) ) ;
#39281 = FACE_OUTER_BOUND ( 'NONE', #4759, .T. ) ;
#39282 = FACE_OUTER_BOUND ( 'NONE', #40833, .T. ) ;
#39283 = CARTESIAN_POINT ( 'NONE',  ( -8.788223396658947806, 117.7098387909605748, -0.3782402184110820742 ) ) ;
#39284 = CARTESIAN_POINT ( 'NONE',  ( -5.475330206976867231, 65.30181249999996851, 5.107412922131463695 ) ) ;
#39285 = CARTESIAN_POINT ( 'NONE',  ( -4.074955089416341991, 118.2429491485453354, 0.1454234154749719787 ) ) ;
#39286 = CARTESIAN_POINT ( 'NONE',  ( -27.59695233663404679, 58.25262445104075226, 1.523999999999995358 ) ) ;
#39287 = CARTESIAN_POINT ( 'NONE',  ( -55.34794038087419210, 7.786537553440359360, 3.264576684945853291 ) ) ;
#39288 = CARTESIAN_POINT ( 'NONE',  ( -58.03414100541874632, 0.4564111095344686175, 0.9708715263941495310 ) ) ;
#39289 = CARTESIAN_POINT ( 'NONE',  ( -22.80463473692780241, 150.3987591554885626, -0.1267456695372859987 ) ) ;
#39290 = ORIENTED_EDGE ( 'NONE', *, *, #41569, .T. ) ;
#39291 = CARTESIAN_POINT ( 'NONE',  ( -51.34394198884087501, 20.23131347170496142, -0.7795225783603546565 ) ) ;
#39292 = CARTESIAN_POINT ( 'NONE',  ( 7.802319612832663509, 122.5629922761574306, -0.05915617574866657152 ) ) ;
#39293 = EDGE_LOOP ( 'NONE', ( #42096, #13099, #10640, #23722 ) ) ;
#39294 = CARTESIAN_POINT ( 'NONE',  ( 3.517175496330608997, 50.13146620154573441, -1.199971990511068398 ) ) ;
#39295 = CARTESIAN_POINT ( 'NONE',  ( -13.59447973938445031, 150.2262467139961473, -0.3969463805754209207 ) ) ;
#39296 = CARTESIAN_POINT ( 'NONE',  ( 6.095337826619875443, -12.40160515274643593, 0.5428006832284221206 ) ) ;
#39297 = CARTESIAN_POINT ( 'NONE',  ( -13.58393798013060838, 155.6725583577350278, 1.480266515874766542 ) ) ;
#39298 = CARTESIAN_POINT ( 'NONE',  ( -4.507778648822867495, 31.37953541088120346, -1.025544427737863362 ) ) ;
#39299 = CARTESIAN_POINT ( 'NONE',  ( 15.70536794749878240, 121.0099257824619627, 0.6352152019007784034 ) ) ;
#39300 = CARTESIAN_POINT ( 'NONE',  ( 2.049679743348181038, -15.55809256208866209, 5.945888963465825405 ) ) ;
#39301 = CARTESIAN_POINT ( 'NONE',  ( 4.815088043200419499, 118.5266822147775940, -0.8000015276336421843 ) ) ;
#39302 = CARTESIAN_POINT ( 'NONE',  ( -0.7776641127062334791, -6.825634839940509124, -0.5883101582535473772 ) ) ;
#39303 = CARTESIAN_POINT ( 'NONE',  ( 0.001838942458790341966, 116.4858755864912183, -0.09202820039585828116 ) ) ;
#39304 = CARTESIAN_POINT ( 'NONE',  ( -4.697434178460381027, 117.9270761130219256, 0.7736398133629062146 ) ) ;
#39305 = ADVANCED_FACE ( 'NONE', ( #1275 ), #12642, .F. ) ;
#39306 = DIRECTION ( 'NONE',  ( -5.188838149069472160E-16, 1.699382548006136559E-16, 1.000000000000000000 ) ) ;
#39307 = VERTEX_POINT ( 'NONE', #1895 ) ;
#39308 = CARTESIAN_POINT ( 'NONE',  ( 5.549484939100879366, 116.7640263767076050, 0.3607275616457042977 ) ) ;
#39309 = ORIENTED_EDGE ( 'NONE', *, *, #30969, .T. ) ;
#39310 = CARTESIAN_POINT ( 'NONE',  ( -17.67908073341003217, 148.3509993576462307, 1.576626744559513682 ) ) ;
#39311 = CARTESIAN_POINT ( 'NONE',  ( -58.36826665097051148, -0.2883791471137164830, -0.04671551776550799534 ) ) ;
#39312 = CARTESIAN_POINT ( 'NONE',  ( 7.848884907109186848, 118.8455990504009492, 1.250143668394028351 ) ) ;
#39313 = CARTESIAN_POINT ( 'NONE',  ( 4.459427130834354713, 157.7533977378147654, -1.670975814381038704 ) ) ;
#39314 = CARTESIAN_POINT ( 'NONE',  ( 0.2616662591921395387, 4.880059721033824793, -0.9399936778652994152 ) ) ;
#39315 = CARTESIAN_POINT ( 'NONE',  ( -21.74240605069427446, 146.0876064316611860, -2.155783927327832306 ) ) ;
#39316 = ADVANCED_FACE ( 'NONE', ( #21040 ), #38492, .T. ) ;
#39317 = CARTESIAN_POINT ( 'NONE',  ( 4.634426409561430482, 118.0229150531969680, -0.6600590983778304999 ) ) ;
#39318 = DIRECTION ( 'NONE',  ( -5.206863593109713661E-17, 1.000000000000000000, -1.077750396879097183E-30 ) ) ;
#39319 = CARTESIAN_POINT ( 'NONE',  ( 10.91797240702838501, 124.6990478933366404, -0.8611562105571394232 ) ) ;
#39320 = CARTESIAN_POINT ( 'NONE',  ( -5.659105795943250034E-14, 120.9974662015457341, 1.217662469992124504E-16 ) ) ;
#39321 = EDGE_LOOP ( 'NONE', ( #40735, #9697, #3256, #4678 ) ) ;
#39322 = CARTESIAN_POINT ( 'NONE',  ( -2.387603053075764592, 119.2205458019918751, -0.7760930522211748617 ) ) ;
#39323 = CARTESIAN_POINT ( 'NONE',  ( 5.510877305967752271, -15.11690630435501248, 2.581843384194929758 ) ) ;
#39324 = CARTESIAN_POINT ( 'NONE',  ( -12.21488373879589240, 55.24499999999999034, 5.016499999999999737 ) ) ;
#39325 = CARTESIAN_POINT ( 'NONE',  ( -44.66298991629287940, 23.47648082339880915, -1.964675176939946644 ) ) ;
#39326 = CARTESIAN_POINT ( 'NONE',  ( 5.834672723501171276, 119.9178398404649926, 1.129903066036338055 ) ) ;
#39327 = CARTESIAN_POINT ( 'NONE',  ( -4.974001918040873882, 117.3966124607983659, -0.9751453929904890794 ) ) ;
#39328 = LINE ( 'NONE', #28890, #14363 ) ;
#39329 =( GEOMETRIC_REPRESENTATION_CONTEXT ( 3 ) GLOBAL_UNCERTAINTY_ASSIGNED_CONTEXT ( ( #3570 ) ) GLOBAL_UNIT_ASSIGNED_CONTEXT ( ( #19633, #13045, #22819 ) ) REPRESENTATION_CONTEXT ( 'NONE', 'WORKASPACE' ) );
#39330 = CARTESIAN_POINT ( 'NONE',  ( -0.5697667371462552532, 106.2969274751293938, 5.150121607182108541 ) ) ;
#39331 = CARTESIAN_POINT ( 'NONE',  ( -7.836836066720379357, 21.45871166075947656, -3.113543590022962881 ) ) ;
#39332 = CARTESIAN_POINT ( 'NONE',  ( 8.208845571667657381, 122.7966848691156514, 0.5426025200548866279 ) ) ;
#39333 = CARTESIAN_POINT ( 'NONE',  ( 11.30743779403327487, 119.0414093155750379, -0.5171725168954617313 ) ) ;
#39334 = EDGE_CURVE ( 'NONE', #2940, #8461, #35753, .T. ) ;
#39335 = CARTESIAN_POINT ( 'NONE',  ( -6.059261036834082681, 78.87450423423038615, -5.016499999999999737 ) ) ;
#39336 = CARTESIAN_POINT ( 'NONE',  ( -6.606029807653651701E-14, 92.04146620154574521, -3.372746026535634231E-18 ) ) ;
#39337 = AXIS2_PLACEMENT_3D ( 'NONE', #25732, #12541, #25938 ) ;
#39338 = UNCERTAINTY_MEASURE_WITH_UNIT (LENGTH_MEASURE( 1.000000000000000082E-05 ), #25692, 'distance_accuracy_value', 'NONE');
#39339 = CARTESIAN_POINT ( 'NONE',  ( -3.301441731159381998, 159.4676453237595410, -0.05120667577156005901 ) ) ;
#39340 = ORIENTED_EDGE ( 'NONE', *, *, #28217, .F. ) ;
#39341 = CARTESIAN_POINT ( 'NONE',  ( -5.387388416630612298, 120.5907514897421606, -0.7742399106899608974 ) ) ;
#39342 = CARTESIAN_POINT ( 'NONE',  ( -3.517175496330734674, 50.63946620154572997, 1.199971990511067954 ) ) ;
#39343 = CARTESIAN_POINT ( 'NONE',  ( -0.6635084510829686311, 156.3292479207028407, -0.3574603001491368781 ) ) ;
#39344 = CARTESIAN_POINT ( 'NONE',  ( 2.161572811135036964, -15.02537755669194830, 5.771884496758437066 ) ) ;
#39345 = CARTESIAN_POINT ( 'NONE',  ( -0.3839177515435807653, 117.3568105388816321, 0.4297925318014835794 ) ) ;
#39346 = CARTESIAN_POINT ( 'NONE',  ( 6.079889189570776509, 121.4459138077559714, 0.1214906566337395633 ) ) ;
#39347 = CARTESIAN_POINT ( 'NONE',  ( 4.723387343850681042, 116.7592613395855352, 0.1361797943638455854 ) ) ;
#39348 = ADVANCED_FACE ( 'NONE', ( #25083 ), #41291, .T. ) ;
#39349 = ORIENTED_EDGE ( 'NONE', *, *, #37275, .T. ) ;
#39350 = CARTESIAN_POINT ( 'NONE',  ( 4.560443952884764229, -11.68867000232777542, 0.6947937212093100445 ) ) ;
#39351 = DIRECTION ( 'NONE',  ( -5.188838149069472160E-16, 1.699382548006136559E-16, 1.000000000000000000 ) ) ;
#39352 = FACE_OUTER_BOUND ( 'NONE', #12369, .T. ) ;
#39353 = DIRECTION ( 'NONE',  ( 9.627370216492862708E-17, 1.000000000000000000, -0.000000000000000000 ) ) ;
#39354 = CARTESIAN_POINT ( 'NONE',  ( -6.866951340267982040, 120.5627663870395452, 0.8828549736221562583 ) ) ;
#39355 = CARTESIAN_POINT ( 'NONE',  ( 3.363087486136625337, 4.875765145370108300, -3.182472177310056605 ) ) ;
#39356 = CARTESIAN_POINT ( 'NONE',  ( 14.51109376910509496, 156.0472725025049954, 1.459756479172739319 ) ) ;
#39357 = CARTESIAN_POINT ( 'NONE',  ( -0.04257260548303649222, 114.5099076536771321, 2.130507264987370863 ) ) ;
#39359 = CARTESIAN_POINT ( 'NONE',  ( 13.43626322254335470, 155.6061939908119882, -1.534180175809178426 ) ) ;
#39358 = FACE_OUTER_BOUND ( 'NONE', #39099, .T. ) ;
#39360 = CARTESIAN_POINT ( 'NONE',  ( -4.255528399684056495, 7.899375212487111497, -1.818898740287305138 ) ) ;
#39361 = CARTESIAN_POINT ( 'NONE',  ( -19.35449845750125419, 128.7092500879292345, -1.403651888282934079 ) ) ;
#39362 = ORIENTED_EDGE ( 'NONE', *, *, #644, .F. ) ;
#39363 = EDGE_CURVE ( 'NONE', #18759, #34369, #21461, .T. ) ;
#39364 = CARTESIAN_POINT ( 'NONE',  ( -9.049782359939607446, 124.0675141969884692, -0.1808361888366265546 ) ) ;
#39365 = ORIENTED_EDGE ( 'NONE', *, *, #35525, .T. ) ;
#39366 = CARTESIAN_POINT ( 'NONE',  ( -4.553626923285223782, 121.1438296405421937, 0.06679122792761502114 ) ) ;
#39368 = CARTESIAN_POINT ( 'NONE',  ( 6.383535934857802907, -12.90002020050165576, 0.3830569482466484321 ) ) ;
#39367 = VECTOR ( 'NONE', #3722, 1000.000000000000114 ) ;
#39369 = CONICAL_SURFACE ( 'NONE', #12842, 1.905000000000007354, 0.7853981633974428389 ) ;
#39370 = CARTESIAN_POINT ( 'NONE',  ( -29.82321757229076908, 71.17901112636586447, -1.524000000000007349 ) ) ;
#39371 = CARTESIAN_POINT ( 'NONE',  ( -3.155546303928757457, 108.2676741415912858, -4.292845182925542069 ) ) ;
#39372 = VERTEX_POINT ( 'NONE', #30846 ) ;
#39373 = CARTESIAN_POINT ( 'NONE',  ( 4.132678194918469217, 118.9132445967212419, 1.007338114003851537 ) ) ;
#39374 = CARTESIAN_POINT ( 'NONE',  ( -30.45812239790965492, 71.16801738242446618, -1.524000000000007793 ) ) ;
#39375 = CARTESIAN_POINT ( 'NONE',  ( -10.15441061790785682, 81.86333342972157823, -1.269999999999998908 ) ) ;
#39376 = CARTESIAN_POINT ( 'NONE',  ( -22.63811803560004421, 149.3758529064199934, 0.7269731895922281195 ) ) ;
#39378 = EDGE_CURVE ( 'NONE', #37219, #16254, #16708, .T. ) ;
#39377 = CARTESIAN_POINT ( 'NONE',  ( 4.581910832313284665, -15.30292673639559098, -0.5105377408573423814 ) ) ;
#39379 = CARTESIAN_POINT ( 'NONE',  ( 10.70371904046263190, 157.9381250348597234, -0.2505172755855809563 ) ) ;
#39380 = CARTESIAN_POINT ( 'NONE',  ( -5.570730988718118226, 56.51499999999999346, -4.419918923950581835 ) ) ;
#39381 = CARTESIAN_POINT ( 'NONE',  ( -48.95619900250866863, 17.85589990993532439, 5.076226165768623844 ) ) ;
#39382 = CARTESIAN_POINT ( 'NONE',  ( -47.35944255389389923, 21.37623662739411401, 4.722871667523157235 ) ) ;
#39383 = CARTESIAN_POINT ( 'NONE',  ( -41.28107547821694112, 23.22158991241130011, 1.523999999999988475 ) ) ;
#39384 = EDGE_CURVE ( 'NONE', #37691, #8502, #41908, .T. ) ;
#39385 = CARTESIAN_POINT ( 'NONE',  ( -50.11792632901008915, 17.09067799859288783, 5.048577231237564966 ) ) ;
#39386 = CARTESIAN_POINT ( 'NONE',  ( -11.53797084252497562, 82.58007221317646440, 1.269999999999999130 ) ) ;
#39387 = CARTESIAN_POINT ( 'NONE',  ( -4.459910022453251521, 118.1246115026546732, 0.5576706506857700418 ) ) ;
#39388 = CARTESIAN_POINT ( 'NONE',  ( -5.435468916197979006, 78.92497954178517716, -5.153742819109117690 ) ) ;
#39389 = VERTEX_POINT ( 'NONE', #24239 ) ;
#39390 = DIRECTION ( 'NONE',  ( -0.8572391118119510045, -0.5149185422762100339, -3.573031421855330583E-16 ) ) ;
#39391 = CIRCLE ( 'NONE', #19657, 0.2539999999999997260 ) ;
#39392 = CARTESIAN_POINT ( 'NONE',  ( -8.279947364166304169, 120.0867420158548811, -1.450008613624738762 ) ) ;
#39393 = CARTESIAN_POINT ( 'NONE',  ( -6.487065698695111848, 120.6500652548963899, -0.3947850323583859677 ) ) ;
#39394 = CARTESIAN_POINT ( 'NONE',  ( 4.635084781736964032, 118.0285823782326986, 0.7661035724334133157 ) ) ;
#39395 = CARTESIAN_POINT ( 'NONE',  ( -9.696059495791558902, 123.7664141286412871, -0.9760873372638445566 ) ) ;
#39396 = CARTESIAN_POINT ( 'NONE',  ( -1.785155554672699596, 115.7029483421136860, -1.723366978510304071 ) ) ;
#39397 = CARTESIAN_POINT ( 'NONE',  ( 0.4168181486211068876, 118.1651002420108512, -0.8784302966413096714 ) ) ;
#39398 = CARTESIAN_POINT ( 'NONE',  ( 6.109903564962296585, 119.5248422734510427, -0.2725184514339174524 ) ) ;
#39399 = CARTESIAN_POINT ( 'NONE',  ( -12.90748236152463413, 128.4900567078429390, -1.625332807165861260 ) ) ;
#39400 = DIRECTION ( 'NONE',  ( -5.188838149069472160E-16, 1.699382548006136559E-16, 1.000000000000000000 ) ) ;
#39401 = DIRECTION ( 'NONE',  ( -0.8745520943968080330, 0.4849315768086841505, -5.271987356194194978E-16 ) ) ;
#39402 = CARTESIAN_POINT ( 'NONE',  ( 8.730044398488933766, 118.0746546384499851, -0.4875147713271585914 ) ) ;
#39403 = CARTESIAN_POINT ( 'NONE',  ( -4.621900518278277303, 121.2009512970921037, -0.02108223683487064209 ) ) ;
#39404 = CARTESIAN_POINT ( 'NONE',  ( -2.983771112188844832, -5.329111280313512999, 3.548611825089460048 ) ) ;
#39405 = CARTESIAN_POINT ( 'NONE',  ( 16.56062761363012825, 155.2525159475892167, 1.104293791145710024 ) ) ;
#39406 = CYLINDRICAL_SURFACE ( 'NONE', #8384, 0.5080000000000000071 ) ;
#39407 = CARTESIAN_POINT ( 'NONE',  ( 3.044219152853963717, -14.30162947539197127, 0.8262259773895895831 ) ) ;
#39408 = CARTESIAN_POINT ( 'NONE',  ( -19.01335237852168092, 147.2511928822236769, 1.726116106780064108 ) ) ;
#39409 = CARTESIAN_POINT ( 'NONE',  ( -0.4197673533123916778, 5.974963139197415174, -0.8815698914671175057 ) ) ;
#39410 = CARTESIAN_POINT ( 'NONE',  ( -21.76232006938128194, 151.4242408681541008, -1.019401482499525669 ) ) ;
#39411 = CARTESIAN_POINT ( 'NONE',  ( -0.9274737138984842089, 27.34353985424608524, 0.2860612317039745167 ) ) ;
#39412 = VERTEX_POINT ( 'NONE', #37449 ) ;
#39413 = EDGE_CURVE ( 'NONE', #26517, #14331, #22130, .T. ) ;
#39414 = ORIENTED_EDGE ( 'NONE', *, *, #23212, .F. ) ;
#39415 = CARTESIAN_POINT ( 'NONE',  ( -47.11704014324648426, 20.18577099567724886, 5.127035723291425207 ) ) ;
#39416 = CARTESIAN_POINT ( 'NONE',  ( 6.266908424742160477, 120.0898888515776264, 0.4521870875522998046 ) ) ;
#39417 = CARTESIAN_POINT ( 'NONE',  ( -13.64865021167028836, 134.2686865373913463, 0.6688813089635640141 ) ) ;
#39418 = CARTESIAN_POINT ( 'NONE',  ( 3.244298476066852732, -14.49340328532226785, 5.143112664727522265 ) ) ;
#39419 = CARTESIAN_POINT ( 'NONE',  ( 16.40043613793195476, 149.3997711511537148, -1.468335723160356432 ) ) ;
#39420 = CARTESIAN_POINT ( 'NONE',  ( -16.38264815551540465, 131.4813445454897192, -2.297577408150382805 ) ) ;
#39421 = CARTESIAN_POINT ( 'NONE',  ( 2.664052010559913253, -13.52006206191685322, 0.08958796903007473778 ) ) ;
#39422 = CARTESIAN_POINT ( 'NONE',  ( -1.651955067937024291, 36.17532580612054005, 1.851243363282029764 ) ) ;
#39423 = CARTESIAN_POINT ( 'NONE',  ( 9.057492758458241866, 123.9289873439938674, 0.02221773104347221292 ) ) ;
#39424 = VERTEX_POINT ( 'NONE', #12095 ) ;
#39425 = EDGE_CURVE ( 'NONE', #11324, #5052, #28956, .T. ) ;
#39426 = CARTESIAN_POINT ( 'NONE',  ( 17.14499999999999957, 71.11999999999999034, 5.016499999999999737 ) ) ;
#39427 = CARTESIAN_POINT ( 'NONE',  ( -6.350000000000054712, 86.35999999999998522, 7.776507174585692163E-16 ) ) ;
#39428 = CIRCLE ( 'NONE', #12902, 13.46199999999999442 ) ;
#39429 = AXIS2_PLACEMENT_3D ( 'NONE', #21921, #40914, #14697 ) ;
#39430 = CARTESIAN_POINT ( 'NONE',  ( 10.28897677580358305, 56.51500000000000057, -4.381500000000000838 ) ) ;
#39431 = DIRECTION ( 'NONE',  ( -5.188838149069472160E-16, 1.699382548006136559E-16, 1.000000000000000000 ) ) ;
#39432 = CARTESIAN_POINT ( 'NONE',  ( 2.757293845589572356, 116.5489981622532127, -0.01971897987843767783 ) ) ;
#39433 = EDGE_CURVE ( 'NONE', #19019, #27525, #14663, .T. ) ;
#39434 = CARTESIAN_POINT ( 'NONE',  ( -6.150459292200251227, 119.5049778551863682, 0.2724401547530462819 ) ) ;
#39435 = ADVANCED_FACE ( 'NONE', ( #15068 ), #41079, .T. ) ;
#39436 = CARTESIAN_POINT ( 'NONE',  ( -2.721379687168246075, 118.0926204763706693, 0.8515759891865197773 ) ) ;
#39437 = FACE_OUTER_BOUND ( 'NONE', #30796, .T. ) ;
#39438 = CARTESIAN_POINT ( 'NONE',  ( -4.679832524073478162, 32.47693947602098063, 1.143146696348500635 ) ) ;
#39439 = CARTESIAN_POINT ( 'NONE',  ( 18.42009423903789411, 151.8926627062091086, 2.314360763190140613 ) ) ;
#39440 = CARTESIAN_POINT ( 'NONE',  ( 4.626035402534343532, 22.79242798913371360, 0.3558936578225105341 ) ) ;
#39441 = CARTESIAN_POINT ( 'NONE',  ( -8.293629857537270667, 31.38027257336059250, -1.381021427861755635 ) ) ;
#39442 = CARTESIAN_POINT ( 'NONE',  ( 5.580386988971347328, 118.0037885632721668, -0.8768600884250703498 ) ) ;
#39443 = CARTESIAN_POINT ( 'NONE',  ( -0.7055264248722583620, 108.7514562038770976, -4.178308661695779413 ) ) ;
#39444 = DIRECTION ( 'NONE',  ( 0.7071067811865479058, -0.7071067811865472397, 0.000000000000000000 ) ) ;
#39445 = CARTESIAN_POINT ( 'NONE',  ( -2.943103431893902666, 108.2626378167148573, -4.302975101750876163 ) ) ;
#39446 = CARTESIAN_POINT ( 'NONE',  ( 1.821065711545410970, 105.1241838947191525, 5.023790078975794771 ) ) ;
#39447 = CARTESIAN_POINT ( 'NONE',  ( 1.141857472271699425, 24.90688314728939190, 4.478778191171412182 ) ) ;
#39448 = DIRECTION ( 'NONE',  ( 9.627370216492862708E-17, 1.000000000000000000, -0.000000000000000000 ) ) ;
#39449 = B_SPLINE_CURVE_WITH_KNOTS ( 'NONE', 3,
 ( #26561, #7820, #17177, #16964 ),
 .UNSPECIFIED., .F., .F.,
 ( 4, 4 ),
 ( 0.02839955696672240640, 1.000000000000000000 ),
 .UNSPECIFIED. ) ;
#39450 = CARTESIAN_POINT ( 'NONE',  ( 2.467608985616319472, -14.95545905184315849, 4.893820528943690462 ) ) ;
#39451 = CARTESIAN_POINT ( 'NONE',  ( 2.040875107092296137, 122.5452913651401587, -0.1521094801190006895 ) ) ;
#39452 = CARTESIAN_POINT ( 'NONE',  ( -21.87092457242496479, 136.8312970274703844, 0.6093905233339396155 ) ) ;
#39453 = CIRCLE ( 'NONE', #19025, 0.6350000000000030065 ) ;
#39454 = CARTESIAN_POINT ( 'NONE',  ( -16.42052266156670726, 59.67959903468464233, 5.072843609925764774 ) ) ;
#39455 = ORIENTED_EDGE ( 'NONE', *, *, #25847, .F. ) ;
#39456 = CARTESIAN_POINT ( 'NONE',  ( -5.938360781727970661, 56.51499999999998636, 4.381499999999999950 ) ) ;
#39457 = AXIS2_PLACEMENT_3D ( 'NONE', #15021, #37406, #41458 ) ;
#39458 = ORIENTED_EDGE ( 'NONE', *, *, #10228, .T. ) ;
#39459 = CARTESIAN_POINT ( 'NONE',  ( 6.059261036834405090, 56.51500000000000057, -4.381499999999999950 ) ) ;
#39460 = CARTESIAN_POINT ( 'NONE',  ( 5.927515451590630313, -14.79481669900410701, -0.3156388015035426764 ) ) ;
#39461 = CARTESIAN_POINT ( 'NONE',  ( -1.145842520593037150, 158.4310823543925721, 1.558676969884219554 ) ) ;
#39462 = CARTESIAN_POINT ( 'NONE',  ( 19.46267448186331350, 131.9512773411433670, -1.172478082078345363 ) ) ;
#39463 = CARTESIAN_POINT ( 'NONE',  ( 1.686640475165922748, -9.627085671684914914, -4.319569293544198274 ) ) ;
#39464 = CARTESIAN_POINT ( 'NONE',  ( -58.82792982499385914, -0.2609477946144658778, -0.04398265886348604742 ) ) ;
#39465 = ORIENTED_EDGE ( 'NONE', *, *, #11387, .T. ) ;
#39466 = CARTESIAN_POINT ( 'NONE',  ( -4.942124793971827579, 117.4083539704047183, -1.067544502694063979 ) ) ;
#39467 = CARTESIAN_POINT ( 'NONE',  ( 0.7330347863449895307, 118.7604188656930120, 0.9075975635256807728 ) ) ;
#39468 = DIRECTION ( 'NONE',  ( 1.000000000000000000, 0.000000000000000000, 0.000000000000000000 ) ) ;
#39469 = CARTESIAN_POINT ( 'NONE',  ( -15.03323000681570498, 150.5987129668814077, 1.374706190065595690 ) ) ;
#39470 = CYLINDRICAL_SURFACE ( 'NONE', #20467, 6.349999999999999645 ) ;
#39471 = CARTESIAN_POINT ( 'NONE',  ( 18.70798771669547378, 146.9271955717142930, -1.702497825003243648 ) ) ;
#39472 = CARTESIAN_POINT ( 'NONE',  ( -19.77411333694952233, 150.7280352275851101, -2.313572189391364109 ) ) ;
#39473 = CARTESIAN_POINT ( 'NONE',  ( -57.92346726745822849, 0.7446056814934959300, -1.206286704679871535 ) ) ;
#39474 = ORIENTED_EDGE ( 'NONE', *, *, #25445, .T. ) ;
#39475 = CARTESIAN_POINT ( 'NONE',  ( 4.558708663912786285, 118.0891419347824751, -0.5801029092231412276 ) ) ;
#39476 = ADVANCED_FACE ( 'NONE', ( #11454 ), #24876, .T. ) ;
#39477 = CARTESIAN_POINT ( 'NONE',  ( 10.06005632938184924, 124.8772485319846055, -0.3443025955426558538 ) ) ;
#39478 = ORIENTED_EDGE ( 'NONE', *, *, #28238, .T. ) ;
#39479 = CARTESIAN_POINT ( 'NONE',  ( -5.258743330460844412, 156.4258374981641282, -1.697662213785431140 ) ) ;
#39480 = CARTESIAN_POINT ( 'NONE',  ( 1.834459164715513291, -15.41678468052755413, 5.387059099755636460 ) ) ;
#39481 = CARTESIAN_POINT ( 'NONE',  ( -29.81357423954495189, 70.62209452652477637, -1.270000000000007123 ) ) ;
#39482 = CARTESIAN_POINT ( 'NONE',  ( -57.74058121727584592, 1.065718057877890201, 1.162857118034767545 ) ) ;
#39483 = CARTESIAN_POINT ( 'NONE',  ( 0.9983407785579379023, 1.652274601622760741, 4.518288805521794238 ) ) ;
#39484 = CARTESIAN_POINT ( 'NONE',  ( 5.146579651471712147, 156.3268443366877989, 1.619031734741228190 ) ) ;
#39485 = CARTESIAN_POINT ( 'NONE',  ( 2.247056820894810958, 36.23569059189157571, 0.3352685789618618517 ) ) ;
#39486 = ADVANCED_FACE ( 'NONE', ( #34475 ), #4487, .T. ) ;
#39487 = CARTESIAN_POINT ( 'NONE',  ( 4.364008504204949013, 7.202613900313124873, 1.580794030135405537 ) ) ;
#39488 = CARTESIAN_POINT ( 'NONE',  ( 15.78121303607979797, 145.9231181611787918, 0.5460855120906794591 ) ) ;
#39489 = CARTESIAN_POINT ( 'NONE',  ( -5.924740142096584172, 65.21691166894066782, 1.524000000000005350 ) ) ;
#39490 =( BOUNDED_SURFACE ( )  B_SPLINE_SURFACE ( 2, 3, ( 
 ( #604, #22923, #35954, #19734, #16550, #22714, #9331, #22294, #2949, #41928, #12729, #1439, #1651, #1236, #36386, #23348, #20999, #7615, #39792, #4013, #33603, #30802, #16970, #14193, #4849, #26781, #14399, #13785, #14606, #27198, #7202, #7826, #17805, #36586, #20577, #40211, #40417, #40003, #37007, #33185, #4436, #30601, #27407, #10586, #34024, #17183, #30182, #20788, #23564, #37207 ),
 ( #17394, #30385, #11009, #23988, #33812, #7404, #26992, #4640, #17597, #11213, #24197, #10794, #29969, #8028, #39573, #10379, #20160, #20366, #809, #33388, #4222, #1023, #13988, #23776, #36797, #32232, #5264, #40828, #22401, #6252, #3267, #18217, #41836, #32014, #28026, #22193, #11627, #28822, #37411, #24614, #22609, #8230, #37622, #41036, #25618, #32435, #12835, #9432, #1853, #11845 ),
 ( #8445, #31218, #24832, #3063, #35641, #24405, #21403, #19429, #18014, #9642, #34431, #42039, #2062, #21203, #35425, #2853, #19221, #29020, #15814, #34229, #15026, #37827, #14817, #5058, #19010, #25823, #16020, #27611, #38831, #27819, #9234, #31011, #6456, #40620, #12631, #38629, #35223, #6048, #11419, #7096, #32646, #17077, #13474, #33498, #20260, #20471, #20057, #13043, #75, #39891 ) ),
 .UNSPECIFIED., .F., .F., .T. ) 
 B_SPLINE_SURFACE_WITH_KNOTS ( ( 3, 3 ),
 ( 4, 2, 2, 2, 2, 2, 2, 2, 2, 2, 2, 2, 2, 2, 2, 2, 2, 2, 2, 2, 2, 2, 2, 2, 4 ),
 ( 0.000000000000000000, 1.000000000000000000 ),
 ( 0.000000000000000000, 0.001458241944942356878, 0.002916483889884713757, 0.005832967779769427513, 0.01166593555953885503, 0.01458241944942356878, 0.01749890333930828254, 0.01895714528425063855, 0.02041538722919299803, 0.02114450820166417777, 0.02150906868789976417, 0.02187362917413535404, 0.02223818966037094391, 0.02260275014660653031, 0.02296731063284212018, 0.02305845075440101505, 0.02310402081518046422, 0.02312680584557019053, 0.02313250210316761951, 0.02313819836076505196, 0.02314959087595991338, 0.02319516093673936255, 0.02324073099751881172, 0.02328630105829826089, 0.02333187111907771005 ),
 .UNSPECIFIED. ) 
 GEOMETRIC_REPRESENTATION_ITEM ( )  RATIONAL_B_SPLINE_SURFACE ( (
 ( 1.000000000000000000, 1.000000000000000000, 1.000000000000000000, 1.000000000000000000, 1.000000000000000000, 1.000000000000000000, 1.000000000000000000, 1.000000000000000000, 1.000000000000000000, 1.000000000000000000, 1.000000000000000000, 1.000000000000000000, 1.000000000000000000, 1.000000000000000000, 1.000000000000000000, 1.000000000000000000, 1.000000000000000000, 1.000000000000000000, 1.000000000000000000, 1.000000000000000000, 1.000000000000000000, 1.000000000000000000, 1.000000000000000000, 1.000000000000000000, 1.000000000000000000, 1.000000000000000000, 1.000000000000000000, 1.000000000000000000, 1.000000000000000000, 1.000000000000000000, 1.000000000000000000, 1.000000000000000000, 1.000000000000000000, 1.000000000000000000, 1.000000000000000000, 1.000000000000000000, 1.000000000000000000, 1.000000000000000000, 1.000000000000000000, 1.000000000000000000, 1.000000000000000000, 1.000000000000000000, 1.000000000000000000, 1.000000000000000000, 1.000000000000000000, 1.000000000000000000, 1.000000000000000000, 1.000000000000000000, 1.000000000000000000, 1.000000000000000000),
 ( 0.9987193938133603899, 0.9996013059082062835, 0.9991963860897459249, 0.9949866313572486298, 0.9909603791786357752, 0.9774858857060727546, 0.9654485462826584152, 0.9208787474394699579, 0.8807605768841590965, 0.8373543814140436137, 0.8249666374273941782, 0.8044008243570911487, 0.7962249832256278470, 0.7861950991343641393, 0.7832680976383418203, 0.7777782220923173950, 0.7752303374625654220, 0.7716286403948026118, 0.7703172242824322113, 0.7685261186013288004, 0.7673635575507736784, 0.7657163664511276169, 0.7656514573019265191, 0.7645255059884744631, 0.7630494482559035951, 0.7607147317261879760, 0.7600215756462245231, 0.7585094466923363310, 0.7575231611311871172, 0.7546848085732021927, 0.7541407386738737673, 0.7516848864309048084, 0.7509064819815688407, 0.7462986158550390936, 0.7479156148844432472, 0.7339777749606422041, 0.7233604987231169181, 0.7138238211886495099, 0.7102391262350743473, 0.6994720207877663798, 0.6929862625726375125, 0.6601362149651482936, 0.6323867238882598940, 0.5714353380975951691, 0.5388352690754523167, 0.4817946329372650993, 0.4578268140826607380, 0.4260966422721294555, 0.4180307774944384547, 0.4190531958288030157),
 ( 1.000000000000000000, 1.000000000000000000, 1.000000000000000000, 1.000000000000000000, 1.000000000000000000, 1.000000000000000000, 1.000000000000000000, 1.000000000000000000, 1.000000000000000000, 1.000000000000000000, 1.000000000000000000, 1.000000000000000000, 1.000000000000000000, 1.000000000000000000, 1.000000000000000000, 1.000000000000000000, 1.000000000000000000, 1.000000000000000000, 1.000000000000000000, 1.000000000000000000, 1.000000000000000000, 1.000000000000000000, 1.000000000000000000, 1.000000000000000000, 1.000000000000000000, 1.000000000000000000, 1.000000000000000000, 1.000000000000000000, 1.000000000000000000, 1.000000000000000000, 1.000000000000000000, 1.000000000000000000, 1.000000000000000000, 1.000000000000000000, 1.000000000000000000, 1.000000000000000000, 1.000000000000000000, 1.000000000000000000, 1.000000000000000000, 1.000000000000000000, 1.000000000000000000, 1.000000000000000000, 1.000000000000000000, 1.000000000000000000, 1.000000000000000000, 1.000000000000000000, 1.000000000000000000, 1.000000000000000000, 1.000000000000000000, 1.000000000000000000) ) ) 
 REPRESENTATION_ITEM ( '' )  SURFACE ( )  );
#39491 = CARTESIAN_POINT ( 'NONE',  ( -54.16862281694330505, 7.200593192618495841, -0.5614961770967549226 ) ) ;
#39492 = FACE_OUTER_BOUND ( 'NONE', #12110, .T. ) ;
#39493 = CARTESIAN_POINT ( 'NONE',  ( -0.4298579492383440281, 117.3993833036474825, 1.480795459422332039 ) ) ;
#39494 = DIRECTION ( 'NONE',  ( 4.017660918040594346E-17, -1.000000000000000000, -2.376309959284834438E-19 ) ) ;
#39495 = FACE_OUTER_BOUND ( 'NONE', #39884, .T. ) ;
#39496 = CARTESIAN_POINT ( 'NONE',  ( -29.27789202447384653, 65.71096991539397436, -1.523999999999142707 ) ) ;
#39497 = VECTOR ( 'NONE', #36275, 1000.000000000000000 ) ;
#39498 = CARTESIAN_POINT ( 'NONE',  ( -5.664977208693889210, 65.30181249999996851, 5.033228321271210781 ) ) ;
#39499 = CARTESIAN_POINT ( 'NONE',  ( -4.074955089416341991, 118.2429491485453354, 0.1454234154749719787 ) ) ;
#39500 = DIRECTION ( 'NONE',  ( -0.9734199927291280474, -0.2290273297124694185, -8.537024980200812943E-16 ) ) ;
#39501 = CARTESIAN_POINT ( 'NONE',  ( -58.55612285180487930, 0.6590214021355705887, 0.05016670522517701486 ) ) ;
#39502 = CARTESIAN_POINT ( 'NONE',  ( -56.26318288983030413, 4.268071985104968213, 2.480832006587838645 ) ) ;
#39503 = CARTESIAN_POINT ( 'NONE',  ( -6.918378865934497135, 117.2797055272990292, 0.1815168674402110049 ) ) ;
#39504 = EDGE_LOOP ( 'NONE', ( #7393, #19230, #9791, #36775 ) ) ;
#39505 = CARTESIAN_POINT ( 'NONE',  ( -57.89852354142710311, 2.261894840748110536, -1.235920526244146167 ) ) ;
#39506 = CARTESIAN_POINT ( 'NONE',  ( 6.065828256571993649, 121.4399732366076137, 0.1127446937255504045 ) ) ;
#39507 = ORIENTED_EDGE ( 'NONE', *, *, #36141, .T. ) ;
#39508 = DIRECTION ( 'NONE',  ( -0.9998004120163608288, 0.000000000000000000, -0.01997839162482750383 ) ) ;
#39510 = CARTESIAN_POINT ( 'NONE',  ( -8.506011814013426431, 123.3280575159016905, -0.2025880313713109560 ) ) ;
#39509 = CIRCLE ( 'NONE', #18380, 8.794749999999996959 ) ;
#39511 = CARTESIAN_POINT ( 'NONE',  ( 5.747688368404943127, -13.35872296688338245, 2.372087187842143674 ) ) ;
#39512 = CARTESIAN_POINT ( 'NONE',  ( -13.77700084449478091, 121.8522644830672590, 1.120765626652496350 ) ) ;
#39513 = CARTESIAN_POINT ( 'NONE',  ( -2.029258473809828711, 23.83235028914373288, 4.157303687431403993 ) ) ;
#39514 = CARTESIAN_POINT ( 'NONE',  ( 8.183336086940839138, 117.5993832199734328, 0.5018928202873277344 ) ) ;
#39515 = CARTESIAN_POINT ( 'NONE',  ( -17.31000046771894318, 62.32679794340116786, 1.524000000000000021 ) ) ;
#39516 = FACE_OUTER_BOUND ( 'NONE', #3010, .T. ) ;
#39517 = CARTESIAN_POINT ( 'NONE',  ( -0.6834205802178441314, -7.050398998296187436, -0.6963091382628930903 ) ) ;
#39518 = B_SPLINE_CURVE_WITH_KNOTS ( 'NONE', 3,
 ( #7391, #4001, #33801, #36994, #36575, #16750, #27393, #14182, #7815, #4208 ),
 .UNSPECIFIED., .F., .F.,
 ( 4, 2, 2, 2, 4 ),
 ( 0.007397145391538723254, 0.008407694387831694122, 0.009418243384124664122, 0.01042879238041763412, 0.01143934137671060586 ),
 .UNSPECIFIED. ) ;
#39519 = CARTESIAN_POINT ( 'NONE',  ( -4.741236776274016407, 116.7839080817633430, -0.2126559219428778014 ) ) ;
#39520 = CARTESIAN_POINT ( 'NONE',  ( -6.629500982736845120E-14, 97.88346620154572975, -1.984505748321436882E-18 ) ) ;
#39521 = CARTESIAN_POINT ( 'NONE',  ( 4.756845622061588230, 117.4019745679933067, 1.206737437952059455 ) ) ;
#39522 = ORIENTED_EDGE ( 'NONE', *, *, #19811, .T. ) ;
#39523 = CARTESIAN_POINT ( 'NONE',  ( 2.257035569276631293, 116.3299305444832612, 0.2435412801458599619 ) ) ;
#39524 = ORIENTED_EDGE ( 'NONE', *, *, #19746, .F. ) ;
#39525 = CARTESIAN_POINT ( 'NONE',  ( -17.90094693680112314, 147.7668373613703352, 1.576197898085538007 ) ) ;
#39526 = CARTESIAN_POINT ( 'NONE',  ( -57.60749290269577472, 1.353032280971704804, -1.296780305043655490 ) ) ;
#39527 = CARTESIAN_POINT ( 'NONE',  ( 19.95554629013488324, 150.7967616730061593, 2.267143661507363017 ) ) ;
#39528 = CARTESIAN_POINT ( 'NONE',  ( 19.58589350844858146, 147.2819018089465715, -1.740056086200069574 ) ) ;
#39529 = CARTESIAN_POINT ( 'NONE',  ( -0.9543378889979354796, -1.596235181177088291, 0.1924800533990675688 ) ) ;
#39530 = CARTESIAN_POINT ( 'NONE',  ( -14.57523308444403476, 121.8773232776577942, -1.525373117076484153 ) ) ;
#39531 = CARTESIAN_POINT ( 'NONE',  ( 4.590426568450723721, 118.0729213092444070, -0.5858333982661567685 ) ) ;
#39532 = CARTESIAN_POINT ( 'NONE',  ( 5.339716761587360416, 104.6144662015456959, 0.2456556763167710433 ) ) ;
#39533 = CARTESIAN_POINT ( 'NONE',  ( 16.21676096112145871, 148.3349945484709451, -1.109893536416838966 ) ) ;
#39534 = CARTESIAN_POINT ( 'NONE',  ( -5.301853325284237251, 121.3529869156830046, -0.07809170188345482266 ) ) ;
#39535 = ORIENTED_EDGE ( 'NONE', *, *, #38846, .F. ) ;
#39536 = CARTESIAN_POINT ( 'NONE',  ( -17.41382892593916765, 149.8167423968465073, -2.401583459992671976 ) ) ;
#39537 = CARTESIAN_POINT ( 'NONE',  ( 3.468122426543017500, -15.77657449013483770, 4.627414140463686820 ) ) ;
#39538 = CARTESIAN_POINT ( 'NONE',  ( -4.557708454346482085, 31.49133016986147737, -0.6947391169727166194 ) ) ;
#39539 = CARTESIAN_POINT ( 'NONE',  ( -4.578719595877105419, 118.0757894456264978, -0.7068121871710010273 ) ) ;
#39540 = AXIS2_PLACEMENT_3D ( 'NONE', #38262, #18215, #9079 ) ;
#39541 = B_SPLINE_CURVE_WITH_KNOTS ( 'NONE', 3,
 ( #10051, #12420, #38618, #32852 ),
 .UNSPECIFIED., .F., .F.,
 ( 4, 4 ),
 ( -5.999999999774938839E-08, 0.0002260494465124368644 ),
 .UNSPECIFIED. ) ;
#39542 = CARTESIAN_POINT ( 'NONE',  ( -56.82628769568140115, 4.502340570254503405, -2.499646007873257414 ) ) ;
#39543 = CARTESIAN_POINT ( 'NONE',  ( -18.83202234259777086, 80.34319284215894186, 1.269999999999995799 ) ) ;
#39544 = B_SPLINE_SURFACE_WITH_KNOTS ( 'NONE', 3, 3, ( 
 ( #38118, #9349, #9149, #19134, #31931, #2969, #15523, #22106, #19337, #5757, #12544, #35134, #5961, #18920, #2768, #32137 ),
 ( #34930, #22312, #3172, #15724, #29138, #28728, #41741, #28313, #25534, #15309, #38534, #28930, #8933, #18709, #21900, #41948 ),
 ( #12748, #25735, #38742, #31719, #28525, #41532, #12338, #41040, #11850, #5473, #11423, #40625, #21003, #34233, #8032, #2282 ),
 ( #17809, #24836, #5063, #34028, #34645, #21831, #27615, #2066, #8450, #18018, #1858, #11631, #14610, #4853, #14821, #24409 ),
 ( #37415, #24618, #8234, #8869, #41251, #37626, #30806, #31657, #31440, #12057, #21407, #15246, #25046, #21207, #1656, #27823 ),
 ( #31015, #40832, #34860, #34435, #37212, #5269, #38049, #18221, #11217, #31222, #15030, #28030, #37831, #18650, #8658, #28247 ),
 ( #21618, #18432, #5692, #2496, #15459, #28460, #24201, #25262, #16079, #32290, #32713, #35078, #22459, #29298, #39106, #22881 ),
 ( #3328, #5900, #22050, #3119, #19696, #16294, #18861, #9704, #26100, #12897, #22256, #9909, #38267, #12486, #31865, #3548 ),
 ( #35919, #19490, #28666, #29083, #2705, #15662, #2911, #32499, #16508, #142, #41466, #35281, #13108, #6729, #12273, #9084 ),
 ( #35488, #41678, #42103, #6106, #22671, #38688, #35704, #38476, #32075, #25481, #9294, #19282, #19069, #15874, #25681, #28881 ),
 ( #9494, #41893, #25885, #12691, #6310, #38892, #6515, #20117, #354, #20899, #1758, #16930, #3969, #34340, #13321, #21104 ),
 ( #4955, #14718, #26307, #24510, #8342, #768, #8130, #39317, #27720, #13745, #33140, #36128, #26738, #21310, #10123, #36542 ),
 ( #30920, #6943, #30702, #23305, #23094, #11320, #40729, #3759, #33920, #39747, #36343, #29930, #10545, #32929, #19913, #23514 ),
 ( #7360, #24309, #4750, #17703, #11529, #1552, #7158, #40528, #16717, #39531, #37314, #29515, #29721, #13537, #14507, #10336 ),
 ( #37517, #27521, #34128, #17914, #5169, #562, #26525, #36072, #39475, #6465, #35864, #22618, #12846, #3072, #32658, #23041 ),
 ( #29670, #35652, #19439, #16030, #16238, #32241, #26472, #16879, #29458, #3493, #32445, #26253, #16451, #33086, #13051, #35436 ),
 ( #39693, #39263, #29030, #19231, #29880, #297, #3277, #29241, #6677, #19643, #13269, #10069, #718, #85, #10280, #10493 ),
 ( #36285, #6889, #23251, #7105, #26042, #42051, #9857, #13692, #39052, #9650, #3917, #25831, #38841, #22827, #20065, #19857 ),
 ( #32872, #3704, #16663, #511, #26683, #13485, #6260, #40733, #927, #1557, #7934, #40325, #14514, #11118, #13900, #30925 ),
 ( #17503, #27724, #7309, #27311, #27526, #1133, #36697, #10904, #8136, #30500, #7518, #4544, #4756, #14100, #40532, #20480 ),
 ( #33298, #33506, #17708, #4337, #37114, #21109, #20905, #23462, #34134, #4960, #1343, #20695, #23677, #14299, #33719, #17919 ),
 ( #24107, #33926, #30291, #27100, #23894, #26890, #4126, #40111, #39901, #30707, #17300, #36911, #7728, #1763, #11326, #24313 ),
 ( #14723, #37320, #36489, #20269, #17086, #30087, #10697, #18127, #28146, #18970, #11748, #27935, #9194, #31132, #37522, #18336 ),
 ( #21523, #11534, #41369, #40942, #41153, #5593, #6008, #31340, #2816, #28780, #1969, #31767, #38169, #28362, #2609, #12173 ) ),
 .UNSPECIFIED., .F., .F., .F.,
 ( 4, 2, 2, 2, 2, 2, 2, 2, 2, 2, 2, 4 ),
 ( 4, 2, 2, 2, 2, 1, 1, 2, 4 ),
 ( 0.000000000000000000, 0.1320108428483948715, 0.1980162642725923072, 0.2640216856967897430, 0.3918749635278167553, 0.4558016024433302338, 0.5197282413588437677, 0.5807760813632503183, 0.6418239213676568689, 0.7639196013764699700, 0.8819598006882349850, 1.000000000000000000 ),
 ( 0.000000000000000000, 0.1250000000000000000, 0.2500000000000000000, 0.3750000000000000000, 0.5000000000000000000, 0.7500000000000000000, 0.8750000000000000000, 0.9375000000000000000, 1.000000000000000000 ),
 .UNSPECIFIED. ) ;
#39545 = CARTESIAN_POINT ( 'NONE',  ( 3.875499641586223287, 157.0187206368471209, 1.749001665105742953 ) ) ;
#39546 = LINE ( 'NONE', #17153, #37229 ) ;
#39547 = AXIS2_PLACEMENT_3D ( 'NONE', #4921, #27063, #7267 ) ;
#39548 = CARTESIAN_POINT ( 'NONE',  ( 15.73471677569731142, 120.8416612192341972, 0.3144170877231854955 ) ) ;
#39549 = CARTESIAN_POINT ( 'NONE',  ( -8.291425676780491472, 12.16085651096402032, -1.523321141447528948 ) ) ;
#39550 = CARTESIAN_POINT ( 'NONE',  ( 0.6714861817527252308, 156.3445873232922736, 0.4416347707370367748 ) ) ;
#39551 = CARTESIAN_POINT ( 'NONE',  ( 7.717559979892206989, 158.5863655655865330, -0.7470610436598875692 ) ) ;
#39552 = CARTESIAN_POINT ( 'NONE',  ( 2.948382749353823495, 50.63946620154572997, 1.837270642369387641 ) ) ;
#39553 = VERTEX_POINT ( 'NONE', #34897 ) ;
#39554 = CARTESIAN_POINT ( 'NONE',  ( -5.591489108514605455, 77.73497692594764885, 1.270000000000003126 ) ) ;
#39555 = CARTESIAN_POINT ( 'NONE',  ( -10.83072783392024618, 157.9016520041087688, -0.1964268902508805315 ) ) ;
#39556 = ORIENTED_EDGE ( 'NONE', *, *, #1982, .F. ) ;
#39557 = CARTESIAN_POINT ( 'NONE',  ( 8.137137598917451697, 121.0224714142185718, -1.005786695753826621 ) ) ;
#39558 = DIRECTION ( 'NONE',  ( -5.188838149069471174E-16, 1.699382548006136313E-16, 1.000000000000000000 ) ) ;
#39559 = CARTESIAN_POINT ( 'NONE',  ( -15.83982646870426336, 146.6055793175013093, -0.7699162700945604287 ) ) ;
#39560 = CARTESIAN_POINT ( 'NONE',  ( 2.629318991877339418, -14.82094413389492615, 5.549789958447211013 ) ) ;
#39561 = CARTESIAN_POINT ( 'NONE',  ( -15.72870526381844591, 122.9504679175852573, 0.8738493638518138873 ) ) ;
#39562 = CARTESIAN_POINT ( 'NONE',  ( -30.44847906516384128, 70.61110078258337808, 1.269999999999991580 ) ) ;
#39563 = TOROIDAL_SURFACE ( 'NONE', #3504, 3.683000000000000718, 0.5080000000000000071 ) ;
#39564 = CARTESIAN_POINT ( 'NONE',  ( 21.90252518039352836, 151.4352167165723415, 0.5139180553509253846 ) ) ;
#39565 = VERTEX_POINT ( 'NONE', #11887 ) ;
#39566 = CARTESIAN_POINT ( 'NONE',  ( 1.961646697876492373, -0.1315482170498871728, -4.191205975169975950 ) ) ;
#39567 = DIRECTION ( 'NONE',  ( -0.8745520943968245753, 0.4849315768086539524, -5.691349986800526185E-16 ) ) ;
#39568 = DIRECTION ( 'NONE',  ( 0.9998004120163610509, 4.016384292689131511E-17, 0.01997839162482749689 ) ) ;
#39569 = CARTESIAN_POINT ( 'NONE',  ( -17.14500000000466784, 71.11999999999886768, -1.524000000000000909 ) ) ;
#39570 = CARTESIAN_POINT ( 'NONE',  ( 4.826677069784417462, 119.0088915937735123, 1.091954489690918351 ) ) ;
#39571 = CARTESIAN_POINT ( 'NONE',  ( 4.628409624684510781, -5.919234854628784959, 0.1277143096542201761 ) ) ;
#39572 = CARTESIAN_POINT ( 'NONE',  ( 3.924194517545410932, 117.4679918459733585, 0.7389123598820265260 ) ) ;
#39573 = CARTESIAN_POINT ( 'NONE',  ( -56.62423581747610513, 3.520748359631705515, -2.300294558596477135 ) ) ;
#39575 = CARTESIAN_POINT ( 'NONE',  ( 10.41147150295383739, 120.1444133044471556, -1.103258690517171514 ) ) ;
#39574 = DIRECTION ( 'NONE',  ( -0.8745520943968663197, 0.4849315768085789013, -5.691349986800499561E-16 ) ) ;
#39576 = AXIS2_PLACEMENT_3D ( 'NONE', #32548, #22518, #32770 ) ;
#39577 = CARTESIAN_POINT ( 'NONE',  ( -0.4757704999385121702, -3.320450887815510121, -4.596079559024887295 ) ) ;
#39578 = CARTESIAN_POINT ( 'NONE',  ( -22.70157303802179882, 149.4207734315791072, -1.531927632650241566 ) ) ;
#39579 = VERTEX_POINT ( 'NONE', #8695 ) ;
#39580 = CARTESIAN_POINT ( 'NONE',  ( -9.439772580079139885, 124.2753396726362780, 0.1368060863603348387 ) ) ;
#39581 = CARTESIAN_POINT ( 'NONE',  ( 5.379018416755689813, -14.82644845813459256, 3.481186560222681692 ) ) ;
#39582 = AXIS2_PLACEMENT_3D ( 'NONE', #23436, #901, #17061 ) ;
#39583 = CARTESIAN_POINT ( 'NONE',  ( -43.35906100199910185, 21.49635880980142133, 2.252931129856620363 ) ) ;
#39584 = CARTESIAN_POINT ( 'NONE',  ( -3.402419904042699006, 108.3861669196250688, -4.099931217281246987 ) ) ;
#39585 = ORIENTED_EDGE ( 'NONE', *, *, #22386, .F. ) ;
#39586 = CARTESIAN_POINT ( 'NONE',  ( 1.237267194679675164, 118.7146927282448132, 0.6928808259403734793 ) ) ;
#39587 = CARTESIAN_POINT ( 'NONE',  ( -5.106395947886140263, 78.95054594174945350, 1.904999999999988258 ) ) ;
#39588 = CARTESIAN_POINT ( 'NONE',  ( -10.32169608105474090, 17.14500000000000313, -4.040823496909975887 ) ) ;
#39589 = CIRCLE ( 'NONE', #34813, 12.69999999999999751 ) ;
#39590 = AXIS2_PLACEMENT_3D ( 'NONE', #9879, #29482, #7130 ) ;
#39591 = CARTESIAN_POINT ( 'NONE',  ( -12.83198513809782604, 156.8686255264331635, 0.8772202223719094416 ) ) ;
#39592 = CARTESIAN_POINT ( 'NONE',  ( 3.683590692373001296, 21.29142263786511080, 7.571256661570916258 ) ) ;
#39593 = EDGE_CURVE ( 'NONE', #36869, #13695, #29247, .T. ) ;
#39594 = CARTESIAN_POINT ( 'NONE',  ( 9.710114326862120393, 153.9716628027005925, 1.336640340121901582 ) ) ;
#39595 = CARTESIAN_POINT ( 'NONE',  ( 0.9570688389943262653, 116.7004868406603322, -0.2253703713229211203 ) ) ;
#39596 = DIRECTION ( 'NONE',  ( -5.188838149069472160E-16, 1.699382548006136559E-16, 1.000000000000000000 ) ) ;
#39597 = CARTESIAN_POINT ( 'NONE',  ( -46.75240110268729410, 25.86707425373576541, 1.404788063146650501 ) ) ;
#39598 = CARTESIAN_POINT ( 'NONE',  ( -48.35963184368405621, 21.82761434182101112, 2.838462189984248596 ) ) ;
#39599 = CARTESIAN_POINT ( 'NONE',  ( 1.400628584307200167E-15, 13.84300000000000352, 0.000000000000000000 ) ) ;
#39600 = CARTESIAN_POINT ( 'NONE',  ( -51.58367816905025194, 14.91232437457545146, 4.609044670965822377 ) ) ;
#39601 = CARTESIAN_POINT ( 'NONE',  ( -58.59183231654615298, -0.2159720215225674478, 0.4817266061078952499 ) ) ;
#39602 = CARTESIAN_POINT ( 'NONE',  ( -4.535200515210230598, 118.1197139754325036, 0.4752115866934419897 ) ) ;
#39603 = DIRECTION ( 'NONE',  ( -1.000000000000000000, 0.000000000000000000, 0.000000000000000000 ) ) ;
#39604 = VERTEX_POINT ( 'NONE', #15697 ) ;
#39605 = CARTESIAN_POINT ( 'NONE',  ( -45.14658554404967106, 22.88857079803865346, 2.562886992506556272 ) ) ;
#39606 = CARTESIAN_POINT ( 'NONE',  ( -8.295186191818521237, 120.0125017958713727, -1.449258406794112997 ) ) ;
#39607 = CARTESIAN_POINT ( 'NONE',  ( -5.194452014863664147, 116.1170857923940787, -1.235891685093609915 ) ) ;
#39608 = CARTESIAN_POINT ( 'NONE',  ( 4.503786011748764473, 118.0871167092629577, 0.7873725921291204743 ) ) ;
#39609 = CARTESIAN_POINT ( 'NONE',  ( -5.869717882709328372, 121.2452591720019370, -0.5958057796325608724 ) ) ;
#39610 = CARTESIAN_POINT ( 'NONE',  ( -0.7572052446267691916, 115.7028915209885014, -1.755553211052053975 ) ) ;
#39611 = CARTESIAN_POINT ( 'NONE',  ( 3.212429978159830668, 117.3993812122530329, -1.261639093947187540 ) ) ;
#39612 = CARTESIAN_POINT ( 'NONE',  ( 4.518882305193341331, 111.2411499886600268, -2.961292089698490226 ) ) ;
#39613 = CARTESIAN_POINT ( 'NONE',  ( -10.46581596931682689, 123.6668265419868646, -1.337773356492248489 ) ) ;
#39614 = CARTESIAN_POINT ( 'NONE',  ( 5.243110457265114377, 104.6144662015457527, 1.505012106405181127 ) ) ;
#39615 = CARTESIAN_POINT ( 'NONE',  ( -3.009276887026423264, 50.13146620154573441, 1.210121013456480377 ) ) ;
#39616 = CARTESIAN_POINT ( 'NONE',  ( -7.213960532367465817, 78.77618639008778700, -1.904999999999999583 ) ) ;
#39617 = CARTESIAN_POINT ( 'NONE',  ( -11.83383823350433772, 152.0554358120322149, -0.04909464509748200090 ) ) ;
#39618 = CARTESIAN_POINT ( 'NONE',  ( -2.424025297795170619, -5.104216246930970868, 3.935102955759355758 ) ) ;
#39619 = CARTESIAN_POINT ( 'NONE',  ( 14.21090189159854056, 120.4756499382577886, 1.027290292067533306 ) ) ;
#39620 = CARTESIAN_POINT ( 'NONE',  ( -23.62918761621517305, 82.45577215708875940, -1.524000000000006017 ) ) ;
#39621 = CARTESIAN_POINT ( 'NONE',  ( 2.572675278006325339, -15.15086880438208716, 4.677806725582212444 ) ) ;
#39622 = CARTESIAN_POINT ( 'NONE',  ( -10.22873863908719194, 155.5514087735115822, 1.732306429912916945 ) ) ;
#39623 = CARTESIAN_POINT ( 'NONE',  ( -0.8939936458071766623, -10.86866097718376523, 0.3889025406916932770 ) ) ;
#39624 = CARTESIAN_POINT ( 'NONE',  ( -4.790162199822132649, 116.9482543694763166, -0.4383784235352165548 ) ) ;
#39625 = AXIS2_PLACEMENT_3D ( 'NONE', #2421, #25603, #5403 ) ;
#39626 = CARTESIAN_POINT ( 'NONE',  ( 0.5584349385955980072, -2.506542431320444742, 0.8015440831694167212 ) ) ;
#39627 = ADVANCED_FACE ( 'NONE', ( #39140 ), #39893, .T. ) ;
#39628 = ORIENTED_EDGE ( 'NONE', *, *, #27602, .F. ) ;
#39629 = CARTESIAN_POINT ( 'NONE',  ( -47.61549956331939626, 19.66157307908737195, 5.197827534590555132 ) ) ;
#39630 = CARTESIAN_POINT ( 'NONE',  ( 4.571503503190692541, 114.7252160460498516, 1.874454982749236498 ) ) ;
#39631 = CARTESIAN_POINT ( 'NONE',  ( -0.005430166084385830948, 120.5648899400503069, 0.2717477157510632124 ) ) ;
#39632 = CARTESIAN_POINT ( 'NONE',  ( 4.240324834746892257, -11.68880992198167945, 0.6883502328505933798 ) ) ;
#39633 = CARTESIAN_POINT ( 'NONE',  ( 0.02768739821002418749, 156.9833357668885014, -1.385590625008458865 ) ) ;
#39634 = CARTESIAN_POINT ( 'NONE',  ( -12.11054887026069871, 155.0146010091537221, -2.232606363771872715 ) ) ;
#39635 = CARTESIAN_POINT ( 'NONE',  ( 4.808131379915037584, 104.6144662015457527, -0.4149153341867691802 ) ) ;
#39636 = CARTESIAN_POINT ( 'NONE',  ( 3.115274840615241292, -13.78277351762104175, 1.693892316854531455 ) ) ;
#39637 = CARTESIAN_POINT ( 'NONE',  ( -4.757248700571870437, 117.4032733054477688, -1.206458840171575009 ) ) ;
#39638 = CARTESIAN_POINT ( 'NONE',  ( 12.97778284513260694, 133.8854804328748571, 0.04088747601382877045 ) ) ;
#39639 = VECTOR ( 'NONE', #2872, 1000.000000000000000 ) ;
#39640 = ORIENTED_EDGE ( 'NONE', *, *, #4211, .T. ) ;
#39641 = FACE_OUTER_BOUND ( 'NONE', #26922, .T. ) ;
#39642 = CARTESIAN_POINT ( 'NONE',  ( 2.545864362986065110, 107.1172351171714467, 4.679951533430918964 ) ) ;
#39643 = DIRECTION ( 'NONE',  ( 0.9998004120163609398, 4.016384292689130894E-17, 0.01997839162482749689 ) ) ;
#39644 = EDGE_CURVE ( 'NONE', #15945, #20056, #15334, .T. ) ;
#39645 = CARTESIAN_POINT ( 'NONE',  ( -10.55305098051677426, 77.31887769575739355, 1.269999999999999796 ) ) ;
#39646 = CARTESIAN_POINT ( 'NONE',  ( 0.8998519745135501458, 116.4604358222411236, -0.05108568132534201112 ) ) ;
#39647 = CARTESIAN_POINT ( 'NONE',  ( -2.677032024553447798, 107.2224589468338536, 4.627058715154634960 ) ) ;
#39648 = TOROIDAL_SURFACE ( 'NONE', #37592, 4.826000000000000512, 0.5080000000000000071 ) ;
#39649 = CARTESIAN_POINT ( 'NONE',  ( 1.753509963957065043, -15.55925396411267414, 5.871249478519287912 ) ) ;
#39650 = DIRECTION ( 'NONE',  ( 9.627370216492862708E-17, 1.000000000000000000, -0.000000000000000000 ) ) ;
#39651 = CARTESIAN_POINT ( 'NONE',  ( 1.766327495819737248, 37.59738145967928347, -1.135536361765588032 ) ) ;
#39652 = EDGE_CURVE ( 'NONE', #13978, #26949, #25712, .T. ) ;
#39653 = CARTESIAN_POINT ( 'NONE',  ( 20.63667788919575585, 149.2407879669073054, 2.389545083207231357 ) ) ;
#39654 = CARTESIAN_POINT ( 'NONE',  ( -4.621355134897683570, 27.56591289442953041, -0.4301045952606497025 ) ) ;
#39655 = CARTESIAN_POINT ( 'NONE',  ( -8.175057852536518510, 12.81247082500981094, 2.033924511151908199 ) ) ;
#39656 = CARTESIAN_POINT ( 'NONE',  ( -5.501858137863374409, 117.7715637320503674, -1.036254152625051939 ) ) ;
#39657 = CARTESIAN_POINT ( 'NONE',  ( -2.813253328531210240, 121.9077826007922312, -0.2952959765298339700 ) ) ;
#39658 = CARTESIAN_POINT ( 'NONE',  ( 4.941661011542251458, 117.4083430605341647, 1.067727440994704624 ) ) ;
#39659 = CARTESIAN_POINT ( 'NONE',  ( -17.14500000000466784, 71.11999999999886768, -1.524000000000000909 ) ) ;
#39660 = CARTESIAN_POINT ( 'NONE',  ( -5.018858541180816424, 105.1216645147153343, 1.817098519714964278 ) ) ;
#39661 = AXIS2_PLACEMENT_3D ( 'NONE', #17413, #1258, #27014 ) ;
#39662 = CARTESIAN_POINT ( 'NONE',  ( 2.003160574663116034, 15.61121511114846960, 4.187759092076685619 ) ) ;
#39663 = CARTESIAN_POINT ( 'NONE',  ( 5.008145224984434485, 117.3993836135855418, -0.7758584094373792706 ) ) ;
#39664 = FACE_OUTER_BOUND ( 'NONE', #20377, .T. ) ;
#39665 = CARTESIAN_POINT ( 'NONE',  ( 3.317891647977158076, -14.03051783662405327, 3.455980060616059113 ) ) ;
#39666 = CARTESIAN_POINT ( 'NONE',  ( 3.444826702830371179, 112.1633951907056996, -2.719597167543061023 ) ) ;
#39667 = CARTESIAN_POINT ( 'NONE',  ( -22.95957815304936744, 148.8788797244430384, 0.5134943257494379854 ) ) ;
#39668 = VECTOR ( 'NONE', #14419, 1000.000000000000114 ) ;
#39669 = CARTESIAN_POINT ( 'NONE',  ( 4.976314832089088647, 117.4086780430578045, -0.8840892738920966831 ) ) ;
#39670 = ORIENTED_EDGE ( 'NONE', *, *, #41253, .F. ) ;
#39671 = CARTESIAN_POINT ( 'NONE',  ( -3.841520934845505941, 71.62889921741444255, -1.269999999999994023 ) ) ;
#39672 = ORIENTED_EDGE ( 'NONE', *, *, #11339, .F. ) ;
#39673 = DIRECTION ( 'NONE',  ( -4.017660918040594346E-17, 1.000000000000000000, 2.376309959284834438E-19 ) ) ;
#39674 = CARTESIAN_POINT ( 'NONE',  ( 5.328887433758706216, -15.24262819705347916, -0.4233796293290443269 ) ) ;
#39675 = CARTESIAN_POINT ( 'NONE',  ( -15.41274837478120574, 125.4902479783272184, 1.384083614372567661 ) ) ;
#39676 = CARTESIAN_POINT ( 'NONE',  ( 4.003603038177849349, 117.7793252414215317, -0.6798483224588709462 ) ) ;
#39677 = CARTESIAN_POINT ( 'NONE',  ( 2.294499597581835193, -9.852027417895397932, -4.012603411698490774 ) ) ;
#39678 = EDGE_CURVE ( 'NONE', #12920, #26767, #20109, .T. ) ;
#39679 = CARTESIAN_POINT ( 'NONE',  ( -58.52263300247899735, -0.06897136332623234056, -0.6413478136646119099 ) ) ;
#39680 = VERTEX_POINT ( 'NONE', #25297 ) ;
#39681 = CARTESIAN_POINT ( 'NONE',  ( -4.970811386520536779, 117.4009602783328461, -0.9886943268754924130 ) ) ;
#39682 = CARTESIAN_POINT ( 'NONE',  ( 1.907654281882038783, 121.7602717223048501, 0.3165470008995036055 ) ) ;
#39683 = CARTESIAN_POINT ( 'NONE',  ( -8.983288137945276475, 154.9128698100208794, 1.355969927742461723 ) ) ;
#39684 = CARTESIAN_POINT ( 'NONE',  ( -6.176553856875742987, 28.68700468106497681, 0.2098252341470465687 ) ) ;
#39685 = EDGE_CURVE ( 'NONE', #33497, #40327, #12931, .T. ) ;
#39686 = CARTESIAN_POINT ( 'NONE',  ( 12.93728320859306358, 153.8477531742089468, -1.710492906883537945 ) ) ;
#39687 = AXIS2_PLACEMENT_3D ( 'NONE', #33222, #5096, #1689 ) ;
#39688 = CARTESIAN_POINT ( 'NONE',  ( -4.941607502190771939, 118.3881331334009985, -1.039683250452205776 ) ) ;
#39689 = CARTESIAN_POINT ( 'NONE',  ( -29.50431010628811990, 60.44740661353770150, -1.524000000000005350 ) ) ;
#39690 = CIRCLE ( 'NONE', #21277, 3.175000000000001155 ) ;
#39691 = EDGE_CURVE ( 'NONE', #17404, #40141, #41488, .T. ) ;
#39692 = ORIENTED_EDGE ( 'NONE', *, *, #20710, .T. ) ;
#39693 = CARTESIAN_POINT ( 'NONE',  ( 4.459699206147334394, 118.1245879234415526, -0.5577549297624452285 ) ) ;
#39694 = CARTESIAN_POINT ( 'NONE',  ( 11.61789020275260320, 128.2970750771678752, -0.3952796010287947803 ) ) ;
#39695 = EDGE_LOOP ( 'NONE', ( #8764, #34495, #15219, #5790 ) ) ;
#39696 = CARTESIAN_POINT ( 'NONE',  ( 3.393951437975996743, -15.00105261681208901, 2.580228093083809071 ) ) ;
#39697 = DIRECTION ( 'NONE',  ( 5.188838149069472160E-16, -1.699382548006136559E-16, -1.000000000000000000 ) ) ;
#39698 = CIRCLE ( 'NONE', #37641, 3.683000000000001162 ) ;
#39699 = CARTESIAN_POINT ( 'NONE',  ( -48.15927431541864223, 19.02058896282273182, 5.220430799429900404 ) ) ;
#39700 = CARTESIAN_POINT ( 'NONE',  ( 2.245307460665866728, 11.68515688572553479, 4.070821060848484940 ) ) ;
#39701 = CARTESIAN_POINT ( 'NONE',  ( 16.78017617680110618, 148.3581316477378493, 2.036619618061131121 ) ) ;
#39702 = CARTESIAN_POINT ( 'NONE',  ( -1.922869785242472762, 31.26939154837774026, 1.580357446662301157 ) ) ;
#39703 = CARTESIAN_POINT ( 'NONE',  ( 1.616848224653315569, 9.589005055319924864, -4.350374724214612243 ) ) ;
#39704 = CARTESIAN_POINT ( 'NONE',  ( 0.6369907463661377278, 120.9735524437166561, 0.07606544612864254984 ) ) ;
#39705 = DIRECTION ( 'NONE',  ( -0.01997839162482761832, -1.040247600000950455E-18, 0.9998004120163610509 ) ) ;
#39706 = CARTESIAN_POINT ( 'NONE',  ( -50.84949806483948720, 11.71728973011883923, -8.857595425233459675E-15 ) ) ;
#39707 = CARTESIAN_POINT ( 'NONE',  ( 5.550207450195033587, 116.8112513961327608, -0.2456669984780832650 ) ) ;
#39708 = DIRECTION ( 'NONE',  ( -0.8745520943968241312, 0.4849315768086548406, -5.691349986800536046E-16 ) ) ;
#39709 = AXIS2_PLACEMENT_3D ( 'NONE', #3103, #16064, #9687 ) ;
#39710 = CARTESIAN_POINT ( 'NONE',  ( -46.91299662966074635, 25.29696379526928496, -1.775053009676189397 ) ) ;
#39711 = CARTESIAN_POINT ( 'NONE',  ( -48.41349243880052455, 18.68090591540773460, 5.201624795074226704 ) ) ;
#39712 = CARTESIAN_POINT ( 'NONE',  ( -29.12312633939021822, 66.61190372955286421, -1.524000000000005350 ) ) ;
#39713 = CARTESIAN_POINT ( 'NONE',  ( -5.664977208693889210, 53.58606250000000415, 5.033228321271210781 ) ) ;
#39714 = CARTESIAN_POINT ( 'NONE',  ( -5.322311913656985638, 57.15000000000021174, 5.239113282063311949 ) ) ;
#39715 = CARTESIAN_POINT ( 'NONE',  ( -21.91949108387693812, 59.24500507708427932, 1.523999999999998245 ) ) ;
#39716 = CARTESIAN_POINT ( 'NONE',  ( -57.92473815682701144, 2.127617342915319565, 1.480748064241587114 ) ) ;
#39717 = CARTESIAN_POINT ( 'NONE',  ( -58.09657527255103560, 0.9821181129459344294, 1.359330230256424521 ) ) ;
#39718 = CARTESIAN_POINT ( 'NONE',  ( -15.48609530480959862, 120.8153160915142337, 0.009749853210865312356 ) ) ;
#39719 = VECTOR ( 'NONE', #27831, 1000.000000000000114 ) ;
#39720 = ADVANCED_FACE ( 'NONE', ( #9739 ), #22082, .T. ) ;
#39721 = ORIENTED_EDGE ( 'NONE', *, *, #12223, .F. ) ;
#39722 = CARTESIAN_POINT ( 'NONE',  ( -57.36672490206960617, 3.909939030509804070, -0.6468086288197882894 ) ) ;
#39723 = CARTESIAN_POINT ( 'NONE',  ( -6.061911998292836223, 121.4331685367002507, -0.1225658242750968657 ) ) ;
#39724 = ORIENTED_EDGE ( 'NONE', *, *, #20565, .F. ) ;
#39725 = FACE_OUTER_BOUND ( 'NONE', #11087, .T. ) ;
#39726 = CARTESIAN_POINT ( 'NONE',  ( -4.223292309265045397, 155.8535809751167562, -0.1210084730045378199 ) ) ;
#39727 = CARTESIAN_POINT ( 'NONE',  ( 5.718287093813156474, -14.23487671053640113, 2.942044405997081391 ) ) ;
#39728 = CARTESIAN_POINT ( 'NONE',  ( -4.957730756931507443, 118.1424809852657773, 0.7901079947696818540 ) ) ;
#39729 = CARTESIAN_POINT ( 'NONE',  ( 2.163044864548389512, 28.58015952483584599, -4.087059112497700042 ) ) ;
#39730 = CIRCLE ( 'NONE', #22020, 0.2540000000000027236 ) ;
#39731 = CARTESIAN_POINT ( 'NONE',  ( 13.33768363058602091, 156.9675713949798421, 0.6438986485269785343 ) ) ;
#39732 = CARTESIAN_POINT ( 'NONE',  ( 5.933371281133245745, 155.4177045500023553, 0.2751541236311783600 ) ) ;
#39733 = DIRECTION ( 'NONE',  ( 0.8138664877804109299, 0.5810519254489895369, 0.000000000000000000 ) ) ;
#39734 = CARTESIAN_POINT ( 'NONE',  ( 0.8978640518332915432, -1.652899491467043180, 0.3817720442996600516 ) ) ;
#39735 = CARTESIAN_POINT ( 'NONE',  ( -16.80483327138728455, 155.2524275687165982, -0.6336504121414450186 ) ) ;
#39736 = DIRECTION ( 'NONE',  ( 5.188838149069472160E-16, -1.699382548006136559E-16, -1.000000000000000000 ) ) ;
#39737 = FACE_OUTER_BOUND ( 'NONE', #39191, .T. ) ;
#39738 = ORIENTED_EDGE ( 'NONE', *, *, #8763, .F. ) ;
#39739 = CARTESIAN_POINT ( 'NONE',  ( 8.777645125800189518, 117.7559043064407831, 0.4625451175356548039 ) ) ;
#39740 = CARTESIAN_POINT ( 'NONE',  ( -18.00062125403734115, 147.1528319293316542, 1.577578161537398493 ) ) ;
#39741 = CARTESIAN_POINT ( 'NONE',  ( -58.21675469219344734, 0.03542984183141312249, -0.5229180514795568335 ) ) ;
#39742 = CARTESIAN_POINT ( 'NONE',  ( 15.09010836182842219, 154.7927800759015042, 2.085168164864714679 ) ) ;
#39743 = CARTESIAN_POINT ( 'NONE',  ( 19.82182223277781574, 148.2167131080949787, -1.724547319354139407 ) ) ;
#39744 = VECTOR ( 'NONE', #320, 1000.000000000000000 ) ;
#39745 = CARTESIAN_POINT ( 'NONE',  ( 0.2779342515209439202, -14.33719732021959636, -0.9356842789569203012 ) ) ;
#39746 = CARTESIAN_POINT ( 'NONE',  ( -10.62690833282013259, 119.8050749133877275, -1.415659332795228043 ) ) ;
#39747 = CARTESIAN_POINT ( 'NONE',  ( 4.631749536040931758, 118.0396149105038148, -0.6219378133418650423 ) ) ;
#39748 = CARTESIAN_POINT ( 'NONE',  ( -46.67659519887700981, 22.71018310752411651, -3.598098858967615055 ) ) ;
#39749 = ADVANCED_FACE ( 'NONE', ( #39352 ), #10372, .T. ) ;
#39750 = CARTESIAN_POINT ( 'NONE',  ( 5.314256983240369436, 105.1224655745845240, -0.4585143440169748841 ) ) ;
#39751 = EDGE_CURVE ( 'NONE', #21991, #3203, #5181, .T. ) ;
#39752 = CARTESIAN_POINT ( 'NONE',  ( 16.69554899298717032, 147.2809512400332608, -1.108146210772844587 ) ) ;
#39753 = CARTESIAN_POINT ( 'NONE',  ( -4.949223898456546422, 117.6231127316777645, 0.7510713373028163886 ) ) ;
#39754 = ORIENTED_EDGE ( 'NONE', *, *, #32552, .F. ) ;
#39755 = CARTESIAN_POINT ( 'NONE',  ( -10.55536611456385110, 121.9340018749941663, -1.633389464556823878 ) ) ;
#39756 = CARTESIAN_POINT ( 'NONE',  ( 2.260827880841108417, -15.68886294521955271, 5.354637041555423416 ) ) ;
#39757 = AXIS2_PLACEMENT_3D ( 'NONE', #6718, #6504, #553 ) ;
#39758 = CARTESIAN_POINT ( 'NONE',  ( -5.208855653336853742, 31.38455280743060527, -0.6720767434146608377 ) ) ;
#39759 = CARTESIAN_POINT ( 'NONE',  ( -4.638992326972686264, 118.0266412661314916, -0.7607261125604591889 ) ) ;
#39760 = CARTESIAN_POINT ( 'NONE',  ( -52.76912830878634253, 12.08540908813377612, -4.334427935445254398 ) ) ;
#39761 = CARTESIAN_POINT ( 'NONE',  ( 4.105707650416926313, 118.2429491485453354, 0.3526241214267462065 ) ) ;
#39762 = CARTESIAN_POINT ( 'NONE',  ( 3.977359857054884262, 157.1622345443605582, 1.793852766001656551 ) ) ;
#39763 = CARTESIAN_POINT ( 'NONE',  ( -3.630816577625875226E-14, 57.14999999999999147, 0.000000000000000000 ) ) ;
#39764 = CARTESIAN_POINT ( 'NONE',  ( 13.69580498508134347, 119.6466660129326272, 0.2573648061928516806 ) ) ;
#39765 = CIRCLE ( 'NONE', #5070, 0.6349999999999977884 ) ;
#39766 = CARTESIAN_POINT ( 'NONE',  ( -6.929632415086860675, 11.50928017261270497, -4.815005168835179816 ) ) ;
#39767 = CARTESIAN_POINT ( 'NONE',  ( 15.47370139510873877, 143.5853813351167219, 1.046079274478294296 ) ) ;
#39768 = CARTESIAN_POINT ( 'NONE',  ( 12.95464425824995836, 119.9671592456446803, -0.6090756887631914029 ) ) ;
#39769 = DIRECTION ( 'NONE',  ( -0.9998004120163608288, 0.000000000000000000, -0.01997839162482749342 ) ) ;
#39770 = ORIENTED_EDGE ( 'NONE', *, *, #12821, .T. ) ;
#39771 = DIRECTION ( 'NONE',  ( -0.9998004120163609398, -4.016384292689130894E-17, -0.01997839162482749689 ) ) ;
#39772 = CARTESIAN_POINT ( 'NONE',  ( -15.65715779584560607, 120.8241032224722176, -0.2083191676592778541 ) ) ;
#39773 = VERTEX_POINT ( 'NONE', #4430 ) ;
#39774 = CARTESIAN_POINT ( 'NONE',  ( -5.444022911906507112, 120.6653284619048350, -0.7521495152940341766 ) ) ;
#39775 = CARTESIAN_POINT ( 'NONE',  ( -8.644792878687130866, 118.5213301182957366, 0.7512959218659897020 ) ) ;
#39776 = ORIENTED_EDGE ( 'NONE', *, *, #33934, .F. ) ;
#39777 = CARTESIAN_POINT ( 'NONE',  ( 15.50061618130081165, 62.14374591690594940, -1.904999999999999583 ) ) ;
#39778 = CARTESIAN_POINT ( 'NONE',  ( -15.89665129872327576, 146.6311637152522565, -0.9120559015848336282 ) ) ;
#39779 = CARTESIAN_POINT ( 'NONE',  ( 3.638845723804262189, -14.60113053194242383, 5.212470003951681363 ) ) ;
#39780 = CARTESIAN_POINT ( 'NONE',  ( -17.77240244235150257, 153.9999837190418930, 1.018827867329159753 ) ) ;
#39781 = CARTESIAN_POINT ( 'NONE',  ( -14.67500508080565780, 148.8517222229471315, -0.2932415260855779637 ) ) ;
#39782 = CARTESIAN_POINT ( 'NONE',  ( 23.28768492013411873, 149.3500807853454546, 0.5424486132203802935 ) ) ;
#39783 = VERTEX_POINT ( 'NONE', #37001 ) ;
#39784 = CARTESIAN_POINT ( 'NONE',  ( 3.064284189169764971, -3.155149710853871525, 3.465721614369133174 ) ) ;
#39785 = CARTESIAN_POINT ( 'NONE',  ( -6.439802422954663176E-14, 159.6054662015457382, 9.942593405483322146E-17 ) ) ;
#39786 = DIRECTION ( 'NONE',  ( 3.035386659626960118E-16, -0.000000000000000000, 1.000000000000000000 ) ) ;
#39787 = DIRECTION ( 'NONE',  ( 9.627370216492862708E-17, 1.000000000000000000, -0.000000000000000000 ) ) ;
#39788 = CARTESIAN_POINT ( 'NONE',  ( 6.829987328009752723, 120.5672262496176614, 1.156243076138642634 ) ) ;
#39789 = EDGE_CURVE ( 'NONE', #25364, #20581, #14526, .T. ) ;
#39790 = CARTESIAN_POINT ( 'NONE',  ( -4.627572956979934204, -1.171460759993483869, -0.2796867628226345492 ) ) ;
#39791 = CARTESIAN_POINT ( 'NONE',  ( 3.898539657838472561, 117.3164332630744298, 0.6789226234856292619 ) ) ;
#39792 = CARTESIAN_POINT ( 'NONE',  ( -57.79860935920169851, 1.496589803104450667, -1.561213607913327639 ) ) ;
#39794 = CARTESIAN_POINT ( 'NONE',  ( 0.01081828485854949978, 118.1092738308834669, -0.5413912121690739321 ) ) ;
#39793 = DIRECTION ( 'NONE',  ( -5.188838149069472160E-16, 1.699382548006136559E-16, 1.000000000000000000 ) ) ;
#39795 = CARTESIAN_POINT ( 'NONE',  ( 4.264856162967361364, -5.269518785209044154, -1.792273654951743067 ) ) ;
#39796 = CARTESIAN_POINT ( 'NONE',  ( -22.22941764614908422, 150.1947564971097222, -1.617977611002929583 ) ) ;
#39797 = B_SPLINE_CURVE_WITH_KNOTS ( 'NONE', 3,
 ( #8584, #28174, #21547, #24541 ),
 .UNSPECIFIED., .F., .F.,
 ( 4, 4 ),
 ( 0.4905041263739763346, 1.000000000000000000 ),
 .UNSPECIFIED. ) ;
#39798 = EDGE_CURVE ( 'NONE', #4652, #359, #39449, .T. ) ;
#39799 = ORIENTED_EDGE ( 'NONE', *, *, #25155, .F. ) ;
#39800 = CARTESIAN_POINT ( 'NONE',  ( -9.391698128492089737, 124.2036136473707018, 0.1363215471561609049 ) ) ;
#39801 = CARTESIAN_POINT ( 'NONE',  ( 6.240488881946434141, -13.64759869265259873, 1.419018975165988294 ) ) ;
#39802 = DIRECTION ( 'NONE',  ( -0.4849315768086535083, -0.8745520943968250194, -1.030032898892974695E-16 ) ) ;
#39803 = CARTESIAN_POINT ( 'NONE',  ( -3.935359235824978708, 109.5187692929153656, -3.609514305193955774 ) ) ;
#39804 = ORIENTED_EDGE ( 'NONE', *, *, #20228, .F. ) ;
#39805 = CARTESIAN_POINT ( 'NONE',  ( 0.9995654073148593222, 157.9544661020348997, 1.649992931013676500 ) ) ;
#39806 = DIRECTION ( 'NONE',  ( -0.9998004120163609398, -4.016384292689130894E-17, -0.01997839162482749689 ) ) ;
#39807 = CARTESIAN_POINT ( 'NONE',  ( -30.84268108620762305, 55.46651512039750997, -1.270000000000005125 ) ) ;
#39808 = CARTESIAN_POINT ( 'NONE',  ( -20.36908824613711033, 132.1502320877631007, 0.7851131432546855082 ) ) ;
#39809 = CARTESIAN_POINT ( 'NONE',  ( -2.830841276205400270, 0.8888151952923978305, 7.984752373722160179 ) ) ;
#39810 = CARTESIAN_POINT ( 'NONE',  ( 14.24959175664875843, 150.3563008155378213, 1.527850727897531513 ) ) ;
#39811 = DIRECTION ( 'NONE',  ( 5.188838149069472160E-16, -1.699382548006136559E-16, -1.000000000000000000 ) ) ;
#39812 = CARTESIAN_POINT ( 'NONE',  ( 0.008148259816486548221, 159.5682499516715040, -0.4077722408685185429 ) ) ;
#39813 = DIRECTION ( 'NONE',  ( -0.8745520943968243532, 0.4849315768086547296, -6.829619984160642269E-16 ) ) ;
#39814 = CARTESIAN_POINT ( 'NONE',  ( -57.34225532943530368, 1.923124478597425524, 1.535638195068367073 ) ) ;
#39815 = CARTESIAN_POINT ( 'NONE',  ( -47.93352606754567091, 24.19884373620804396, 0.9125764105762101952 ) ) ;
#39816 = CARTESIAN_POINT ( 'NONE',  ( -3.203180711741437481, 117.9394507697571584, 1.176600582426013952 ) ) ;
#39817 = CARTESIAN_POINT ( 'NONE',  ( -52.50198181065980663, 11.96455506022023307, 4.263607785004571937 ) ) ;
#39818 = CARTESIAN_POINT ( 'NONE',  ( -58.51012109478204337, -0.04195086158869835297, 0.6673390170621641415 ) ) ;
#39819 = CARTESIAN_POINT ( 'NONE',  ( -4.505903132795666011, 118.1291298611057243, 0.5121121603323477434 ) ) ;
#39820 = CARTESIAN_POINT ( 'NONE',  ( 3.946705940144926483, 109.6290786634770456, -3.598380483330867463 ) ) ;
#39821 = ORIENTED_EDGE ( 'NONE', *, *, #12927, .F. ) ;
#39822 = CARTESIAN_POINT ( 'NONE',  ( -46.67659519887701691, 22.71018310752411651, 3.598098858967599512 ) ) ;
#39823 = CARTESIAN_POINT ( 'NONE',  ( 8.335401033256285785, 120.0665470143100322, -1.117875946357163253 ) ) ;
#39824 = CARTESIAN_POINT ( 'NONE',  ( -6.508649675962092651, 120.6419738463991536, -0.3953840990482027085 ) ) ;
#39825 = CARTESIAN_POINT ( 'NONE',  ( 4.574997526833646688, 118.0705043500909142, 0.7556435857121347466 ) ) ;
#39826 = CARTESIAN_POINT ( 'NONE',  ( -7.104091076028453244, 121.8059686962219672, -0.6844636119373687100 ) ) ;
#39827 = CARTESIAN_POINT ( 'NONE',  ( -1.198294787039654974, 115.7029448745467732, -1.741961060379599413 ) ) ;
#39828 = CARTESIAN_POINT ( 'NONE',  ( 0.7552937574752076610, 117.3993842961046568, -1.459880452114538985 ) ) ;
#39829 = CYLINDRICAL_SURFACE ( 'NONE', #37632, 5.588000000000006295 ) ;
#39830 = CARTESIAN_POINT ( 'NONE',  ( -14.05412825714270397, 131.1061190467503934, -1.842221413061616797 ) ) ;
#39831 = CARTESIAN_POINT ( 'NONE',  ( 14.79536922792820697, 61.64024183321802042, 1.904999999999990257 ) ) ;
#39832 = CARTESIAN_POINT ( 'NONE',  ( -43.11180532273385779, 21.58876176642518629, 2.074236749937639068 ) ) ;
#39833 = CARTESIAN_POINT ( 'NONE',  ( 8.644792878686919479, 118.5213301182956656, -0.7512959218659588378 ) ) ;
#39834 = CARTESIAN_POINT ( 'NONE',  ( -3.792622695653071307, 121.0920089199514535, 0.02902016224539996636 ) ) ;
#39835 = DIRECTION ( 'NONE',  ( 0.4849315768086534528, 0.8745520943968250194, 1.030032898892974942E-16 ) ) ;
#39836 = CARTESIAN_POINT ( 'NONE',  ( 18.24338043389141362, 154.1370782493726210, 1.275500441016771624 ) ) ;
#39837 = CARTESIAN_POINT ( 'NONE',  ( -6.439703808512989190E-14, 63.33946620154573282, 4.463794035948134848E-29 ) ) ;
#39838 = CARTESIAN_POINT ( 'NONE',  ( 2.245555723253176872, -15.32365336378345511, 5.046800657416122604 ) ) ;
#39839 = CARTESIAN_POINT ( 'NONE',  ( -18.65843730539394230, 148.7425187291823363, 1.723213218779726441 ) ) ;
#39840 = CARTESIAN_POINT ( 'NONE',  ( -0.3451692354163579113, -3.745485276186693469, -0.9107729336563508138 ) ) ;
#39841 = CARTESIAN_POINT ( 'NONE',  ( -19.93082032328737085, 128.8226523212408949, -1.025501306202716734 ) ) ;
#39842 = CARTESIAN_POINT ( 'NONE',  ( 0.7509867122348852231, -11.68634165275979342, 0.6197512838553165260 ) ) ;
#39843 = ORIENTED_EDGE ( 'NONE', *, *, #18498, .F. ) ;
#39844 = ADVANCED_FACE ( 'NONE', ( #23981 ), #25556, .F. ) ;
#39845 = CARTESIAN_POINT ( 'NONE',  ( -42.12253153191132782, 21.94389511927449732, 0.09363185731630196962 ) ) ;
#39846 = CARTESIAN_POINT ( 'NONE',  ( 6.465481721428002260, 120.6581566633936404, 0.3941859656685693380 ) ) ;
#39847 = AXIS2_PLACEMENT_3D ( 'NONE', #11724, #31529, #24712 ) ;
#39848 = CARTESIAN_POINT ( 'NONE',  ( -9.374368624788303350, 123.5785764018267514, 0.4819391486299057226 ) ) ;
#39849 = CARTESIAN_POINT ( 'NONE',  ( 5.004296470405577679, -11.88282826624689825, 0.9770688040177184508 ) ) ;
#39850 = CARTESIAN_POINT ( 'NONE',  ( 17.49548072478902583, 148.2779598588913643, -1.530134328283176304 ) ) ;
#39851 = CARTESIAN_POINT ( 'NONE',  ( -9.864431837517996016, 120.7895603300898699, -1.595968683908903785 ) ) ;
#39852 = CARTESIAN_POINT ( 'NONE',  ( -2.864695162152176788, 104.6144662015457669, 3.894373788578088469 ) ) ;
#39853 = CARTESIAN_POINT ( 'NONE',  ( 2.467608985616319472, -14.95545905184315849, 4.893820528943690462 ) ) ;
#39854 = CARTESIAN_POINT ( 'NONE',  ( -4.915268796012386865, 117.6231067272046289, -0.9482029235052464866 ) ) ;
#39855 = CARTESIAN_POINT ( 'NONE',  ( 15.25729751669398659, 143.4548391324710224, 0.07249109134377358654 ) ) ;
#39856 = ORIENTED_EDGE ( 'NONE', *, *, #39433, .F. ) ;
#39857 = CARTESIAN_POINT ( 'NONE',  ( -2.790041887114321995, 107.7052943677556556, 4.425947592945074227 ) ) ;
#39858 = CARTESIAN_POINT ( 'NONE',  ( 4.439281039736937551, 110.9173483060885843, 3.020962623249374257 ) ) ;
#39859 = DIRECTION ( 'NONE',  ( 1.000000000000000000, 0.000000000000000000, 0.000000000000000000 ) ) ;
#39860 = CARTESIAN_POINT ( 'NONE',  ( -4.973569738608247803, 117.3993868453981548, -0.9750659555622913643 ) ) ;
#39861 = CARTESIAN_POINT ( 'NONE',  ( 15.16801640535318363, 156.1230782244120121, 0.1031879763837426633 ) ) ;
#39862 = DIRECTION ( 'NONE',  ( -5.206863593109713661E-17, 1.000000000000000000, -1.077750396879097183E-30 ) ) ;
#39863 = CARTESIAN_POINT ( 'NONE',  ( 1.989873938678733412, -15.24182034147698950, 5.977043307750504297 ) ) ;
#39864 = CARTESIAN_POINT ( 'NONE',  ( 11.55299880265466506, 55.57741982016700177, 4.472382752598254463 ) ) ;
#39865 = CARTESIAN_POINT ( 'NONE',  ( -2.603905383243863891, 31.86823266994409565, 1.021610582188352323 ) ) ;
#39866 = CARTESIAN_POINT ( 'NONE',  ( 14.76979702826404406, 154.6636077862465015, 2.174438252133946481 ) ) ;
#39867 = AXIS2_PLACEMENT_3D ( 'NONE', #40869, #31056, #28284 ) ;
#39868 = VERTEX_POINT ( 'NONE', #40205 ) ;
#39869 = CARTESIAN_POINT ( 'NONE',  ( -0.4304388160753707671, 14.75877898171113145, 8.412599170943037663 ) ) ;
#39870 = CARTESIAN_POINT ( 'NONE',  ( -8.600679198160465333, 118.5556138246751487, -1.111917903331490987 ) ) ;
#39871 = CARTESIAN_POINT ( 'NONE',  ( -2.327304502367640193, 119.2037781873646622, -0.6856724729282701603 ) ) ;
#39872 = CARTESIAN_POINT ( 'NONE',  ( -5.496588887047691330, 78.91991874857598077, 5.121802412194515597 ) ) ;
#39873 = CARTESIAN_POINT ( 'NONE',  ( -10.62867326514809108, 56.48194529650092477, -4.405924061720180696 ) ) ;
#39874 = CARTESIAN_POINT ( 'NONE',  ( -4.356736194631761094, 104.6144662015456959, 2.084086694369730264 ) ) ;
#39875 = CARTESIAN_POINT ( 'NONE',  ( 4.634220987317881679, -1.855718946426311078, -0.01876340930339078644 ) ) ;
#39876 = CARTESIAN_POINT ( 'NONE',  ( -17.14500000000466784, 71.11999999999886768, 1.523999999999998689 ) ) ;
#39877 = CARTESIAN_POINT ( 'NONE',  ( -4.851810479404537801, 115.6909491485453003, 1.282009238014815811 ) ) ;
#39878 = CARTESIAN_POINT ( 'NONE',  ( 2.905753382753808900, -13.11311505661566557, 0.7091545436608904796 ) ) ;
#39879 = CARTESIAN_POINT ( 'NONE',  ( 3.467804978690671280, 119.7720183225874138, -0.4097519885510783610 ) ) ;
#39880 = CARTESIAN_POINT ( 'NONE',  ( -0.3479910049261774052, 116.9201722098172382, 0.3032510685202792766 ) ) ;
#39881 = EDGE_CURVE ( 'NONE', #40718, #13050, #7882, .T. ) ;
#39882 = LINE ( 'NONE', #32850, #34650 ) ;
#39883 = DIRECTION ( 'NONE',  ( -0.4849315768086534528, -0.8745520943968249084, -1.030032898892974818E-16 ) ) ;
#39884 = EDGE_LOOP ( 'NONE', ( #10906, #6444 ) ) ;
#39885 = CARTESIAN_POINT ( 'NONE',  ( -13.17422243436020857, 17.14499999999999957, -5.016499999999999737 ) ) ;
#39886 = CARTESIAN_POINT ( 'NONE',  ( 4.883858777703569132, -15.45279978240890451, 0.9440085714135780792 ) ) ;
#39887 = CARTESIAN_POINT ( 'NONE',  ( -19.90609901365559509, 149.5711785761137662, 1.665592367946398644 ) ) ;
#39888 = CARTESIAN_POINT ( 'NONE',  ( -3.416230376366909294, -5.529048218071860532, 3.121479803864907865 ) ) ;
#39889 = EDGE_CURVE ( 'NONE', #17866, #23676, #33050, .T. ) ;
#39890 = ORIENTED_EDGE ( 'NONE', *, *, #32998, .T. ) ;
#39891 = CARTESIAN_POINT ( 'NONE',  ( -58.36992421181234647, -0.2917964073288620286, 4.861495987418534161E-13 ) ) ;
#39892 = CARTESIAN_POINT ( 'NONE',  ( 2.311675797007677335, 124.5312663981120380, 0.07107509915817157575 ) ) ;
#39893 = B_SPLINE_SURFACE_WITH_KNOTS ( 'NONE', 3, 3, ( 
 ( #22708, #35523, #6761, #3362, #9324, #2943, #12722, #16112 ),
 ( #12517, #35109, #22287, #3149, #19523, #19104, #12309, #35949 ),
 ( #19729, #9120, #19315, #9945, #31904, #6549, #18895, #2533 ),
 ( #41503, #35737, #35312, #38718, #2740, #6345, #16329, #15907 ) ),
 .UNSPECIFIED., .F., .F., .F.,
 ( 4, 4 ),
 ( 4, 2, 2, 4 ),
 ( 0.000000000000000000, 1.000000000000000000 ),
 ( 0.000000000000000000, 0.2500000000000000000, 0.5000000000000000000, 1.000000000000000000 ),
 .UNSPECIFIED. ) ;
#39894 = CARTESIAN_POINT ( 'NONE',  ( -11.17088054096573124, 124.6236798342360856, 0.9649352710901087926 ) ) ;
#39895 = CARTESIAN_POINT ( 'NONE',  ( 1.526750911922509779, 118.1287369781418164, 0.9395972400893385368 ) ) ;
#39896 = CARTESIAN_POINT ( 'NONE',  ( 18.43358770356677923, 147.0160646422468744, -1.663356549802410767 ) ) ;
#39897 = CARTESIAN_POINT ( 'NONE',  ( -16.23079787743092339, 153.4734386769207504, -2.282812701028141600 ) ) ;
#39898 = CARTESIAN_POINT ( 'NONE',  ( -24.10666987309389597, 82.16896248603319464, 1.523999999999993138 ) ) ;
#39899 = ORIENTED_EDGE ( 'NONE', *, *, #34392, .T. ) ;
#39900 = CIRCLE ( 'NONE', #30354, 3.175000000000001155 ) ;
#39901 = CARTESIAN_POINT ( 'NONE',  ( 4.164354687101496921, 118.2394403266935115, -0.2263719665096066147 ) ) ;
#39902 = EDGE_CURVE ( 'NONE', #29093, #25690, #31673, .T. ) ;
#39903 = CARTESIAN_POINT ( 'NONE',  ( 6.164480127824531586, 155.3548635187015350, -0.4492659787150437012 ) ) ;
#39904 = VECTOR ( 'NONE', #35172, 999.9999999999998863 ) ;
#39905 = EDGE_LOOP ( 'NONE', ( #25473, #660, #11623, #9274 ) ) ;
#39906 = VECTOR ( 'NONE', #20235, 1000.000000000000000 ) ;
#39907 = CARTESIAN_POINT ( 'NONE',  ( 2.484037338616324142, -15.29988040857715959, 4.804498879097399033 ) ) ;
#39908 = CARTESIAN_POINT ( 'NONE',  ( -4.932064943850939187, 117.4109299206517818, 0.9378731322835484052 ) ) ;
#39909 = CARTESIAN_POINT ( 'NONE',  ( -58.36582417652992660, -0.2832568706214733112, 0.07935633695520924458 ) ) ;
#39910 = CARTESIAN_POINT ( 'NONE',  ( -4.503669762702418033, -0.7216326387320324276, 1.072590735790061922 ) ) ;
#39912 = EDGE_CURVE ( 'NONE', #27998, #42038, #14717, .T. ) ;
#39911 = CARTESIAN_POINT ( 'NONE',  ( 3.477534164838054664, 156.5024071230465097, 1.413294873543960550 ) ) ;
#39913 = CARTESIAN_POINT ( 'NONE',  ( 2.920597266354742150, 38.61197011361286258, -0.9696037573092457507 ) ) ;
#39914 = CARTESIAN_POINT ( 'NONE',  ( 4.627880361116947228, 7.839802885307131319, -0.3238752845059330032 ) ) ;
#39915 = CARTESIAN_POINT ( 'NONE',  ( 12.88021573494086525, 133.7932622986943159, 0.3045934876098303490 ) ) ;
#39916 = FACE_OUTER_BOUND ( 'NONE', #9059, .T. ) ;
#39917 = ADVANCED_FACE ( 'NONE', ( #39996 ), #804, .T. ) ;
#39918 = CARTESIAN_POINT ( 'NONE',  ( -52.48304539424793091, 11.63526101311008354, -3.802211793135442885 ) ) ;
#39919 = CARTESIAN_POINT ( 'NONE',  ( 2.177580517772025104, 116.2510284916901782, -0.1164253007932135875 ) ) ;
#39920 = DIRECTION ( 'NONE',  ( -0.01997839162482737546, -1.040247600000940825E-18, 0.9998004120163610509 ) ) ;
#39921 = FACE_OUTER_BOUND ( 'NONE', #26558, .T. ) ;
#39922 = CARTESIAN_POINT ( 'NONE',  ( -14.60500000000000220, 71.11999999999999034, -5.080000000000000959 ) ) ;
#39923 = LINE ( 'NONE', #7127, #33153 ) ;
#39924 = CARTESIAN_POINT ( 'NONE',  ( -1.495267265506447174, 0.7142801726123456652, -8.304712878169773660 ) ) ;
#39925 = EDGE_CURVE ( 'NONE', #926, #25156, #23656, .T. ) ;
#39926 = DIRECTION ( 'NONE',  ( 5.206863593109713661E-17, -1.000000000000000000, 1.077750396879097183E-30 ) ) ;
#39927 = DIRECTION ( 'NONE',  ( -1.000000000000000000, 0.000000000000000000, 0.000000000000000000 ) ) ;
#39928 = CARTESIAN_POINT ( 'NONE',  ( -58.43523997267251247, 0.9435442997105664142, 0.5849561510202019310 ) ) ;
#39929 = CARTESIAN_POINT ( 'NONE',  ( 0.01254005783130787005, 120.1716774721351157, -0.6275557724548823657 ) ) ;
#39930 = CARTESIAN_POINT ( 'NONE',  ( -15.22618061423900215, 120.7148350616293300, 0.1140551857323335305 ) ) ;
#39931 = AXIS2_PLACEMENT_3D ( 'NONE', #22901, #35937, #32954 ) ;
#39932 = EDGE_LOOP ( 'NONE', ( #32005, #32149, #5789, #21306 ) ) ;
#39933 = CARTESIAN_POINT ( 'NONE',  ( -56.91937565786325592, 5.591339438888994984, -0.1632292574589517820 ) ) ;
#39934 = CARTESIAN_POINT ( 'NONE',  ( 7.795083226883911642, 122.5915480376389866, 0.009939133504787384804 ) ) ;
#39935 = ORIENTED_EDGE ( 'NONE', *, *, #25682, .T. ) ;
#39936 = DIRECTION ( 'NONE',  ( 0.8745520943968249084, -0.4849315768086533418, 5.271987356194193006E-16 ) ) ;
#39937 = CARTESIAN_POINT ( 'NONE',  ( -15.21722582537775637, 143.4245298570049840, -0.3558394363636828706 ) ) ;
#39938 = CARTESIAN_POINT ( 'NONE',  ( 5.379018416755689813, -14.82644845813459256, 3.481186560222681692 ) ) ;
#39939 = CARTESIAN_POINT ( 'NONE',  ( -20.76034172958460644, 149.5879773183856685, 1.515053003442401680 ) ) ;
#39940 = CARTESIAN_POINT ( 'NONE',  ( -4.420329592304260480, 21.65838872207745425, -1.398650104627336743 ) ) ;
#39941 = CARTESIAN_POINT ( 'NONE',  ( 23.20196384716129856, 149.3105122542552863, 0.9177021184322482483 ) ) ;
#39942 = CARTESIAN_POINT ( 'NONE',  ( 2.217927584814327613, -15.58779998727646898, 5.527464523343218694 ) ) ;
#39943 = CARTESIAN_POINT ( 'NONE',  ( -1.648064503646425649, 29.87956589480163316, -4.325937074807028715 ) ) ;
#39944 = CARTESIAN_POINT ( 'NONE',  ( -0.2091969695887432312, -7.904008462454454431, -0.9542532860826526964 ) ) ;
#39945 = CARTESIAN_POINT ( 'NONE',  ( -14.74522353080556947, 120.3062992333385921, -0.5208356519839250076 ) ) ;
#39946 = CARTESIAN_POINT ( 'NONE',  ( 4.937178538763392410, 117.4076076791066470, 1.082348873812597922 ) ) ;
#39947 = ORIENTED_EDGE ( 'NONE', *, *, #23307, .F. ) ;
#39948 = CARTESIAN_POINT ( 'NONE',  ( -2.255705573375303974, 116.3134673151485430, 0.1365217663799836445 ) ) ;
#39949 = CARTESIAN_POINT ( 'NONE',  ( -14.94938132205808579, 131.2528086460777388, 1.477614431843955467 ) ) ;
#39950 = CARTESIAN_POINT ( 'NONE',  ( -57.92987961479896342, 0.6565893080917146740, -0.9491229006729858808 ) ) ;
#39951 = CARTESIAN_POINT ( 'NONE',  ( 3.077448401760547902, 117.9340107969418341, 0.8067720256249978350 ) ) ;
#39952 = CARTESIAN_POINT ( 'NONE',  ( 18.20160870511324447, 135.6759721228443425, -1.705493676697015015 ) ) ;
#39953 = CARTESIAN_POINT ( 'NONE',  ( 0.4551624184790937777, -5.041848893434334400, -0.8611515851349844652 ) ) ;
#39954 = CARTESIAN_POINT ( 'NONE',  ( -21.34910226488280927, 149.1985357531029308, -2.237902092811237864 ) ) ;
#39955 = VECTOR ( 'NONE', #8345, 1000.000000000000000 ) ;
#39956 = CARTESIAN_POINT ( 'NONE',  ( -41.45218294293373162, 22.69057396248467384, -1.547390787314429472 ) ) ;
#39957 = AXIS2_PLACEMENT_3D ( 'NONE', #28236, #41242, #12047 ) ;
#39958 = CARTESIAN_POINT ( 'NONE',  ( 3.853324095080354006, 105.1225530707694986, 3.704948206273974698 ) ) ;
#39959 = CARTESIAN_POINT ( 'NONE',  ( 4.430366727502268454, 120.6578283891288379, -0.4452475156743748164 ) ) ;
#39960 = CARTESIAN_POINT ( 'NONE',  ( -1.561582345843753217, 156.2588034088681184, -0.03120413162939504950 ) ) ;
#39961 = VERTEX_POINT ( 'NONE', #7609 ) ;
#39962 = CARTESIAN_POINT ( 'NONE',  ( -14.47078677760135257, 128.5519869857110393, -2.060874889273090815 ) ) ;
#39963 = CARTESIAN_POINT ( 'NONE',  ( 2.005403748902764516, -15.69871118693741430, 5.609036204238825540 ) ) ;
#39964 = CIRCLE ( 'NONE', #20884, 3.175000000000001155 ) ;
#39965 = DIRECTION ( 'NONE',  ( -0.8745520943968235761, 0.4849315768086558953, -5.361993529360570985E-16 ) ) ;
#39966 = CARTESIAN_POINT ( 'NONE',  ( -4.543664835419952475, 118.0881836969183070, -0.7497823245519673607 ) ) ;
#39967 = CARTESIAN_POINT ( 'NONE',  ( -50.15972161391664486, 17.13814111569220699, -4.955022299345085202 ) ) ;
#39968 = EDGE_CURVE ( 'NONE', #12580, #8945, #8568, .T. ) ;
#39969 = AXIS2_PLACEMENT_3D ( 'NONE', #16207, #9006, #35003 ) ;
#39970 = CARTESIAN_POINT ( 'NONE',  ( 4.111708801323036511, 118.2429491485453354, 0.3463700888942771727 ) ) ;
#39971 = CARTESIAN_POINT ( 'NONE',  ( 15.87222905729431943, 135.0473088626721392, 2.190551936964585611 ) ) ;
#39972 = DIRECTION ( 'NONE',  ( -6.353134868986659519E-16, 1.000000000000000000, 0.000000000000000000 ) ) ;
#39973 = CARTESIAN_POINT ( 'NONE',  ( 3.707388773974296559, 116.6237204831772232, 0.06043239539139045463 ) ) ;
#39974 = CARTESIAN_POINT ( 'NONE',  ( -7.794209556482943668, 13.03656553185805222, 3.210957146378262461 ) ) ;
#39975 = CARTESIAN_POINT ( 'NONE',  ( 9.418980095613568082, 123.9587481073520223, 0.7032982658115918273 ) ) ;
#39976 = CARTESIAN_POINT ( 'NONE',  ( 16.18247977474483079, 122.8183540351560907, -0.6517309543831906193 ) ) ;
#39977 = EDGE_CURVE ( 'NONE', #40944, #1213, #13312, .T. ) ;
#39978 = CARTESIAN_POINT ( 'NONE',  ( 5.664977208693820820, 57.14999999999998437, 5.033228321271210781 ) ) ;
#39979 = CARTESIAN_POINT ( 'NONE',  ( 0.06584543127246964000, 115.6909491485452719, 1.765419582720901825 ) ) ;
#39980 = EDGE_CURVE ( 'NONE', #29654, #29150, #24174, .T. ) ;
#39981 = CARTESIAN_POINT ( 'NONE',  ( -14.87733005835129063, 120.3210621052586475, -0.2473824415510233188 ) ) ;
#39982 = ORIENTED_EDGE ( 'NONE', *, *, #7838, .F. ) ;
#39983 = CARTESIAN_POINT ( 'NONE',  ( -46.60530155212508419, 26.17382724835469432, -1.171222222222230824 ) ) ;
#39984 = CARTESIAN_POINT ( 'NONE',  ( 6.835380503559908227, 121.3218668833306992, -0.5961742291405608407 ) ) ;
#39985 = DIRECTION ( 'NONE',  ( -0.5149185422762221354, 0.8572391118119438991, -4.128606161907600514E-16 ) ) ;
#39986 = ORIENTED_EDGE ( 'NONE', *, *, #9443, .F. ) ;
#39987 = CARTESIAN_POINT ( 'NONE',  ( -1.598479218588914730, 156.2658572007470639, -0.3094434466263948913 ) ) ;
#39988 = CARTESIAN_POINT ( 'NONE',  ( 4.668376822648329316, -11.99306229768662391, 1.198378876927704839 ) ) ;
#39989 = CARTESIAN_POINT ( 'NONE',  ( -22.07843093565582038, 149.7938220333360846, 0.9986438184040021815 ) ) ;
#39990 = FACE_OUTER_BOUND ( 'NONE', #15711, .T. ) ;
#39991 = CARTESIAN_POINT ( 'NONE',  ( 1.804784692667541268, 116.4728921782852922, 0.07541441754812436282 ) ) ;
#39992 = B_SPLINE_CURVE_WITH_KNOTS ( 'NONE', 3,
 ( #22753, #19569, #3409, #16377, #29382, #222, #36628, #40042 ),
 .UNSPECIFIED., .F., .F.,
 ( 4, 2, 2, 4 ),
 ( 0.003986743484052247127, 0.004242962777773731133, 0.004499182071495215138, 0.005011620658938190087 ),
 .UNSPECIFIED. ) ;
#39993 = ORIENTED_EDGE ( 'NONE', *, *, #20134, .T. ) ;
#39994 = CARTESIAN_POINT ( 'NONE',  ( 2.294499597581835193, -9.852027417895397932, -4.012603411698490774 ) ) ;
#39995 = CARTESIAN_POINT ( 'NONE',  ( -5.757472737270721730, 159.1136035536173097, -0.1150480073142621795 ) ) ;
#39996 = FACE_OUTER_BOUND ( 'NONE', #26685, .T. ) ;
#39997 = CARTESIAN_POINT ( 'NONE',  ( -24.10666987309389597, 82.16896248603319464, 1.269999999999993134 ) ) ;
#39998 = AXIS2_PLACEMENT_3D ( 'NONE', #17284, #33491, #10474 ) ;
#39999 = ORIENTED_EDGE ( 'NONE', *, *, #30481, .F. ) ;
#40000 = CARTESIAN_POINT ( 'NONE',  ( 4.914704081444464023, 119.0942267931248040, 1.098002887962306495 ) ) ;
#40001 = CARTESIAN_POINT ( 'NONE',  ( 3.573240411403531436, -4.819783300376494495, -2.961220487682875824 ) ) ;
#40002 = CARTESIAN_POINT ( 'NONE',  ( 2.005144469770952398, 117.2046888992736200, 0.5340627965622031237 ) ) ;
#40003 = CARTESIAN_POINT ( 'NONE',  ( -58.67120857663339706, -0.3138064510428972831, -0.3172299661764663159 ) ) ;
#40005 = CARTESIAN_POINT ( 'NONE',  ( 9.293546136053006279, 157.2521837264336853, -1.575842917768122575 ) ) ;
#40004 = CARTESIAN_POINT ( 'NONE',  ( 5.860279866549846339, 57.15000000000084412, 5.019549989156823600 ) ) ;
#40006 = CARTESIAN_POINT ( 'NONE',  ( -4.120466288800530563, -1.808681497221679590, -2.133573495687988597 ) ) ;
#40007 = CARTESIAN_POINT ( 'NONE',  ( -2.946415863239081556, 117.2422168882539211, -0.6071713939981749908 ) ) ;
#40008 = VERTEX_POINT ( 'NONE', #3795 ) ;
#40009 = CARTESIAN_POINT ( 'NONE',  ( -9.679874449561454597, 124.8500477395539576, -0.02572261534930060309 ) ) ;
#40010 = CARTESIAN_POINT ( 'NONE',  ( 5.122375111755775201, -14.64399685039916044, 3.991980633533394052 ) ) ;
#40011 =( BOUNDED_CURVE ( )  B_SPLINE_CURVE ( 3, ( #12948, #3601, #410, #12745 ),
 .UNSPECIFIED., .F., .T. ) 
 B_SPLINE_CURVE_WITH_KNOTS ( ( 4, 4 ),
 ( 1.570796326794896558, 3.141592653589793116 ),
 .UNSPECIFIED. ) 
 CURVE ( )  GEOMETRIC_REPRESENTATION_ITEM ( )  RATIONAL_B_SPLINE_CURVE ( ( 1.000000000000000000, 0.8047378541243649375, 0.8047378541243649375, 1.000000000000000000 ) ) 
 REPRESENTATION_ITEM ( '' )  );
#40012 = CARTESIAN_POINT ( 'NONE',  ( -43.93237127071131454, 21.31409657049223227, 2.696834577194972216 ) ) ;
#40013 = TOROIDAL_SURFACE ( 'NONE', #27044, 5.080000000000005400, 0.5080000000000000071 ) ;
#40014 = CARTESIAN_POINT ( 'NONE',  ( -0.07510606132778108179, 117.9496054766374158, -1.407797200287234984 ) ) ;
#40015 = VERTEX_POINT ( 'NONE', #10581 ) ;
#40016 = CARTESIAN_POINT ( 'NONE',  ( 2.337245495867128486, 157.7073581658784178, 1.721377379916721129 ) ) ;
#40017 = CARTESIAN_POINT ( 'NONE',  ( -7.461250000000054783, 86.35999999999998522, 9.137395930138188390E-16 ) ) ;
#40018 = CARTESIAN_POINT ( 'NONE',  ( -0.3623072504456354981, 117.0882377308211773, 0.3576919811193871035 ) ) ;
#40019 = CARTESIAN_POINT ( 'NONE',  ( 7.688107727944508696, 4.450669244509953160, -3.435853896805545649 ) ) ;
#40020 = CARTESIAN_POINT ( 'NONE',  ( 8.359771539777417715, 154.6912814427390970, 1.273680951853117138 ) ) ;
#40021 = DIRECTION ( 'NONE',  ( -0.9998004120163609398, 0.000000000000000000, -0.01997839162482749689 ) ) ;
#40022 = CARTESIAN_POINT ( 'NONE',  ( 15.62635203013925889, 121.2802728028965475, -0.2997488694636321060 ) ) ;
#40023 = CARTESIAN_POINT ( 'NONE',  ( -15.50061618130081165, 62.14374591690594940, -1.904999999999999583 ) ) ;
#40024 = CARTESIAN_POINT ( 'NONE',  ( -57.62836615807631802, 1.308031921563323596, 1.276376674128435029 ) ) ;
#40025 = CARTESIAN_POINT ( 'NONE',  ( -50.22242355904485578, 22.76272800790864181, 0.3424289802766369295 ) ) ;
#40026 = EDGE_CURVE ( 'NONE', #9964, #33280, #38915, .T. ) ;
#40027 = CARTESIAN_POINT ( 'NONE',  ( -51.02479983779974049, 14.46739584830851477, 4.600955224801048793 ) ) ;
#40028 = CARTESIAN_POINT ( 'NONE',  ( -58.64020961342745153, -0.3060494297185549217, 0.3493912677027103397 ) ) ;
#40029 = CARTESIAN_POINT ( 'NONE',  ( -4.385328315531485721, 118.1846248134211379, 0.4263140361897638231 ) ) ;
#40030 = CARTESIAN_POINT ( 'NONE',  ( -30.15519950990045572, 69.97033940222175374, -1.270000000000007123 ) ) ;
#40031 = ORIENTED_EDGE ( 'NONE', *, *, #7974, .T. ) ;
#40032 = CARTESIAN_POINT ( 'NONE',  ( -44.96292901393739783, 21.56701576681934540, 3.486870777078499017 ) ) ;
#40033 = CARTESIAN_POINT ( 'NONE',  ( 6.170393643008810436, 119.5853013911638811, -1.006946838071717032 ) ) ;
#40034 = CARTESIAN_POINT ( 'NONE',  ( -3.916844122728852184, 109.8065891650451249, -3.681372831196203066 ) ) ;
#40035 = CARTESIAN_POINT ( 'NONE',  ( 4.491247496296435493, 118.1274053408948390, 0.6814523630037505608 ) ) ;
#40036 = CARTESIAN_POINT ( 'NONE',  ( -15.61785206596079689, 148.1291547725267037, -1.273309296088947828 ) ) ;
#40037 =( GEOMETRIC_REPRESENTATION_CONTEXT ( 3 ) GLOBAL_UNCERTAINTY_ASSIGNED_CONTEXT ( ( #16317 ) ) GLOBAL_UNIT_ASSIGNED_CONTEXT ( ( #37942, #5793, #38372 ) ) REPRESENTATION_CONTEXT ( 'NONE', 'WORKASPACE' ) );
#40038 = CARTESIAN_POINT ( 'NONE',  ( -0.8519111957592009343, 115.7029491485453576, -1.752612029837606666 ) ) ;
#40039 = CARTESIAN_POINT ( 'NONE',  ( 5.348924234570989533, 56.51499999999999346, -4.492130288940734850 ) ) ;
#40040 = FACE_OUTER_BOUND ( 'NONE', #5090, .T. ) ;
#40041 = CARTESIAN_POINT ( 'NONE',  ( -8.650892266477143266, 122.3401343867201945, -1.081441824013609443 ) ) ;
#40042 = CARTESIAN_POINT ( 'NONE',  ( -13.17422243436020857, 17.14499999999999957, -5.016499999999999737 ) ) ;
#40043 = CARTESIAN_POINT ( 'NONE',  ( -46.93088534759985464, 20.29541677029552460, 5.030633991647738945 ) ) ;
#40044 = CARTESIAN_POINT ( 'NONE',  ( 7.931359276468123554, 121.9896588117074998, -0.6306316981394162191 ) ) ;
#40045 = CARTESIAN_POINT ( 'NONE',  ( -0.001427691597722236970, 156.3034662015458593, 0.07144752562581345445 ) ) ;
#40046 = CARTESIAN_POINT ( 'NONE',  ( -6.550797450135577910E-14, 84.67546620154573134, 2.164564701558966795E-29 ) ) ;
#40047 = CARTESIAN_POINT ( 'NONE',  ( 5.829268545577174443, 117.2350771734024164, 0.5950018394081721951 ) ) ;
#40048 = CARTESIAN_POINT ( 'NONE',  ( 5.965356522962838248, 77.01756249999996840, -5.016499999999999737 ) ) ;
#40049 = CARTESIAN_POINT ( 'NONE',  ( 3.065366080762625955, -14.95244456720379311, 3.762810261076596330 ) ) ;
#40050 = CARTESIAN_POINT ( 'NONE',  ( -18.50543525367162090, 148.3462492009778373, 1.698196615343024796 ) ) ;
#40051 = CARTESIAN_POINT ( 'NONE',  ( -0.5824522774871869757, -3.319493544524417583, -0.7801697309090062094 ) ) ;
#40052 = CARTESIAN_POINT ( 'NONE',  ( -5.580240031299428694, 159.0849926622337023, -0.6989143883095924048 ) ) ;
#40053 = CARTESIAN_POINT ( 'NONE',  ( -0.7070771686734943495, -4.675651901196332005, 0.6724949525944122763 ) ) ;
#40054 = ORIENTED_EDGE ( 'NONE', *, *, #302, .T. ) ;
#40055 = CARTESIAN_POINT ( 'NONE',  ( -48.74330358230356808, 18.21177412086844072, 5.147861347727184622 ) ) ;
#40056 = CARTESIAN_POINT ( 'NONE',  ( 5.908534618823872542, 118.9825038774357466, 0.5858829404670616858 ) ) ;
#40057 = CARTESIAN_POINT ( 'NONE',  ( -4.443995521150195138, 155.8637389808261275, 0.5396741685193008342 ) ) ;
#40058 = CARTESIAN_POINT ( 'NONE',  ( 2.417269819423324861, -15.13903239461346395, 5.861448462117607505 ) ) ;
#40059 = CARTESIAN_POINT ( 'NONE',  ( 16.84814155439267935, 148.3581316477378493, -1.364645798843572733 ) ) ;
#40060 = ORIENTED_EDGE ( 'NONE', *, *, #1932, .T. ) ;
#40061 = CARTESIAN_POINT ( 'NONE',  ( -15.19444909298876567, 153.0676604005411434, -2.356382943223728876 ) ) ;
#40062 = CIRCLE ( 'NONE', #21640, 0.5080000000000000071 ) ;
#40063 = CARTESIAN_POINT ( 'NONE',  ( -1.157812389576497347, 104.6144662015457669, 4.694735647536337098 ) ) ;
#40064 = CARTESIAN_POINT ( 'NONE',  ( 3.075357915497110017, -13.94103813162880989, 1.416127232796946966 ) ) ;
#40065 = CARTESIAN_POINT ( 'NONE',  ( -4.944211420742701257, 117.5327897045929859, -0.9782740106667096036 ) ) ;
#40066 = CARTESIAN_POINT ( 'NONE',  ( 13.61628268276109210, 150.2179846313823930, 0.04905232040057783127 ) ) ;
#40067 = ORIENTED_EDGE ( 'NONE', *, *, #2160, .F. ) ;
#40068 = CARTESIAN_POINT ( 'NONE',  ( -2.561166057192335366, 106.9230564690795546, 4.673879012131969546 ) ) ;
#40069 = CARTESIAN_POINT ( 'NONE',  ( 4.679650109289619664, 111.8766742161798220, 2.628376281732180075 ) ) ;
#40070 = PRODUCT_DEFINITION_FORMATION_WITH_SPECIFIED_SOURCE ( 'ANY', '', #1125, .NOT_KNOWN. ) ;
#40071 = FACE_OUTER_BOUND ( 'NONE', #5766, .T. ) ;
#40072 = CARTESIAN_POINT ( 'NONE',  ( 18.71881220850874072, 125.2636347375217838, 0.1974931939226153843 ) ) ;
#40073 = CIRCLE ( 'NONE', #30505, 0.5080000000000002292 ) ;
#40074 = FACE_BOUND ( 'NONE', #8055, .T. ) ;
#40075 = CARTESIAN_POINT ( 'NONE',  ( 2.064435910936676777, -15.27355197655908015, 5.962396817882995137 ) ) ;
#40076 = FACE_OUTER_BOUND ( 'NONE', #21146, .T. ) ;
#40077 = CARTESIAN_POINT ( 'NONE',  ( -4.845170713328630363, 117.7576911979032559, -0.9526118176995749254 ) ) ;
#40078 = CARTESIAN_POINT ( 'NONE',  ( 14.40940766795059069, 123.3930721568691382, 1.837956572252896104 ) ) ;
#40079 = ORIENTED_EDGE ( 'NONE', *, *, #28197, .F. ) ;
#40080 = CARTESIAN_POINT ( 'NONE',  ( -7.524129562762011503, 22.75916136179084859, 3.848622047589015160 ) ) ;
#40081 = CARTESIAN_POINT ( 'NONE',  ( -8.593394099080960302, 118.5896537841807969, -1.127171445019202300 ) ) ;
#40082 = CARTESIAN_POINT ( 'NONE',  ( -3.662133038521701245, 120.6652674781340551, -0.4257566204602384330 ) ) ;
#40083 = CARTESIAN_POINT ( 'NONE',  ( -5.385891243464945966, 78.92849802251097913, 5.190125708699868667 ) ) ;
#40084 = CARTESIAN_POINT ( 'NONE',  ( -0.4201689423133995183, 106.0154168944984434, -5.283495245356437664 ) ) ;
#40085 = CARTESIAN_POINT ( 'NONE',  ( -0.007670926888326720997, 121.5961256765098284, 0.3838845493045228707 ) ) ;
#40086 = CARTESIAN_POINT ( 'NONE',  ( 0.3994026957563919789, 5.465888722076803319, 4.619092260001838923 ) ) ;
#40087 = DIRECTION ( 'NONE',  ( -0.8745520943968250194, 0.4849315768086535083, -5.424246918827963022E-16 ) ) ;
#40088 = CARTESIAN_POINT ( 'NONE',  ( -4.789447579930971699, 118.5264896598256854, 0.8320597001846437024 ) ) ;
#40089 = CARTESIAN_POINT ( 'NONE',  ( 2.946624452826990925, -14.63926610985447141, 4.195571020465345136 ) ) ;
#40090 = CARTESIAN_POINT ( 'NONE',  ( 5.854942301702412699, 124.9344662015456890, 0.1169956811762815629 ) ) ;
#40091 = CARTESIAN_POINT ( 'NONE',  ( -5.566083668711205412, 159.0643023895801491, 0.5661052595122398889 ) ) ;
#40092 = CARTESIAN_POINT ( 'NONE',  ( -4.171639465256384405, 28.89343014676064669, 2.695540212632123289 ) ) ;
#40093 = DIRECTION ( 'NONE',  ( -5.188838149069472160E-16, 1.699382548006136559E-16, 1.000000000000000000 ) ) ;
#40094 = ORIENTED_EDGE ( 'NONE', *, *, #1682, .F. ) ;
#40095 = CARTESIAN_POINT ( 'NONE',  ( -5.282613984594703105, 105.1224582691644258, -0.7587507295933431095 ) ) ;
#40096 = CARTESIAN_POINT ( 'NONE',  ( 4.512673509771836677, -15.64532105467335299, 2.834742450761120303 ) ) ;
#40097 = CARTESIAN_POINT ( 'NONE',  ( -3.234792161733187843, 118.6508749770327995, 0.7732002099368725512 ) ) ;
#40098 = CARTESIAN_POINT ( 'NONE',  ( -0.7219274401084647685, 31.37879824840181442, -0.6700674276139703123 ) ) ;
#40099 = ORIENTED_EDGE ( 'NONE', *, *, #41610, .F. ) ;
#40100 = DIRECTION ( 'NONE',  ( -0.9998501190848633202, -0.01731298258488772612, -5.158639060800499282E-16 ) ) ;
#40101 = CARTESIAN_POINT ( 'NONE',  ( 0.5374927741465299613, 112.6282971158091470, 2.756357034314327770 ) ) ;
#40102 =( LENGTH_UNIT ( ) NAMED_UNIT ( * ) SI_UNIT ( .MILLI., .METRE. ) );
#40103 = CARTESIAN_POINT ( 'NONE',  ( -17.00728043862078565, 146.2370505443881257, 1.250989154318494556 ) ) ;
#40104 = CARTESIAN_POINT ( 'NONE',  ( -46.95911617132934879, 24.98948415085533270, 1.986615011824473864 ) ) ;
#40105 = AXIS2_PLACEMENT_3D ( 'NONE', #39454, #10256, #18839 ) ;
#40106 = CARTESIAN_POINT ( 'NONE',  ( 4.259301615573734878, 119.5670751559891585, -0.7808790134437380015 ) ) ;
#40107 = AXIS2_PLACEMENT_3D ( 'NONE', #24084, #13875, #33272 ) ;
#40108 = CARTESIAN_POINT ( 'NONE',  ( -8.976454200711149412, 119.5326672034033777, -1.412516637748555404 ) ) ;
#40109 = LINE ( 'NONE', #4540, #23365 ) ;
#40110 = EDGE_LOOP ( 'NONE', ( #28966, #36810, #4889, #13971 ) ) ;
#40111 = CARTESIAN_POINT ( 'NONE',  ( 4.163732346407177154, 118.2394253532318373, -0.2271039051975612677 ) ) ;
#40112 = CARTESIAN_POINT ( 'NONE',  ( 0.6220149250934452478, 120.7813932625355307, -0.1825499261673580731 ) ) ;
#40113 = B_SPLINE_CURVE_WITH_KNOTS ( 'NONE', 3,
 ( #4599, #11958, #17353, #30342, #39753, #40375, #28145, #40168 ),
 .UNSPECIFIED., .F., .F.,
 ( 4, 2, 2, 4 ),
 ( 0.7435342612792388284, 0.8019765719082849742, 0.8679843812721900198, 1.000000000000000000 ),
 .UNSPECIFIED. ) ;
#40114 = ORIENTED_EDGE ( 'NONE', *, *, #28132, .T. ) ;
#40115 = CARTESIAN_POINT ( 'NONE',  ( 3.252851485128089415, -14.73889851401814788, 2.797586445667359811 ) ) ;
#40116 = DIRECTION ( 'NONE',  ( -0.8745520943968235761, 0.4849315768086558398, -5.691349986800547879E-16 ) ) ;
#40117 = CARTESIAN_POINT ( 'NONE',  ( -58.34765594471344485, -0.2451624547641084728, 0.1853313705894183983 ) ) ;
#40118 = CARTESIAN_POINT ( 'NONE',  ( 3.019445949670579665, 11.99742794009110014, 3.522755186455234000 ) ) ;
#40119 = CARTESIAN_POINT ( 'NONE',  ( 8.769168840778068130, 122.1986804192922875, 1.175795117382457677 ) ) ;
#40120 = CARTESIAN_POINT ( 'NONE',  ( -2.889499560705188319, 30.91168237226732884, 0.4695966336271347741 ) ) ;
#40121 = CARTESIAN_POINT ( 'NONE',  ( -0.1065646865916160396, 105.8844662015456777, 5.332932678536313809 ) ) ;
#40122 = EDGE_CURVE ( 'NONE', #1088, #12215, #40613, .T. ) ;
#40123 = CARTESIAN_POINT ( 'NONE',  ( -1.287880193524239658, 20.15907059199006923, -4.440276399826991849 ) ) ;
#40124 = CARTESIAN_POINT ( 'NONE',  ( 15.26387433774249835, 148.0131224598485744, 0.4327379813662103891 ) ) ;
#40125 = CARTESIAN_POINT ( 'NONE',  ( -2.483897188070747664, 106.8186250688659555, 4.725446615029760267 ) ) ;
#40126 = EDGE_CURVE ( 'NONE', #19701, #39565, #19133, .T. ) ;
#40127 = AXIS2_PLACEMENT_3D ( 'NONE', #21954, #17560, #21740 ) ;
#40128 = AXIS2_PLACEMENT_3D ( 'NONE', #39569, #16113, #177 ) ;
#40129 = CARTESIAN_POINT ( 'NONE',  ( -56.42052199906244425, 3.302738315264078128, -0.3606658556335856081 ) ) ;
#40130 = CARTESIAN_POINT ( 'NONE',  ( -2.171138432512356609, 116.2511519099119681, -0.2036645720446532970 ) ) ;
#40131 = DIRECTION ( 'NONE',  ( -0.8745520943968235761, 0.4849315768086558398, -4.268512490100410909E-16 ) ) ;
#40132 = PLANE ( 'NONE',  #31444 ) ;
#40133 = CARTESIAN_POINT ( 'NONE',  ( -11.66725022231030984, 17.14499999999999957, 5.016499999999999737 ) ) ;
#40134 = CARTESIAN_POINT ( 'NONE',  ( -30.84292043842125963, 55.46612528690534560, -1.270000000000195417 ) ) ;
#40135 = CARTESIAN_POINT ( 'NONE',  ( 7.667154907385915763, 6.987472373264454362, 3.492918021822637442 ) ) ;
#40136 = CARTESIAN_POINT ( 'NONE',  ( -46.48884030892912023, 25.85920880503905650, 1.537089628573577338 ) ) ;
#40137 = DIRECTION ( 'NONE',  ( 0.0004113621477241937948, -0.9999999153568039922, 8.219994698375953989E-06 ) ) ;
#40138 = CARTESIAN_POINT ( 'NONE',  ( -57.78461401849437351, 2.885363594410703225, -1.046722867489131048E-14 ) ) ;
#40139 = LINE ( 'NONE', #11558, #16553 ) ;
#40140 = CARTESIAN_POINT ( 'NONE',  ( -0.003746264460361951702, 116.6481217037470373, 0.1874783927187338162 ) ) ;
#40141 = VERTEX_POINT ( 'NONE', #24825 ) ;
#40142 = CARTESIAN_POINT ( 'NONE',  ( -58.20820809768405013, 1.420579653404072218, -1.355822160094615203 ) ) ;
#40143 = CARTESIAN_POINT ( 'NONE',  ( 1.589478822742971486E-15, 16.51000000000000156, 0.000000000000000000 ) ) ;
#40144 = ORIENTED_EDGE ( 'NONE', *, *, #21170, .F. ) ;
#40145 = CARTESIAN_POINT ( 'NONE',  ( -47.72737885966222393, 19.53144537861342656, -5.204668046373046586 ) ) ;
#40146 = CARTESIAN_POINT ( 'NONE',  ( 0.0005468344958371703160, 156.3034662015456604, -0.02736583427618478198 ) ) ;
#40147 = CARTESIAN_POINT ( 'NONE',  ( 5.611355841363750763, -14.32207541480874724, 3.167021961541031327 ) ) ;
#40148 = CARTESIAN_POINT ( 'NONE',  ( -20.89924265627231748, 149.3152741295656369, 1.514357740512881190 ) ) ;
#40149 = CARTESIAN_POINT ( 'NONE',  ( 15.20946960781365043, 120.7148350616293300, 0.7222319099908602880 ) ) ;
#40150 = CARTESIAN_POINT ( 'NONE',  ( 15.37733514790036438, 147.8388096571506765, 0.5071817389179859026 ) ) ;
#40151 = CARTESIAN_POINT ( 'NONE',  ( -13.46199999999999442, 12.17394877578617240, 1.841354584184931751E-15 ) ) ;
#40152 = CARTESIAN_POINT ( 'NONE',  ( 0.3959014520675726012, 0.7218480974852773402, -0.8918910426260873159 ) ) ;
#40153 = CARTESIAN_POINT ( 'NONE',  ( -22.94033276177410485, 150.1476136049543868, -0.7879714733284356454 ) ) ;
#40154 = CARTESIAN_POINT ( 'NONE',  ( -49.90208883897420833, 16.45160819380948425, -4.945622778263405905 ) ) ;
#40155 = CARTESIAN_POINT ( 'NONE',  ( -7.994219716368544226, 68.36415334912796027, -1.269999999999995577 ) ) ;
#40156 = VERTEX_POINT ( 'NONE', #34221 ) ;
#40157 = CARTESIAN_POINT ( 'NONE',  ( 2.212278878456643838, 116.2471469023566470, 0.1464055763033723367 ) ) ;
#40158 = CARTESIAN_POINT ( 'NONE',  ( -16.98902716506020028, 149.6223975874448229, 1.623990461445593114 ) ) ;
#40159 = CARTESIAN_POINT ( 'NONE',  ( -58.29423361876341403, -0.1316707858636646522, -0.3525719584774348325 ) ) ;
#40160 = CARTESIAN_POINT ( 'NONE',  ( 19.06420633224110261, 149.2349160008635351, -1.736338202726219304 ) ) ;
#40161 = CARTESIAN_POINT ( 'NONE',  ( 0.9553521702984651975, -6.993735180969975929, 0.1873809170862112405 ) ) ;
#40162 = CARTESIAN_POINT ( 'NONE',  ( -21.43631064271318465, 148.9071063441643048, -2.241374363660425306 ) ) ;
#40163 = CARTESIAN_POINT ( 'NONE',  ( -47.19936399096371105, 20.24790404726484283, -5.251082349106865443 ) ) ;
#40164 = CARTESIAN_POINT ( 'NONE',  ( 4.372915526554613130, 104.6144662015457527, 2.049786579545553877 ) ) ;
#40165 = ADVANCED_FACE ( 'NONE', ( #14810 ), #8222, .T. ) ;
#40166 = AXIS2_PLACEMENT_3D ( 'NONE', #9604, #9816, #16188 ) ;
#40167 = CARTESIAN_POINT ( 'NONE',  ( 15.22619620759357950, 139.4722935914273307, -0.9828944228028647645 ) ) ;
#40168 = CARTESIAN_POINT ( 'NONE',  ( -5.008552712180506461, 117.3993836135855560, 0.7755994290793736257 ) ) ;
#40169 = VERTEX_POINT ( 'NONE', #15020 ) ;
#40170 = CARTESIAN_POINT ( 'NONE',  ( -10.24420426168412490, 122.2012759285571946, -1.550633339661970478 ) ) ;
#40171 = CARTESIAN_POINT ( 'NONE',  ( 4.998192975942944649, -15.53260140147937030, 2.284796345537305928 ) ) ;
#40172 = CARTESIAN_POINT ( 'NONE',  ( -4.801687489738192482, 117.4019780203432646, 1.015655943361054581 ) ) ;
#40173 = CARTESIAN_POINT ( 'NONE',  ( -4.418207565432228812, 118.1647756611046276, -0.6321334375057892085 ) ) ;
#40174 = CARTESIAN_POINT ( 'NONE',  ( -50.58884987432006852, 15.93229845861179861, -5.010371253631922706 ) ) ;
#40175 = CARTESIAN_POINT ( 'NONE',  ( -26.29578028364076658, 73.87584665086983193, -1.524000000000006017 ) ) ;
#40176 = CARTESIAN_POINT ( 'NONE',  ( 13.94976549039465397, 152.5802402909829425, 2.190326936676450842 ) ) ;
#40177 = LINE ( 'NONE', #7796, #27015 ) ;
#40178 = CARTESIAN_POINT ( 'NONE',  ( 23.34372044207203700, 149.0681261006882039, 0.4664630893996631333 ) ) ;
#40179 = CIRCLE ( 'NONE', #30635, 0.3810000000000015041 ) ;
#40180 = EDGE_CURVE ( 'NONE', #21262, #22469, #11938, .T. ) ;
#40181 = CARTESIAN_POINT ( 'NONE',  ( 3.595709101656964890, 5.917279480223868404, 7.636340781540109646 ) ) ;
#40182 = CARTESIAN_POINT ( 'NONE',  ( 7.055095707297161844, 122.0164807696326790, 0.4009610655988182781 ) ) ;
#40183 = CARTESIAN_POINT ( 'NONE',  ( 22.70688998881770360, 149.0844379882532849, -0.7271790501850812216 ) ) ;
#40184 = CARTESIAN_POINT ( 'NONE',  ( -3.174366308152013705, 104.1064662015457287, -0.06343139340882732180 ) ) ;
#40185 = VECTOR ( 'NONE', #30929, 1000.000000000000000 ) ;
#40186 = LINE ( 'NONE', #33789, #9958 ) ;
#40187 = CARTESIAN_POINT ( 'NONE',  ( -58.28497307353767809, -0.1385909279409680561, -1.015887430899425772E-14 ) ) ;
#40188 = ADVANCED_FACE ( 'NONE', ( #11621 ), #27539, .T. ) ;
#40189 = CARTESIAN_POINT ( 'NONE',  ( -20.42271720105693333, 129.0384130229076334, -0.2828206407990417892 ) ) ;
#40190 = EDGE_LOOP ( 'NONE', ( #7774, #26409, #38505, #9094, #37663, #19002, #34599, #4276, #29725, #28659, #5297 ) ) ;
#40191 = CARTESIAN_POINT ( 'NONE',  ( -47.93352606754567091, 24.19884373620804396, -0.9125764105762284029 ) ) ;
#40192 = CARTESIAN_POINT ( 'NONE',  ( -7.886840516052592065, 122.0567478468350799, -0.9062200922211768317 ) ) ;
#40193 = CARTESIAN_POINT ( 'NONE',  ( -8.625062891301432444, 118.6226016915422719, 0.7970602507507228429 ) ) ;
#40194 = ORIENTED_EDGE ( 'NONE', *, *, #27489, .T. ) ;
#40195 = CARTESIAN_POINT ( 'NONE',  ( 0.8425567758001710761, 115.6909491485452719, -1.725004630648912185 ) ) ;
#40196 = CARTESIAN_POINT ( 'NONE',  ( -15.80292465353841713, 145.7390459690742830, -0.7709107363076876940 ) ) ;
#40197 = CARTESIAN_POINT ( 'NONE',  ( 4.664530445857379526, -12.43571634592606578, 1.922475882534872449 ) ) ;
#40198 = CARTESIAN_POINT ( 'NONE',  ( -15.97727112977748831, 122.8751182158008959, 0.7600457325971274880 ) ) ;
#40199 = CARTESIAN_POINT ( 'NONE',  ( -6.642767299088215313E-14, 101.1854662015457365, -1.199848199765585135E-18 ) ) ;
#40200 = CARTESIAN_POINT ( 'NONE',  ( 2.754305024641273025, 116.5489981622532127, 0.1298538421819644684 ) ) ;
#40201 = VECTOR ( 'NONE', #40791, 1000.000000000000000 ) ;
#40202 = ORIENTED_EDGE ( 'NONE', *, *, #1402, .F. ) ;
#40203 = CARTESIAN_POINT ( 'NONE',  ( -4.595132424582489605, -6.828429371805166959, -0.5093739664528403877 ) ) ;
#40204 = CARTESIAN_POINT ( 'NONE',  ( -22.66375647020928952, 150.6386093215955100, -0.4528757910175258972 ) ) ;
#40205 = CARTESIAN_POINT ( 'NONE',  ( -3.174366308152013261, 101.6934662015457320, -0.06343139340882730792 ) ) ;
#40206 = CARTESIAN_POINT ( 'NONE',  ( -13.85159022459153988, 12.96416000000000146, -5.016499999999999737 ) ) ;
#40207 = ORIENTED_EDGE ( 'NONE', *, *, #30723, .T. ) ;
#40208 = CARTESIAN_POINT ( 'NONE',  ( 5.325320179608937998, 119.5216941149903676, 1.109481133952169296 ) ) ;
#40209 = CARTESIAN_POINT ( 'NONE',  ( 1.463615122064738427, -3.970138727222522590, -4.384008014421088895 ) ) ;
#40210 = CARTESIAN_POINT ( 'NONE',  ( 6.844670616442288136, 117.9658002137636856, 0.9618333202595321652 ) ) ;
#40211 = CARTESIAN_POINT ( 'NONE',  ( -58.65598178208009017, -0.3163282088987223739, -0.3245478190977730271 ) ) ;
#40212 = CARTESIAN_POINT ( 'NONE',  ( 17.07772634048045646, 128.5677977248401476, -1.430458439683570893 ) ) ;
#40213 = CARTESIAN_POINT ( 'NONE',  ( -3.663749374568059380, -0.07195744677916669774, 2.838909333946205482 ) ) ;
#40214 = CARTESIAN_POINT ( 'NONE',  ( -3.898539657838600903, 117.3164332630744298, -0.6789226234856290398 ) ) ;
#40215 = CIRCLE ( 'NONE', #20439, 0.2540000000000018909 ) ;
#40216 = ORIENTED_EDGE ( 'NONE', *, *, #38951, .T. ) ;
#40217 = ORIENTED_EDGE ( 'NONE', *, *, #610, .F. ) ;
#40218 = CARTESIAN_POINT ( 'NONE',  ( -10.45649748849141680, 153.0728660266736370, 0.08902316335936741321 ) ) ;
#40219 = EDGE_CURVE ( 'NONE', #17174, #35234, #5852, .T. ) ;
#40220 = CARTESIAN_POINT ( 'NONE',  ( 2.293780832555937010, -15.47183500671027367, 5.912194120686782739 ) ) ;
#40221 = CIRCLE ( 'NONE', #81, 14.09699999999999420 ) ;
#40222 = DIRECTION ( 'NONE',  ( 1.011795553208986377E-16, 1.000000000000000000, -0.000000000000000000 ) ) ;
#40223 = EDGE_CURVE ( 'NONE', #20172, #23403, #33806, .T. ) ;
#40224 = CARTESIAN_POINT ( 'NONE',  ( -8.438477507926629428, 69.62414081991882142, -1.523999999999995802 ) ) ;
#40225 = ORIENTED_EDGE ( 'NONE', *, *, #30777, .F. ) ;
#40226 = CARTESIAN_POINT ( 'NONE',  ( 12.00151653869053803, 122.4500365997666336, 1.784698555944021159 ) ) ;
#40227 = CARTESIAN_POINT ( 'NONE',  ( 13.46199999999999797, 13.84300000000000175, 0.000000000000000000 ) ) ;
#40228 = CARTESIAN_POINT ( 'NONE',  ( 5.078986093043054595, 66.64146620154573952, 0.1014902294541243921 ) ) ;
#40229 = CARTESIAN_POINT ( 'NONE',  ( -21.51828904745235960, 136.6907720476960435, 0.8331038389761595830 ) ) ;
#40230 = CARTESIAN_POINT ( 'NONE',  ( -6.994280559954464849, 7.701067304790329082, -4.726517096957497444 ) ) ;
#40231 = CARTESIAN_POINT ( 'NONE',  ( 16.11589901136876790, 145.8839827664328368, 1.295141180005177750 ) ) ;
#40232 = CARTESIAN_POINT ( 'NONE',  ( 1.406077420118782567E-15, 14.60500000000000220, 0.000000000000000000 ) ) ;
#40233 = EDGE_CURVE ( 'NONE', #5054, #21592, #7983, .T. ) ;
#40234 = CARTESIAN_POINT ( 'NONE',  ( 22.34885681094289822, 150.7328461917231550, -0.2743282927392729498 ) ) ;
#40235 = CARTESIAN_POINT ( 'NONE',  ( -11.24191166894635074, 82.34025985790688651, -1.269999999999999574 ) ) ;
#40236 = CARTESIAN_POINT ( 'NONE',  ( -56.16847044329335148, 4.408804334539881964, 2.360680022881862961 ) ) ;
#40237 = VECTOR ( 'NONE', #2808, 1000.000000000000114 ) ;
#40238 = CARTESIAN_POINT ( 'NONE',  ( -57.22363667057550884, 2.289652018204080264, 1.875138655370640173 ) ) ;
#40239 = CARTESIAN_POINT ( 'NONE',  ( -58.57305159669930816, -0.1768144671344527297, 0.5299680571121552219 ) ) ;
#40240 = CARTESIAN_POINT ( 'NONE',  ( -4.533795937410928900, 118.1203770736758116, 0.4771152162569446409 ) ) ;
#40241 = CARTESIAN_POINT ( 'NONE',  ( 3.070893729975305853, 107.8345691433024172, -4.352706817367781866 ) ) ;
#40242 = PRODUCT_DEFINITION_SHAPE ( 'NONE', 'NONE',  #20881 ) ;
#40243 = ORIENTED_EDGE ( 'NONE', *, *, #8453, .T. ) ;
#40244 = CARTESIAN_POINT ( 'NONE',  ( -46.82679756180435504, 21.08486709759267086, 4.907624977305271585 ) ) ;
#40245 = CARTESIAN_POINT ( 'NONE',  ( 8.333504027011557014, 120.0758091897315722, -1.117991676638815601 ) ) ;
#40246 = CARTESIAN_POINT ( 'NONE',  ( 0.1065646865915093611, 105.8844662015456777, -5.332932678536313809 ) ) ;
#40248 = CARTESIAN_POINT ( 'NONE',  ( 4.558520316232089975, 118.0156047093444585, 0.8817180759835696602 ) ) ;
#40247 = CIRCLE ( 'NONE', #1475, 0.5080000000000000071 ) ;
#40249 = CARTESIAN_POINT ( 'NONE',  ( -9.619667158014763686, 123.8920215319950842, -0.8772578247576549026 ) ) ;
#40250 = CARTESIAN_POINT ( 'NONE',  ( -0.3620645665610385255, 115.7033447612903103, -1.764050604746122852 ) ) ;
#40251 = CARTESIAN_POINT ( 'NONE',  ( 3.413761347186222483, 117.3993835099294643, -1.238230392815611758 ) ) ;
#40252 = CARTESIAN_POINT ( 'NONE',  ( 5.103137870717143088, 114.3519703858145959, -1.758966173294684632 ) ) ;
#40253 = CARTESIAN_POINT ( 'NONE',  ( -1.456364663600036691, 120.2326517397585377, -0.4672470943647332731 ) ) ;
#40254 = CARTESIAN_POINT ( 'NONE',  ( -5.332935397695336199, 116.0444662015457311, -0.1065647409268299234 ) ) ;
#40255 = CARTESIAN_POINT ( 'NONE',  ( -45.96492958222027880, 21.02066589183244361, 4.445716362541716649 ) ) ;
#40256 = EDGE_CURVE ( 'NONE', #12250, #15268, #16818, .T. ) ;
#40257 = CARTESIAN_POINT ( 'NONE',  ( -41.09670346151922615, 23.04688172092959775, 1.270085369932517194 ) ) ;
#40258 = CARTESIAN_POINT ( 'NONE',  ( -2.869904849639449029, 156.1076442532932731, 0.07316186139488585483 ) ) ;
#40259 = CARTESIAN_POINT ( 'NONE',  ( -17.99070523305416813, 61.93444992276926797, -1.269999999999999574 ) ) ;
#40260 = CARTESIAN_POINT ( 'NONE',  ( 18.03394523526729643, 125.1493905788104684, 1.135097528960560487 ) ) ;
#40261 = CARTESIAN_POINT ( 'NONE',  ( 5.475330206976798841, 53.58606249999999704, -5.107412922131463695 ) ) ;
#40262 = CARTESIAN_POINT ( 'NONE',  ( 3.216867006742271329, -14.81339725456490264, 3.133484537391586944 ) ) ;
#40263 = CARTESIAN_POINT ( 'NONE',  ( -18.22015820038736678, 148.8986565181125457, 1.699282175587853549 ) ) ;
#40264 = CIRCLE ( 'NONE', #5557, 0.7620000000000015650 ) ;
#40265 = CARTESIAN_POINT ( 'NONE',  ( 0.9728917428133897483, -6.565010040704528649, -0.08600706860408523224 ) ) ;
#40266 = CARTESIAN_POINT ( 'NONE',  ( -16.67457936879075930, 122.7093839631038463, -0.9722687365115703084 ) ) ;
#40267 = CARTESIAN_POINT ( 'NONE',  ( -0.2169513509689728059, 19.34598098455444770, 0.9497947498389193166 ) ) ;
#40268 = ORIENTED_EDGE ( 'NONE', *, *, #25035, .F. ) ;
#40269 = CARTESIAN_POINT ( 'NONE',  ( -48.77973395026506864, 17.81645205181620639, 4.684626272830461069 ) ) ;
#40270 = CARTESIAN_POINT ( 'NONE',  ( 2.490049542275739825, 107.2224589468338536, 4.730309301830580182 ) ) ;
#40271 = CARTESIAN_POINT ( 'NONE',  ( -6.498933901768386256, 121.5572409441427482, 0.3210307352789210089 ) ) ;
#40272 = CARTESIAN_POINT ( 'NONE',  ( 4.422138279315844578, -13.30579995099732926, 3.341551838899307736 ) ) ;
#40273 = CARTESIAN_POINT ( 'NONE',  ( 2.030192889891265118, 156.8313070664539168, -1.335154060002984089 ) ) ;
#40274 = ORIENTED_EDGE ( 'NONE', *, *, #39912, .F. ) ;
#40275 = CARTESIAN_POINT ( 'NONE',  ( -1.756936351882958158, 104.6144662015457527, 4.504134836993110014 ) ) ;
#40276 = CIRCLE ( 'NONE', #21854, 3.683000000000001162 ) ;
#40277 = EDGE_CURVE ( 'NONE', #8736, #37437, #13417, .T. ) ;
#40278 = CARTESIAN_POINT ( 'NONE',  ( 3.114041961411902371, -14.44963006906317737, 3.768961988127400353 ) ) ;
#40279 = CARTESIAN_POINT ( 'NONE',  ( -4.899464968550142352, 117.6324563737643700, -0.9916011361669829771 ) ) ;
#40280 = VECTOR ( 'NONE', #17644, 1000.000000000000227 ) ;
#40281 = CARTESIAN_POINT ( 'NONE',  ( 14.20283082469467217, 138.9094276006951247, 0.1579304324436909823 ) ) ;
#40282 = ADVANCED_FACE ( 'NONE', ( #6301 ), #20211, .F. ) ;
#40283 = ORIENTED_EDGE ( 'NONE', *, *, #31348, .T. ) ;
#40284 = CARTESIAN_POINT ( 'NONE',  ( 0.4360227397040848385, 118.4074432378348689, 0.6062663470103506480 ) ) ;
#40285 = CARTESIAN_POINT ( 'NONE',  ( -5.965356522962929731, 57.14999999999999147, 5.016499999999999737 ) ) ;
#40286 = CARTESIAN_POINT ( 'NONE',  ( 1.969680065291609994, 117.3993837346511384, 1.449778539274672262 ) ) ;
#40287 = CARTESIAN_POINT ( 'NONE',  ( 0.03245814172805068509, 158.1186941186938952, -1.624338139048501217 ) ) ;
#40288 = CARTESIAN_POINT ( 'NONE',  ( 3.286349204026739468, 159.4678586119998442, -0.07386938312792008798 ) ) ;
#40289 = DIRECTION ( 'NONE',  ( -0.9998004120163608288, 0.000000000000000000, -0.01997839162482749342 ) ) ;
#40290 = CARTESIAN_POINT ( 'NONE',  ( 1.893654310830311882, -15.30438151921108236, 5.998987748567822464 ) ) ;
#40291 = CARTESIAN_POINT ( 'NONE',  ( -28.09515292912719175, 77.51021392068167870, 1.269999999999992468 ) ) ;
#40292 = CARTESIAN_POINT ( 'NONE',  ( 0.1949087904810302418, 33.82644263972942156, 0.4054292462034596034 ) ) ;
#40293 = CARTESIAN_POINT ( 'NONE',  ( 20.49864673575774532, 149.5144255282053223, 2.384675166241297717 ) ) ;
#40294 = ORIENTED_EDGE ( 'NONE', *, *, #6452, .T. ) ;
#40295 = CARTESIAN_POINT ( 'NONE',  ( -6.161128625374170831, 23.17997237347384853, 5.746845633999829950 ) ) ;
#40296 = CARTESIAN_POINT ( 'NONE',  ( 5.534489273878227422, 117.7316410755767038, -0.8034299031018331538 ) ) ;
#40297 = CARTESIAN_POINT ( 'NONE',  ( -4.252685754339997182, 122.9893884486272526, -0.2003490066864923314 ) ) ;
#40298 = DIRECTION ( 'NONE',  ( 4.017660918040594346E-17, -1.000000000000000000, -2.376309959284834438E-19 ) ) ;
#40299 = CARTESIAN_POINT ( 'NONE',  ( -11.82906070755484507, 56.41571150956207958, -5.016499999999999737 ) ) ;
#40300 = CARTESIAN_POINT ( 'NONE',  ( -0.01331772328581275200, 119.9741034315943864, 0.6664733318052136202 ) ) ;
#40301 = AXIS2_PLACEMENT_3D ( 'NONE', #21546, #28806, #31154 ) ;
#40302 = CARTESIAN_POINT ( 'NONE',  ( -4.012847786888796620, 11.73797844546971270, -2.294585225469591983 ) ) ;
#40303 = DIRECTION ( 'NONE',  ( 0.8745520943968240202, -0.4849315768086551182, 4.268512490100404500E-16 ) ) ;
#40304 = CARTESIAN_POINT ( 'NONE',  ( -3.685234504066145167, 108.9296531859112633, -3.861079628948677289 ) ) ;
#40305 = CARTESIAN_POINT ( 'NONE',  ( 3.213330078112610177, -12.77372567451348573, 1.108568753689092690 ) ) ;
#40306 = CARTESIAN_POINT ( 'NONE',  ( 2.922973558833750207, 114.3344743418335128, -2.013556875909916943 ) ) ;
#40307 = CARTESIAN_POINT ( 'NONE',  ( -6.616924617768071466E-14, 97.37546620154573418, 7.965525879364083286E-30 ) ) ;
#40308 = CARTESIAN_POINT ( 'NONE',  ( -5.817719362921545567, 56.51500000000001478, 4.384519708708647379 ) ) ;
#40309 = ORIENTED_EDGE ( 'NONE', *, *, #34161, .T. ) ;
#40310 = CARTESIAN_POINT ( 'NONE',  ( -2.763873622044191958, 104.6144662015457243, -3.957344514305136673 ) ) ;
#40311 = CARTESIAN_POINT ( 'NONE',  ( 2.515823494799488191, -15.76102479606726625, 5.403604998519412561 ) ) ;
#40312 = CARTESIAN_POINT ( 'NONE',  ( -6.324931890614157837, 157.3995435888475072, 1.705594245970836642 ) ) ;
#40313 = CARTESIAN_POINT ( 'NONE',  ( -0.3664848240473963514, 30.73350494673895739, -0.9073219246443798847 ) ) ;
#40314 = ORIENTED_EDGE ( 'NONE', *, *, #311, .F. ) ;
#40315 = CIRCLE ( 'NONE', #13110, 0.2540000000000012248 ) ;
#40316 = ORIENTED_EDGE ( 'NONE', *, *, #30576, .T. ) ;
#40317 = CARTESIAN_POINT ( 'NONE',  ( -10.28897677580358305, 57.14999999999998437, -5.016499999999999737 ) ) ;
#40318 = CARTESIAN_POINT ( 'NONE',  ( 2.813253328531081898, 121.9077826007922312, 0.2952959765298341366 ) ) ;
#40319 =( LENGTH_UNIT ( ) NAMED_UNIT ( * ) SI_UNIT ( .MILLI., .METRE. ) );
#40320 = CARTESIAN_POINT ( 'NONE',  ( -3.332096981533035684, 156.3062290909284116, 1.017430637527963810 ) ) ;
#40321 = DIRECTION ( 'NONE',  ( -0.9998004120163610509, -4.016384292689131511E-17, -0.01997839162482749689 ) ) ;
#40322 = CARTESIAN_POINT ( 'NONE',  ( 3.942276470047239467, 157.0187206368471209, -1.592783893122187155 ) ) ;
#40323 = CARTESIAN_POINT ( 'NONE',  ( -19.16059698253096144, 135.9655892003723636, -2.351238754465550862 ) ) ;
#40324 = FACE_OUTER_BOUND ( 'NONE', #10279, .T. ) ;
#40325 = CARTESIAN_POINT ( 'NONE',  ( 4.408657250832476393, 118.1814690201069311, -0.3998733507563780321 ) ) ;
#40326 = CARTESIAN_POINT ( 'NONE',  ( 7.681492011331848779, 122.2986020547093915, -0.2830363146464229263 ) ) ;
#40327 = VERTEX_POINT ( 'NONE', #35477 ) ;
#40328 = CARTESIAN_POINT ( 'NONE',  ( 3.162461164278121739, -14.57801340048104777, 3.369881103115548893 ) ) ;
#40329 = CARTESIAN_POINT ( 'NONE',  ( 1.222676017494593648E-15, 12.70000000000000284, 0.000000000000000000 ) ) ;
#40330 = AXIS2_PLACEMENT_3D ( 'NONE', #14964, #30322, #1375 ) ;
#40331 = CARTESIAN_POINT ( 'NONE',  ( -58.34429324193580868, -0.2380942604818248043, 0.1989150628791497843 ) ) ;
#40332 = CARTESIAN_POINT ( 'NONE',  ( 4.409325496788552456, -14.99073161069602911, -1.440227693534741782 ) ) ;
#40333 = CARTESIAN_POINT ( 'NONE',  ( 16.56824576912627478, 144.0643239018434940, 1.930375849691871926 ) ) ;
#40334 = CARTESIAN_POINT ( 'NONE',  ( -3.890668369019033790, 28.55756886444902065, 1.917437575001416539 ) ) ;
#40335 = CARTESIAN_POINT ( 'NONE',  ( -4.812498123319443266, 116.8297769931967309, 0.8564213435964300736 ) ) ;
#40336 = CARTESIAN_POINT ( 'NONE',  ( -3.366035089439492811, 13.68705809737886447, 3.178168622443589886 ) ) ;
#40337 = CARTESIAN_POINT ( 'NONE',  ( 9.190025975545930592, 124.2403664864748549, 0.2180328680397459196 ) ) ;
#40338 = CARTESIAN_POINT ( 'NONE',  ( 5.328530153152057913, 115.6909491485453145, 0.4168410533107074212 ) ) ;
#40339 = AXIS2_PLACEMENT_3D ( 'NONE', #829, #17616, #8045 ) ;
#40340 = CARTESIAN_POINT ( 'NONE',  ( -52.82621711067185544, 9.762356329794503296, -1.302233150175829302 ) ) ;
#40341 = CARTESIAN_POINT ( 'NONE',  ( 8.796826986025713779, 117.7047326868996180, 0.02773673846713334279 ) ) ;
#40342 = CARTESIAN_POINT ( 'NONE',  ( -5.078986093043186045, 94.32746620154571815, -0.1014902294541231709 ) ) ;
#40343 = FACE_OUTER_BOUND ( 'NONE', #24058, .T. ) ;
#40344 = CARTESIAN_POINT ( 'NONE',  ( 1.930844028328119188, -15.65960119559217745, 5.531553210582127456 ) ) ;
#40345 = CARTESIAN_POINT ( 'NONE',  ( -29.14841176306108039, 63.09186355671238999, -1.523999999996936250 ) ) ;
#40346 = CARTESIAN_POINT ( 'NONE',  ( -6.572471397769512613, 1.803772144246908127, -5.323917895317753946 ) ) ;
#40347 = FACE_OUTER_BOUND ( 'NONE', #34312, .T. ) ;
#40348 = LINE ( 'NONE', #7959, #34146 ) ;
#40349 = CARTESIAN_POINT ( 'NONE',  ( -58.23655390014408084, 1.485667022650544178, 0.5301823895692101551 ) ) ;
#40350 = CARTESIAN_POINT ( 'NONE',  ( -6.504806966450658722E-14, 124.9344662015457317, 5.107768156065721555E-17 ) ) ;
#40351 = CARTESIAN_POINT ( 'NONE',  ( -23.04498962259538075, 149.8694456586574972, -0.007884547560928519341 ) ) ;
#40352 = ORIENTED_EDGE ( 'NONE', *, *, #39413, .F. ) ;
#40353 = CARTESIAN_POINT ( 'NONE',  ( -56.90132276708389725, 4.901539372897764757, -1.453963793661438242 ) ) ;
#40354 = ORIENTED_EDGE ( 'NONE', *, *, #12395, .T. ) ;
#40355 = CARTESIAN_POINT ( 'NONE',  ( -45.65533061069547927, 20.86966646997169761, -4.138311239627009641 ) ) ;
#40356 = CARTESIAN_POINT ( 'NONE',  ( -5.308493528853332144, 121.3525139070573147, -0.1060763342189515873 ) ) ;
#40357 = CARTESIAN_POINT ( 'NONE',  ( 5.253792623460133981, -14.56763799980149976, 3.797339299194151696 ) ) ;
#40358 = CARTESIAN_POINT ( 'NONE',  ( -6.856369467415258434, 157.9234729166680040, 1.555392933271967149 ) ) ;
#40359 = AXIS2_PLACEMENT_3D ( 'NONE', #12623, #25611, #38621 ) ;
#40360 = CARTESIAN_POINT ( 'NONE',  ( 23.06466230714210752, 149.5685596498530288, 1.055262110361127270 ) ) ;
#40361 = CARTESIAN_POINT ( 'NONE',  ( 0.3722574617741854497, 117.2097358735305050, -0.3924287308447400591 ) ) ;
#40362 = CARTESIAN_POINT ( 'NONE',  ( 4.496586626007489151, 27.28078351817337222, -1.068494511273165193 ) ) ;
#40363 = CARTESIAN_POINT ( 'NONE',  ( 0.002426349801082275555, 116.5266044092193880, -0.1214244658147704548 ) ) ;
#40364 = CARTESIAN_POINT ( 'NONE',  ( -49.91451862302049136, 16.43186916766678252, -4.943002434195075345 ) ) ;
#40365 = VERTEX_POINT ( 'NONE', #12681 ) ;
#40366 = CARTESIAN_POINT ( 'NONE',  ( -8.797438454481680381, 117.7000120450088048, -0.04557994465076498081 ) ) ;
#40367 = CARTESIAN_POINT ( 'NONE',  ( -13.85457725998124801, 128.5353789189983900, 1.357273257441081071 ) ) ;
#40368 = CARTESIAN_POINT ( 'NONE',  ( -57.60581131635193231, 1.356655032538339967, -1.298406945959667214 ) ) ;
#40369 = CARTESIAN_POINT ( 'NONE',  ( 5.879203592408400958, 119.4106843418347950, -0.9594678464101259463 ) ) ;
#40370 = CARTESIAN_POINT ( 'NONE',  ( 0.7944722411588411859, -7.641519016208866866, 0.5639076281424253434 ) ) ;
#40371 = CARTESIAN_POINT ( 'NONE',  ( -2.834005798679621435, 158.8946464937287999, -1.432308184773209980 ) ) ;
#40372 = CARTESIAN_POINT ( 'NONE',  ( -47.71508057896579658, 20.49549959222711593, -5.111566084959475731 ) ) ;
#40373 = AXIS2_PLACEMENT_3D ( 'NONE', #20387, #24218, #23800 ) ;
#40374 = CARTESIAN_POINT ( 'NONE',  ( 9.903729432088722362, 123.6875948057429895, -0.6970279851166613083 ) ) ;
#40375 = CARTESIAN_POINT ( 'NONE',  ( -4.981834297919686350, 117.5302800348309518, 0.7676192988303492948 ) ) ;
#40376 = VERTEX_POINT ( 'NONE', #19272 ) ;
#40377 = CARTESIAN_POINT ( 'NONE',  ( -11.35704730865809253, 122.8492764348241337, -1.683887364911069051 ) ) ;
#40378 = CARTESIAN_POINT ( 'NONE',  ( 5.293312112441732609, -15.32963308811979886, 0.4416779358531437993 ) ) ;
#40379 = DIRECTION ( 'NONE',  ( 0.9454731675810338354, -0.3256999990547844170, 5.459396135145338185E-16 ) ) ;
#40380 = CARTESIAN_POINT ( 'NONE',  ( -4.398970153489806023, 118.1654313746710159, -0.6513127681900948707 ) ) ;
#40381 = CARTESIAN_POINT ( 'NONE',  ( -55.41603145274652320, 6.826612083464994818, -3.210495615568592420 ) ) ;
#40382 = CARTESIAN_POINT ( 'NONE',  ( -4.997525182441658664, 56.61525291752814582, -5.184946129310926466 ) ) ;
#40383 = CARTESIAN_POINT ( 'NONE',  ( 2.462641994822346803, 119.6096776070104681, 0.7191205607878171646 ) ) ;
#40384 = DIRECTION ( 'NONE',  ( 5.188838149069472160E-16, -1.699382548006136559E-16, -1.000000000000000000 ) ) ;
#40385 = CARTESIAN_POINT ( 'NONE',  ( 14.91134437181069927, 120.3281135998953459, 0.2979641475761142244 ) ) ;
#40386 = CARTESIAN_POINT ( 'NONE',  ( 8.383109624418931816, 7.835852165998051788, -1.087619381312709077 ) ) ;
#40387 = CARTESIAN_POINT ( 'NONE',  ( 1.571702145576592935, 120.8584627942791627, 0.1987642453017053890 ) ) ;
#40388 = CIRCLE ( 'NONE', #21989, 0.6350000000000008971 ) ;
#40389 = CARTESIAN_POINT ( 'NONE',  ( 18.09030135340791290, 154.0913862843578670, -0.7524810965364957527 ) ) ;
#40390 = CARTESIAN_POINT ( 'NONE',  ( 18.35410564743290607, 77.35382415001784295, 1.904999999999988480 ) ) ;
#40391 = CARTESIAN_POINT ( 'NONE',  ( -0.02551629668048742416, 118.7629491485454025, 1.276939826301574987 ) ) ;
#40392 = AXIS2_PLACEMENT_3D ( 'NONE', #7211, #31557, #6999 ) ;
#40393 = CARTESIAN_POINT ( 'NONE',  ( -57.89731077922510849, 0.5615449381113774008, 0.05962325924456875204 ) ) ;
#40394 = CARTESIAN_POINT ( 'NONE',  ( -15.52360445758517216, 120.7153972339879715, -0.2596658046059212577 ) ) ;
#40395 = VERTEX_POINT ( 'NONE', #25875 ) ;
#40396 = CARTESIAN_POINT ( 'NONE',  ( -46.81005371095113077, 25.73327194510126859, -1.583310528698486541 ) ) ;
#40397 = CARTESIAN_POINT ( 'NONE',  ( 5.895458498755588472, 121.3261075308788719, -0.1611362123841119653 ) ) ;
#40398 = CARTESIAN_POINT ( 'NONE',  ( -17.31476582418722643, 62.07284264934779827, -1.523999999999999355 ) ) ;
#40399 = ORIENTED_EDGE ( 'NONE', *, *, #4821, .T. ) ;
#40400 = CARTESIAN_POINT ( 'NONE',  ( -5.586884702347496123, 92.04146620154574521, -0.1116392523995361624 ) ) ;
#40401 = CARTESIAN_POINT ( 'NONE',  ( -2.922188055539197915, 156.0861408873597327, -0.2775485887099102267 ) ) ;
#40402 = CARTESIAN_POINT ( 'NONE',  ( 4.778187575955942457, -13.11831155531867310, 3.026993680286476973 ) ) ;
#40403 = CARTESIAN_POINT ( 'NONE',  ( -19.46267448186344495, 131.9512773411433670, 1.172478082078345585 ) ) ;
#40404 = CARTESIAN_POINT ( 'NONE',  ( -6.431420355030265265E-14, 156.3034662015457172, 9.897580308537652682E-17 ) ) ;
#40405 = CARTESIAN_POINT ( 'NONE',  ( 23.10027255048446548, 149.8968678342272653, 0.6153025774343642285 ) ) ;
#40406 = CARTESIAN_POINT ( 'NONE',  ( 12.82793160447645953, 133.7433403788203066, 0.3179556874975825731 ) ) ;
#40407 = EDGE_LOOP ( 'NONE', ( #40677, #8877, #30531, #21647 ) ) ;
#40408 = CARTESIAN_POINT ( 'NONE',  ( 0.9733856798199480576, 17.99895565637743999, 0.09873697238165508872 ) ) ;
#40409 = CARTESIAN_POINT ( 'NONE',  ( -8.075047650969624513, 158.6620026115301698, -0.1796671307923021765 ) ) ;
#40410 = CARTESIAN_POINT ( 'NONE',  ( -41.09670346151853693, 23.04688172093031540, -1.270085369932520303 ) ) ;
#40411 = ORIENTED_EDGE ( 'NONE', *, *, #8199, .T. ) ;
#40412 = DIRECTION ( 'NONE',  ( 0.02487920782528813338, -0.9876883405951415451, 0.1544434099286914330 ) ) ;
#40413 = VERTEX_POINT ( 'NONE', #38881 ) ;
#40414 = CARTESIAN_POINT ( 'NONE',  ( -6.814166505432768695, 120.4085755475616253, 0.9136569436695998192 ) ) ;
#40415 = CARTESIAN_POINT ( 'NONE',  ( -3.663749374568059380, -0.07195744677916669774, 2.838909333946205482 ) ) ;
#40416 = CARTESIAN_POINT ( 'NONE',  ( 21.80715381475361170, 148.2155681941778482, 2.148825447453798443 ) ) ;
#40417 = CARTESIAN_POINT ( 'NONE',  ( -58.66375602224954378, -0.3143320623655576629, -0.3221285174456221534 ) ) ;
#40418 = CARTESIAN_POINT ( 'NONE',  ( 20.71566368020593174, 149.2407879669073054, -1.563226885547172706 ) ) ;
#40419 = AXIS2_PLACEMENT_3D ( 'NONE', #40259, #17436, #17642 ) ;
#40420 = CARTESIAN_POINT ( 'NONE',  ( -3.074427775304182209, -11.96646105551300643, -3.469969274305642060 ) ) ;
#40421 = CARTESIAN_POINT ( 'NONE',  ( -21.90872843939991554, 150.3855106993079005, -1.734217137259093100 ) ) ;
#40422 = EDGE_CURVE ( 'NONE', #15671, #40763, #40637, .T. ) ;
#40423 = VERTEX_POINT ( 'NONE', #28870 ) ;
#40425 = AXIS2_PLACEMENT_3D ( 'NONE', #20285, #30728, #7954 ) ;
#40424 = CARTESIAN_POINT ( 'NONE',  ( -4.275377040554547037, 155.8374496918941077, 0.1508172661092593292 ) ) ;
#40426 = CARTESIAN_POINT ( 'NONE',  ( 6.307811598796486230, -13.53853427790793695, 1.133914056348525934 ) ) ;
#40427 = DIRECTION ( 'NONE',  ( -4.017660918040594346E-17, 1.000000000000000000, 2.376309959284834438E-19 ) ) ;
#40428 = AXIS2_PLACEMENT_3D ( 'NONE', #17262, #20862, #21071 ) ;
#40429 = DIRECTION ( 'NONE',  ( 4.017660918040594346E-17, -1.000000000000000000, -2.376309959284834438E-19 ) ) ;
#40430 = ADVANCED_FACE ( 'NONE', ( #35068 ), #1187, .T. ) ;
#40431 = ORIENTED_EDGE ( 'NONE', *, *, #13028, .T. ) ;
#40432 = CARTESIAN_POINT ( 'NONE',  ( 14.20181026158647519, 125.7140216354555804, 2.028863013303968899 ) ) ;
#40433 = CARTESIAN_POINT ( 'NONE',  ( -1.915954025944994433E-14, 30.83083951148100255, 1.904999999999999805 ) ) ;
#40434 = CIRCLE ( 'NONE', #17273, 6.905625000000000568 ) ;
#40435 = CARTESIAN_POINT ( 'NONE',  ( -30.54923999206217289, 56.28999798340426253, -1.270000000000004903 ) ) ;
#40436 = CARTESIAN_POINT ( 'NONE',  ( -1.024802081479867066, 117.0751458430253393, 0.3787107017154778266 ) ) ;
#40437 = CARTESIAN_POINT ( 'NONE',  ( -8.002357889267953439, 8.121853428443936096, -2.619265908643666929 ) ) ;
#40438 = CARTESIAN_POINT ( 'NONE',  ( 13.61103386154286810, 134.2686865373913463, 1.213594671188916951 ) ) ;
#40439 = CYLINDRICAL_SURFACE ( 'NONE', #906, 7.461249999999999716 ) ;
#40440 = CARTESIAN_POINT ( 'NONE',  ( 23.05353557640024675, 148.9204423966469335, -0.3945749818456246172 ) ) ;
#40441 = CARTESIAN_POINT ( 'NONE',  ( 8.515285667870288113E-16, 8.844871939465425825, 0.000000000000000000 ) ) ;
#40442 = CIRCLE ( 'NONE', #30204, 2.540000000000000480 ) ;
#40443 = CARTESIAN_POINT ( 'NONE',  ( -57.86639066231883533, 0.7938686018777963982, 1.024763737755092885 ) ) ;
#40444 = CARTESIAN_POINT ( 'NONE',  ( -6.784104592523965728E-14, 136.3644662015457527, 7.159772606002533724E-18 ) ) ;
#40445 = CARTESIAN_POINT ( 'NONE',  ( -58.55221842960730783, 0.5754175076986972615, 0.9757793345693576148 ) ) ;
#40446 = CARTESIAN_POINT ( 'NONE',  ( -58.22293861823094829, 0.5799661241833895531, 1.107036107443613693 ) ) ;
#40447 = EDGE_CURVE ( 'NONE', #1824, #29132, #1870, .T. ) ;
#40448 = CARTESIAN_POINT ( 'NONE',  ( 23.36555825341164550, 148.7788340588663800, 0.4668994608413311043 ) ) ;
#40449 = CARTESIAN_POINT ( 'NONE',  ( -4.121280158250598014, 118.2429491485453497, 0.1829298354757566414 ) ) ;
#40450 = CARTESIAN_POINT ( 'NONE',  ( 0.1066493941974242521, 105.7853621660184444, -5.332931186019217229 ) ) ;
#40451 = ORIENTED_EDGE ( 'NONE', *, *, #11857, .F. ) ;
#40452 = CARTESIAN_POINT ( 'NONE',  ( -53.09398923718962493, 10.65108322687173548, 3.938325876039757478 ) ) ;
#40453 = EDGE_CURVE ( 'NONE', #449, #18529, #9341, .T. ) ;
#40454 = CARTESIAN_POINT ( 'NONE',  ( 4.381439635116813669, 119.4686423241179085, -0.7540022720711342386 ) ) ;
#40455 = CARTESIAN_POINT ( 'NONE',  ( -5.771537640388904045, 118.4310156723767307, -0.6642225483502960381 ) ) ;
#40456 = CARTESIAN_POINT ( 'NONE',  ( 4.286528689365628253, 118.2141904594688384, 0.5114333612981697419 ) ) ;
#40457 = CARTESIAN_POINT ( 'NONE',  ( -16.14702439603941286, 146.0959698922748942, -1.294960982472433519 ) ) ;
#40458 = CARTESIAN_POINT ( 'NONE',  ( -1.357158281331605432, 115.7027986320083812, -1.737098550677430131 ) ) ;
#40459 = ADVANCED_FACE ( 'NONE', ( #5890 ), #8642, .T. ) ;
#40460 = CARTESIAN_POINT ( 'NONE',  ( 8.216926545874459364, 117.5004104479096583, 0.1641937475849289951 ) ) ;
#40461 = EDGE_LOOP ( 'NONE', ( #28925, #2877, #22971, #27937 ) ) ;
#40462 = CARTESIAN_POINT ( 'NONE',  ( 5.222556791543245147, 115.4535745449993982, -1.305545271932168960 ) ) ;
#40463 = CARTESIAN_POINT ( 'NONE',  ( -5.855671506236725499, 121.0368588677253143, -0.7388637662663294359 ) ) ;
#40464 = CARTESIAN_POINT ( 'NONE',  ( -41.05190940400897404, 23.09449711912554903, -1.270000000000012896 ) ) ;
#40465 = CARTESIAN_POINT ( 'NONE',  ( -45.11690586071527775, 21.31720619196439159, 3.746636771226976137 ) ) ;
#40466 = DIRECTION ( 'NONE',  ( -5.188838149069471174E-16, 1.699382548006136313E-16, 1.000000000000000000 ) ) ;
#40467 = CARTESIAN_POINT ( 'NONE',  ( -14.11998566707450564, 138.8091548059119020, -0.08316428514401870420 ) ) ;
#40468 = CARTESIAN_POINT ( 'NONE',  ( 22.26995438616699374, 150.5193240506149550, 1.407572089812798799 ) ) ;
#40469 = CARTESIAN_POINT ( 'NONE',  ( 6.059261036834384662, 88.73331249999999670, -5.016499999999999737 ) ) ;
#40471 = CARTESIAN_POINT ( 'NONE',  ( 21.26362230212569671, 150.1117090729339623, -1.276404781699089774 ) ) ;
#40470 = CARTESIAN_POINT ( 'NONE',  ( 2.459637058406862309, -15.11974833578012856, 4.824092508607692231 ) ) ;
#40472 = CARTESIAN_POINT ( 'NONE',  ( -5.875153347143380778, 119.9178398404649926, 0.8959128733076282547 ) ) ;
#40473 = CARTESIAN_POINT ( 'NONE',  ( -0.8332992110815757858, -10.66407516643697306, 0.5056687530665907593 ) ) ;
#40474 = CARTESIAN_POINT ( 'NONE',  ( -4.811924804297874836, 117.0737178285515654, -0.5427311436463462258 ) ) ;
#40475 = CARTESIAN_POINT ( 'NONE',  ( -0.5956917769015268593, 15.89737491555829685, -0.7703063551142234067 ) ) ;
#40476 = EDGE_LOOP ( 'NONE', ( #41543, #16653, #32726, #38870 ) ) ;
#40477 = CARTESIAN_POINT ( 'NONE',  ( -51.79385399617232366, 10.81633633057992050, 0.6965991018155703873 ) ) ;
#40478 = CARTESIAN_POINT ( 'NONE',  ( -8.277497327055032272, 122.7564308547279666, 0.2971990107970639561 ) ) ;
#40479 = CARTESIAN_POINT ( 'NONE',  ( 4.295506980234458538, -13.52603301450379369, 3.694598940018447575 ) ) ;
#40480 = CARTESIAN_POINT ( 'NONE',  ( 0.02615319344468031854, 156.8698190429800832, -1.308812744920978099 ) ) ;
#40481 = ORIENTED_EDGE ( 'NONE', *, *, #39425, .F. ) ;
#40482 = CARTESIAN_POINT ( 'NONE',  ( 3.040151308551036990, 115.7029506951511735, 1.666347003474312638 ) ) ;
#40483 = CARTESIAN_POINT ( 'NONE',  ( 3.226040172055379518, -13.73821525131127608, 2.149215086980220235 ) ) ;
#40484 = DIRECTION ( 'NONE',  ( 0.4849315768086425726, 0.8745520943968309036, 1.030032898892908012E-16 ) ) ;
#40485 = CARTESIAN_POINT ( 'NONE',  ( 8.961118498052918824, 123.9105667600146177, 0.1452814789513761640 ) ) ;
#40486 = EDGE_LOOP ( 'NONE', ( #6243, #41333, #37554, #27280 ) ) ;
#40487 = CARTESIAN_POINT ( 'NONE',  ( 15.97272115206776633, 153.3736753708079732, 2.320099718173297632 ) ) ;
#40488 = CARTESIAN_POINT ( 'NONE',  ( 5.166455574615658186, 114.8007926982540994, 1.419721048087801307 ) ) ;
#40489 = CARTESIAN_POINT ( 'NONE',  ( -9.138499898145774125, 117.7878261280527710, -0.1826089763859923554 ) ) ;
#40490 = CARTESIAN_POINT ( 'NONE',  ( -14.60499999999999865, 71.11999999999999034, 5.714999999999997193 ) ) ;
#40491 = EDGE_CURVE ( 'NONE', #37954, #1374, #35693, .T. ) ;
#40492 = CARTESIAN_POINT ( 'NONE',  ( 17.11470313646601227, 122.7072422303320707, 0.09880859551014498088 ) ) ;
#40493 = EDGE_CURVE ( 'NONE', #27477, #23556, #31105, .T. ) ;
#40494 = DIRECTION ( 'NONE',  ( 0.8745520943968230210, -0.4849315768086570611, 6.829619984160674809E-16 ) ) ;
#40495 = CARTESIAN_POINT ( 'NONE',  ( 2.048596186826366683, -15.20054017908126198, 5.929173703500263848 ) ) ;
#40496 = CARTESIAN_POINT ( 'NONE',  ( 4.812022206586005879, 117.4092931151362933, 1.196645100868244604 ) ) ;
#40497 = DIRECTION ( 'NONE',  ( -4.017660918040594346E-17, 1.000000000000000000, 2.376309959284834438E-19 ) ) ;
#40498 = CARTESIAN_POINT ( 'NONE',  ( -4.677964096319726650, 117.9838868299774362, 0.6915560018011523979 ) ) ;
#40499 = ORIENTED_EDGE ( 'NONE', *, *, #26963, .T. ) ;
#40500 = CARTESIAN_POINT ( 'NONE',  ( -6.940074030747619638, 22.95585651114365788, 4.785772612677765991 ) ) ;
#40501 = EDGE_CURVE ( 'NONE', #5241, #24814, #28657, .T. ) ;
#40502 = CARTESIAN_POINT ( 'NONE',  ( 2.700640353861210929, 117.7589353780938808, -0.7017837913142891404 ) ) ;
#40503 = CARTESIAN_POINT ( 'NONE',  ( -1.464138133146304366, 108.1711930243730109, -4.389422119207357476 ) ) ;
#40504 = CARTESIAN_POINT ( 'NONE',  ( 4.946784285683848204, 117.5302610941451178, 0.9662579091233235440 ) ) ;
#40505 = CARTESIAN_POINT ( 'NONE',  ( -4.666417123046072035, 117.8349074441706534, -1.040161417730997462 ) ) ;
#40506 = CARTESIAN_POINT ( 'NONE',  ( -4.888105396971740291, 104.6144662015479270, 2.142115408852796499 ) ) ;
#40507 = CARTESIAN_POINT ( 'NONE',  ( -2.395914033174281865, 1.367755174955888275, -3.957843245732672877 ) ) ;
#40508 = ADVANCED_FACE ( 'NONE', ( #25471 ), #32452, .T. ) ;
#40509 = FACE_OUTER_BOUND ( 'NONE', #12834, .T. ) ;
#40510 = CARTESIAN_POINT ( 'NONE',  ( -5.066192932591571108, 115.6909491485453003, 1.197525932795551640 ) ) ;
#40511 = CARTESIAN_POINT ( 'NONE',  ( 3.853068500771395399, -13.31557002055877525, 3.124774401994960815 ) ) ;
#40512 = CARTESIAN_POINT ( 'NONE',  ( 4.073291749555208341, 117.6466181296975151, -0.7504383534773489961 ) ) ;
#40513 = CARTESIAN_POINT ( 'NONE',  ( -1.505490909297014790, 33.15442552098056694, 4.097489486992727414 ) ) ;
#40514 = VECTOR ( 'NONE', #22547, 1000.000000000000000 ) ;
#40515 = CARTESIAN_POINT ( 'NONE',  ( -0.7499141588179909501, 115.7030497829226903, 1.729243208713743041 ) ) ;
#40516 = ORIENTED_EDGE ( 'NONE', *, *, #38287, .T. ) ;
#40517 = CARTESIAN_POINT ( 'NONE',  ( -2.893454522978812893, 104.6144662015457243, -3.863863340516500600 ) ) ;
#40518 = CARTESIAN_POINT ( 'NONE',  ( 3.501109451447479870, -15.63356008979879874, 3.898959153382382858 ) ) ;
#40519 = CARTESIAN_POINT ( 'NONE',  ( -19.74506706576321236, 148.5147687316951135, 1.724011100433736177 ) ) ;
#40520 = EDGE_CURVE ( 'NONE', #21812, #7720, #38678, .T. ) ;
#40521 = CARTESIAN_POINT ( 'NONE',  ( -0.5455758836206960893, 21.45819190514113117, -0.8097498057291211415 ) ) ;
#40522 = ORIENTED_EDGE ( 'NONE', *, *, #22688, .F. ) ;
#40523 = ORIENTED_EDGE ( 'NONE', *, *, #31332, .F. ) ;
#40524 = FACE_OUTER_BOUND ( 'NONE', #12034, .T. ) ;
#40525 = CARTESIAN_POINT ( 'NONE',  ( 2.282361306983733407, 118.7862729053988318, 0.7764855222020032866 ) ) ;
#40526 = CARTESIAN_POINT ( 'NONE',  ( -15.62653493684497796, 149.1167355181319181, 1.114087811593069910 ) ) ;
#40527 = CARTESIAN_POINT ( 'NONE',  ( -6.474089935681887051E-14, 69.94346620154573202, 3.752704589293910110E-29 ) ) ;
#40528 = CARTESIAN_POINT ( 'NONE',  ( 4.574931840464235400, 118.0742404603594053, -0.6030673501148580140 ) ) ;
#40529 = CARTESIAN_POINT ( 'NONE',  ( 3.413396786258054316, 119.6896249646678569, -0.6770706109030819597 ) ) ;
#40530 = CARTESIAN_POINT ( 'NONE',  ( -13.02489573621956076, 155.4510764517707742, -2.156236249524808635 ) ) ;
#40531 = CARTESIAN_POINT ( 'NONE',  ( -5.008987216574991130, 117.3966124399498199, 0.7756614662348499944 ) ) ;
#40532 = CARTESIAN_POINT ( 'NONE',  ( 4.318480543059425969, 118.2119050262681981, -0.3228229928774009605 ) ) ;
#40533 = CARTESIAN_POINT ( 'NONE',  ( 9.417214020844189903, 124.0858766813489780, -0.2349654282845519138 ) ) ;
#40534 = VERTEX_POINT ( 'NONE', #6502 ) ;
#40535 = CARTESIAN_POINT ( 'NONE',  ( 2.770264620702337588, -13.86593384134129892, 0.2159450460461957433 ) ) ;
#40536 = CARTESIAN_POINT ( 'NONE',  ( -4.958806897238241085, 117.4102282907815606, 0.9054230299057887121 ) ) ;
#40537 = CARTESIAN_POINT ( 'NONE',  ( -54.14414085402405163, 8.624088997049140559, 3.578441826534893622 ) ) ;
#40538 = AXIS2_PLACEMENT_3D ( 'NONE', #28068, #21445, #24445 ) ;
#40539 = CARTESIAN_POINT ( 'NONE',  ( -0.09930934064637705894, -13.04092083763876175, -4.623607705436294957 ) ) ;
#40540 = CARTESIAN_POINT ( 'NONE',  ( 4.351716102370827066, 120.3584862571861436, 0.7474562918332060546 ) ) ;
#40541 = CARTESIAN_POINT ( 'NONE',  ( -3.748619050207897985, 28.91994025391836942, 2.520532616727765518 ) ) ;
#40542 = CARTESIAN_POINT ( 'NONE',  ( -0.1065646865916159702, 105.8844662015456777, 5.332932678536312032 ) ) ;
#40543 = CARTESIAN_POINT ( 'NONE',  ( -3.812863311134618183, 2.017465188139291765, -2.614655560905410958 ) ) ;
#40544 = CARTESIAN_POINT ( 'NONE',  ( 11.06205061746896234, 128.0319838675845290, 0.2615737156286701004 ) ) ;
#40545 = CARTESIAN_POINT ( 'NONE',  ( -11.48503488083560065, 55.92196062030127024, 5.016500000000108983 ) ) ;
#40546 = CARTESIAN_POINT ( 'NONE',  ( -57.50808096206083775, 1.366199858870195794, -0.4699486091021616296 ) ) ;
#40547 = CARTESIAN_POINT ( 'NONE',  ( -8.790893838487704670, 117.7047839374624516, -0.3241293065953896879 ) ) ;
#40548 = CARTESIAN_POINT ( 'NONE',  ( -11.58677707360137532, 55.24499999999999034, 4.474811398758258285 ) ) ;
#40549 = DIRECTION ( 'NONE',  ( -0.8745520943968243532, 0.4849315768086547296, -5.361993529360573944E-16 ) ) ;
#40550 = CARTESIAN_POINT ( 'NONE',  ( -1.506244733641594280, 106.1067062490223947, 5.119529036520902743 ) ) ;
#40551 = CARTESIAN_POINT ( 'NONE',  ( -20.05275907367747124, 79.68882802557934042, -1.524000000000003796 ) ) ;
#40552 = CARTESIAN_POINT ( 'NONE',  ( -5.746845633966660039, 1.589972373264088246, -6.161128625535090109 ) ) ;
#40553 = ADVANCED_FACE ( 'NONE', ( #15864 ), #33164, .T. ) ;
#40554 = CARTESIAN_POINT ( 'NONE',  ( -5.224225543104921599, 57.14999999999898250, 5.327462464253450491 ) ) ;
#40555 = CARTESIAN_POINT ( 'NONE',  ( 1.852819980464847305, -15.24972552306870455, 5.408883774200016425 ) ) ;
#40556 = CARTESIAN_POINT ( 'NONE',  ( 0.01046636458941188792, 120.7331730230139755, -0.5237796829256086140 ) ) ;
#40557 = CARTESIAN_POINT ( 'NONE',  ( -15.85309526068962427, 121.4040080620525117, 0.2080479070310633782 ) ) ;
#40558 = ORIENTED_EDGE ( 'NONE', *, *, #32619, .T. ) ;
#40559 = FACE_OUTER_BOUND ( 'NONE', #792, .T. ) ;
#40560 = EDGE_CURVE ( 'NONE', #28559, #29332, #34851, .T. ) ;
#40561 = ORIENTED_EDGE ( 'NONE', *, *, #8089, .F. ) ;
#40562 = CARTESIAN_POINT ( 'NONE',  ( -46.50210365331269458, 20.51386735865872168, -4.739171082384393330 ) ) ;
#40563 = CARTESIAN_POINT ( 'NONE',  ( -6.439798515484507670E-14, 156.3034662015457172, 9.575285601066443938E-17 ) ) ;
#40564 = CARTESIAN_POINT ( 'NONE',  ( 3.432440172432007053, -15.40242305089609154, 5.447709670318832131 ) ) ;
#40565 = CARTESIAN_POINT ( 'NONE',  ( -1.161715739485909671, 117.9723128000925669, 0.5854012653586094794 ) ) ;
#40566 = CARTESIAN_POINT ( 'NONE',  ( 6.890728787288526114, 117.8105958006179890, -0.6119090536800845248 ) ) ;
#40567 = CARTESIAN_POINT ( 'NONE',  ( -1.178223178616622402, 14.53665720681882689, 4.476207649055042204 ) ) ;
#40568 = CARTESIAN_POINT ( 'NONE',  ( -13.37536684427251110, 156.9592627042916604, -0.5421920129525307219 ) ) ;
#40569 = CARTESIAN_POINT ( 'NONE',  ( -49.52378801310364054, 17.04469588244878153, -5.022789431048734876 ) ) ;
#40570 = ORIENTED_EDGE ( 'NONE', *, *, #3677, .F. ) ;
#40571 = CIRCLE ( 'NONE', #6563, 18.32410244842765934 ) ;
#40572 = CARTESIAN_POINT ( 'NONE',  ( 2.183041108267496977, 116.1870934937200985, 0.05032534355729129799 ) ) ;
#40573 = CARTESIAN_POINT ( 'NONE',  ( -17.81274246965193342, 147.0764175921665640, 1.531068679518140518 ) ) ;
#40574 = CARTESIAN_POINT ( 'NONE',  ( -48.09695194791964923, 19.08878339914985034, -5.210713465316049842 ) ) ;
#40575 = CARTESIAN_POINT ( 'NONE',  ( 19.17469122182624375, 148.2829752965438956, -1.735408567215429132 ) ) ;
#40576 = CARTESIAN_POINT ( 'NONE',  ( -3.058686590880046907, 117.8293475852256904, -0.7841115193421154261 ) ) ;
#40577 = CARTESIAN_POINT ( 'NONE',  ( -45.14658554404967106, 22.88857079803865346, -2.562886992506571371 ) ) ;
#40578 = CARTESIAN_POINT ( 'NONE',  ( 16.33963436279736214, 146.4745453488731357, -0.7896242330311487034 ) ) ;
#40579 = ORIENTED_EDGE ( 'NONE', *, *, #25944, .T. ) ;
#40580 = CARTESIAN_POINT ( 'NONE',  ( -18.09674421129296817, 146.7121067869193496, -2.346545542165937803 ) ) ;
#40581 = CARTESIAN_POINT ( 'NONE',  ( 3.501109451447479870, -15.63356008979879874, 3.898959153382382858 ) ) ;
#40582 = CARTESIAN_POINT ( 'NONE',  ( -4.512835031468954483, 118.1143071752745612, -0.7003032011746382901 ) ) ;
#40583 = CARTESIAN_POINT ( 'NONE',  ( -57.57967628038989005, 1.451576601202181349, -1.494865757154152153 ) ) ;
#40584 = CARTESIAN_POINT ( 'NONE',  ( -4.908928425608774404, 117.5479188556219441, 0.9160482988203918486 ) ) ;
#40585 = CARTESIAN_POINT ( 'NONE',  ( 8.234130529647114116, 121.1361926620737393, 1.330377128061140057 ) ) ;
#40586 = CARTESIAN_POINT ( 'NONE',  ( 2.744962145539584952, 116.5337465564440578, 0.01469834071105289089 ) ) ;
#40587 = VECTOR ( 'NONE', #1897, 1000.000000000000000 ) ;
#40588 = CARTESIAN_POINT ( 'NONE',  ( 8.218723488459346527, -2.309819447571417772, 1.932697321913255717 ) ) ;
#40589 = CARTESIAN_POINT ( 'NONE',  ( 4.529648377620876687, 121.1059516323014549, 0.2990124396216896074 ) ) ;
#40590 = CARTESIAN_POINT ( 'NONE',  ( -57.93941708942283952, 2.052042089854988483, -1.628789306319529118 ) ) ;
#40591 = CIRCLE ( 'NONE', #33786, 0.2539999999999992264 ) ;
#40592 = CARTESIAN_POINT ( 'NONE',  ( -41.31984638471809745, 22.80761424078405497, -1.396846000931804666 ) ) ;
#40593 = FACE_OUTER_BOUND ( 'NONE', #20792, .T. ) ;
#40594 = CARTESIAN_POINT ( 'NONE',  ( -5.332935397695332647, 62.83146620154573014, -0.1065647409268298401 ) ) ;
#40595 = CARTESIAN_POINT ( 'NONE',  ( -57.66977034847604955, 1.126272260461025354, 0.8071799157849385287 ) ) ;
#40596 = CARTESIAN_POINT ( 'NONE',  ( -23.34248308131520488, 149.0646716566344026, -0.3893018266236027980 ) ) ;
#40597 = ORIENTED_EDGE ( 'NONE', *, *, #198, .T. ) ;
#40598 = CARTESIAN_POINT ( 'NONE',  ( -47.53841933257975683, 25.36174273411122115, -0.2940116119275095752 ) ) ;
#40599 = CARTESIAN_POINT ( 'NONE',  ( -5.858775649260424601, 121.3022210319751082, -0.4117851423131264066 ) ) ;
#40600 = CARTESIAN_POINT ( 'NONE',  ( -8.413874481325345656, 119.6811429777991265, 1.089663159344654630 ) ) ;
#40601 = ORIENTED_EDGE ( 'NONE', *, *, #1147, .F. ) ;
#40602 = CARTESIAN_POINT ( 'NONE',  ( 0.6390139148044564621, 115.7029491485453576, -1.736660153015813890 ) ) ;
#40603 = CARTESIAN_POINT ( 'NONE',  ( -1.583718294068570343, 120.9073379818811134, -0.1636693232558001920 ) ) ;
#40604 = CARTESIAN_POINT ( 'NONE',  ( 2.226119369219526689, -15.10343733042141068, 5.886803469647748699 ) ) ;
#40605 = CARTESIAN_POINT ( 'NONE',  ( -15.81089186882093856, 155.0373533369262589, 1.166412807380551531 ) ) ;
#40606 = CIRCLE ( 'NONE', #14734, 0.2540000000000027236 ) ;
#40607 = DIRECTION ( 'NONE',  ( 0.9511648638205648654, 0.3086833358527896753, 8.537024980200876052E-16 ) ) ;
#40608 = CARTESIAN_POINT ( 'NONE',  ( 22.52498503541040975, 150.7873321363286152, 0.6028683204863922729 ) ) ;
#40609 = CARTESIAN_POINT ( 'NONE',  ( 15.78228220284642269, 146.2362006864767636, 0.3825322408708758948 ) ) ;
#40610 = DIRECTION ( 'NONE',  ( 0.9998004120163610509, 4.016384292689131511E-17, 0.01997839162482749689 ) ) ;
#40611 = CARTESIAN_POINT ( 'NONE',  ( -0.4908008364610317309, 30.95719094559541418, -0.8433761395939078920 ) ) ;
#40612 = CARTESIAN_POINT ( 'NONE',  ( -13.43562511198114784, 156.9186530619738562, -0.2898375456858039434 ) ) ;
#40613 = LINE ( 'NONE', #24399, #1099 ) ;
#40614 = ORIENTED_EDGE ( 'NONE', *, *, #34237, .T. ) ;
#40615 = FACE_OUTER_BOUND ( 'NONE', #31419, .T. ) ;
#40616 = ORIENTED_EDGE ( 'NONE', *, *, #16981, .F. ) ;
#40617 = CARTESIAN_POINT ( 'NONE',  ( -6.275263529460059608, 119.2322458688779250, 1.005175755799972315 ) ) ;
#40618 = CARTESIAN_POINT ( 'NONE',  ( -3.538659794179211726, -11.74154716455626257, -2.972011832598964176 ) ) ;
#40619 = CARTESIAN_POINT ( 'NONE',  ( 18.27285712481717539, 128.6097515361309149, 1.839992588890194458 ) ) ;
#40620 = CARTESIAN_POINT ( 'NONE',  ( -58.33992048227231209, -0.2288887037932701984, -0.2155571079148838054 ) ) ;
#40621 = AXIS2_PLACEMENT_3D ( 'NONE', #11430, #5075, #2076 ) ;
#40622 = CARTESIAN_POINT ( 'NONE',  ( 20.46161261025634204, 147.6366098820875266, -1.667455336067830585 ) ) ;
#40623 = CARTESIAN_POINT ( 'NONE',  ( -1.191460153279743750, 25.61543958765020434, -8.344265960924422743 ) ) ;
#40624 = CARTESIAN_POINT ( 'NONE',  ( -5.450899203174041752, 159.0107326448372191, -0.9576670044529981274 ) ) ;
#40625 = CARTESIAN_POINT ( 'NONE',  ( 4.969807616941213091, 117.5383056595475466, -0.8108227939444502264 ) ) ;
#40626 = ORIENTED_EDGE ( 'NONE', *, *, #37129, .T. ) ;
#40627 = AXIS2_PLACEMENT_3D ( 'NONE', #24380, #40801, #15001 ) ;
#40628 = CARTESIAN_POINT ( 'NONE',  ( -10.40586874195283151, 126.0814211662656419, 0.04952998093763452681 ) ) ;
#40629 = CARTESIAN_POINT ( 'NONE',  ( 4.513795256570364067, -15.26848473984131260, 4.551867270201407578 ) ) ;
#40630 = CARTESIAN_POINT ( 'NONE',  ( -6.345283257703988156, 28.99440867395404453, 0.1037513055964221220 ) ) ;
#40631 = CARTESIAN_POINT ( 'NONE',  ( -6.640726327341849406E-14, 100.6774662015457409, -1.320564745697255449E-18 ) ) ;
#40632 = ORIENTED_EDGE ( 'NONE', *, *, #30320, .T. ) ;
#40633 = CARTESIAN_POINT ( 'NONE',  ( 11.88178580215906344, 154.9039014673913073, 2.222676336029907773 ) ) ;
#40634 = CARTESIAN_POINT ( 'NONE',  ( 1.400628584307200167E-15, 13.84300000000000352, 0.000000000000000000 ) ) ;
#40635 = EDGE_CURVE ( 'NONE', #25156, #41231, #37738, .T. ) ;
#40636 = CARTESIAN_POINT ( 'NONE',  ( -0.3686011943524581391, 118.1627388489639827, -0.9054303920307451570 ) ) ;
#40637 = CIRCLE ( 'NONE', #28375, 0.2539999999999980052 ) ;
#40638 = CARTESIAN_POINT ( 'NONE',  ( -1.559908931542489885, 116.9323294830472122, 1.291681667928520794 ) ) ;
#40639 = CARTESIAN_POINT ( 'NONE',  ( 0.7792876995799051798, 11.14506788600763443, 8.385000233822015758 ) ) ;
#40640 = CARTESIAN_POINT ( 'NONE',  ( -0.01341678693510457362, 156.4123495908283985, 0.6714308817992611367 ) ) ;
#40641 = CARTESIAN_POINT ( 'NONE',  ( -4.727076074248890869, 118.5930653697794384, -1.020453353391729712 ) ) ;
#40642 = CARTESIAN_POINT ( 'NONE',  ( 23.05883864707322672, 142.5499849734818838, -0.2756568390806648505 ) ) ;
#40643 = LINE ( 'NONE', #4032, #36962 ) ;
#40644 = CARTESIAN_POINT ( 'NONE',  ( -57.80874022462288764, 0.9184563934575655786, 1.089676212215488826 ) ) ;
#40645 = CARTESIAN_POINT ( 'NONE',  ( -50.22374042606539035, 15.93784852756063586, 4.876865049933926777 ) ) ;
#40646 = EDGE_CURVE ( 'NONE', #25936, #35053, #41285, .T. ) ;
#40647 = DIRECTION ( 'NONE',  ( 0.01997839162482749689, 1.040247600000945640E-18, -0.9998004120163610509 ) ) ;
#40648 = CARTESIAN_POINT ( 'NONE',  ( -4.245060323073253983, 118.2245461714415882, 0.3158324249594203215 ) ) ;
#40649 = CARTESIAN_POINT ( 'NONE',  ( 3.009276887026298031, 39.20946620154573736, -1.210121013456480599 ) ) ;
#40650 = AXIS2_PLACEMENT_3D ( 'NONE', #2636, #27553, #14754 ) ;
#40651 = ORIENTED_EDGE ( 'NONE', *, *, #11284, .T. ) ;
#40652 = CARTESIAN_POINT ( 'NONE',  ( -49.93490050754573417, 16.96705409125581099, 5.170188367178237598 ) ) ;
#40653 = CARTESIAN_POINT ( 'NONE',  ( 4.064929033868455832, 119.1709280882609647, -0.7633918317421104494 ) ) ;
#40654 = CARTESIAN_POINT ( 'NONE',  ( -6.733859895264124873, 121.2177056076135528, -0.3428974583126987996 ) ) ;
#40655 = CARTESIAN_POINT ( 'NONE',  ( 4.384565885174443345, 118.1629857386982252, 0.6642191121717796465 ) ) ;
#40656 = CARTESIAN_POINT ( 'NONE',  ( -0.6075365842366953206, 120.7136710450757988, -0.2388278564565361750 ) ) ;
#40657 = CARTESIAN_POINT ( 'NONE',  ( -12.69999999999999574, 17.14499999999999957, 0.000000000000000000 ) ) ;
#40658 = CARTESIAN_POINT ( 'NONE',  ( 0.1174553389596492831, 118.1651004037305057, -0.8901345560001526769 ) ) ;
#40659 = ORIENTED_EDGE ( 'NONE', *, *, #4058, .F. ) ;
#40660 = CARTESIAN_POINT ( 'NONE',  ( 3.935102970030661673, 16.48578375386999539, 2.424025302511324309 ) ) ;
#40661 = CARTESIAN_POINT ( 'NONE',  ( -16.15947664645545245, 148.3349945484709451, -1.756847814979443534 ) ) ;
#40662 = B_SPLINE_CURVE_WITH_KNOTS ( 'NONE', 3,
 ( #6928, #41879, #2899, #38464 ),
 .UNSPECIFIED., .F., .F.,
 ( 4, 4 ),
 ( 0.000000000000000000, 0.5094958736258470289 ),
 .UNSPECIFIED. ) ;
#40663 = DIRECTION ( 'NONE',  ( -0.8745520943968243532, 0.4849315768086547296, -6.829619984160642269E-16 ) ) ;
#40664 = CARTESIAN_POINT ( 'NONE',  ( -45.67969256299868164, 21.13156854447563759, 4.214927840906447010 ) ) ;
#40665 = CARTESIAN_POINT ( 'NONE',  ( -47.90759336580052263, 19.42461454689798117, 5.304755467655303036 ) ) ;
#40666 = CARTESIAN_POINT ( 'NONE',  ( 7.787415783305453587, 122.6040299132955766, 0.2655587982165120153 ) ) ;
#40667 = CARTESIAN_POINT ( 'NONE',  ( -19.97113776634630256, 79.44829951959813741, -1.524000000000003574 ) ) ;
#40668 = CARTESIAN_POINT ( 'NONE',  ( 22.65971377182555457, 149.0844379882532849, 1.633711759839209465 ) ) ;
#40669 = CARTESIAN_POINT ( 'NONE',  ( 5.965356522962860453, 53.58606249999999704, -5.016499999999999737 ) ) ;
#40671 = CARTESIAN_POINT ( 'NONE',  ( 13.92608219098127442, 121.7708260186165177, -1.076920499313079649 ) ) ;
#40670 = CARTESIAN_POINT ( 'NONE',  ( 3.198224922426783579, -14.19254063666773291, 2.189163805996276579 ) ) ;
#40672 = CARTESIAN_POINT ( 'NONE',  ( -14.49813937024316779, 152.7616507467334372, 1.711219460879524146 ) ) ;
#40673 = CARTESIAN_POINT ( 'NONE',  ( -4.596079559025361583, 18.26954911218466648, 0.4757704999388879807 ) ) ;
#40674 = CARTESIAN_POINT ( 'NONE',  ( -7.852582050918316625, 158.6543443936584481, -0.7853876145049528690 ) ) ;
#40675 = VECTOR ( 'NONE', #18168, 1000.000000000000227 ) ;
#40676 = CARTESIAN_POINT ( 'NONE',  ( 0.6142125404598580696, 23.44653936994281906, -0.7587870835084352672 ) ) ;
#40677 = ORIENTED_EDGE ( 'NONE', *, *, #4603, .F. ) ;
#40678 = CARTESIAN_POINT ( 'NONE',  ( -47.83226487260633775, 16.75079348177631999, 1.615774049669061574 ) ) ;
#40679 = CARTESIAN_POINT ( 'NONE',  ( -10.74829939017208424, 126.1521286088116369, 0.3663887985317103024 ) ) ;
#40680 = CARTESIAN_POINT ( 'NONE',  ( 4.362034286260056071, -13.41731938665795276, 3.520857194803681534 ) ) ;
#40681 = CARTESIAN_POINT ( 'NONE',  ( 16.92314199871282909, 144.1809451582817587, -1.383154804529856730 ) ) ;
#40682 = ORIENTED_EDGE ( 'NONE', *, *, #18885, .T. ) ;
#40683 = CARTESIAN_POINT ( 'NONE',  ( 3.087900938566228604, 115.7029548885307690, 1.663163182406099949 ) ) ;
#40684 = EDGE_LOOP ( 'NONE', ( #24698, #33167, #12225, #29696 ) ) ;
#40685 = CARTESIAN_POINT ( 'NONE',  ( 3.001448597307602828, -14.49079452896849496, 4.301892286087903194 ) ) ;
#40686 = CARTESIAN_POINT ( 'NONE',  ( -4.869070970386411012, 117.7192101133515081, -0.9437256607972734912 ) ) ;
#40687 = EDGE_CURVE ( 'NONE', #32704, #35171, #7314, .T. ) ;
#40688 = CARTESIAN_POINT ( 'NONE',  ( 13.59948517815232982, 150.2262467139961473, 0.1464537565166199873 ) ) ;
#40689 = ORIENTED_EDGE ( 'NONE', *, *, #4501, .T. ) ;
#40690 = CARTESIAN_POINT ( 'NONE',  ( 19.08488522674161558, 150.4642993720107143, 2.434974558521498356 ) ) ;
#40691 = CARTESIAN_POINT ( 'NONE',  ( 14.24929227862422465, 61.25037559889041461, -5.016500000000000625 ) ) ;
#40692 = CARTESIAN_POINT ( 'NONE',  ( -5.351939987885121930, 28.02203698121795128, 0.4484657473410642026 ) ) ;
#40693 = CARTESIAN_POINT ( 'NONE',  ( -23.75997692595333177, 82.67351089148900201, -1.524000000000006239 ) ) ;
#40694 = CARTESIAN_POINT ( 'NONE',  ( 3.754954749907335465, 116.6824454826851820, -0.08209545411912760882 ) ) ;
#40695 = DIRECTION ( 'NONE',  ( -0.8745520943968235761, 0.4849315768086558398, -4.268512490100410909E-16 ) ) ;
#40696 = AXIS2_PLACEMENT_3D ( 'NONE', #6000, #22771, #29617 ) ;
#40697 = CARTESIAN_POINT ( 'NONE',  ( 1.943636354525413168, -15.05866079806446400, 5.749033333573775550 ) ) ;
#40698 = CARTESIAN_POINT ( 'NONE',  ( 10.45722248778855246, 56.52709681235302241, 5.016500000000865711 ) ) ;
#40699 = CARTESIAN_POINT ( 'NONE',  ( -4.999442924991678083, 117.3993846698902672, -0.8265828626092326381 ) ) ;
#40700 = CARTESIAN_POINT ( 'NONE',  ( -4.675172209724520300, 117.9626846738122623, 0.7309470385922346436 ) ) ;
#40701 = ORIENTED_EDGE ( 'NONE', *, *, #19654, .F. ) ;
#40702 = CARTESIAN_POINT ( 'NONE',  ( 19.68500000000000227, 71.11999999999999034, -1.904999999999999583 ) ) ;
#40703 = CARTESIAN_POINT ( 'NONE',  ( -8.451782431670267215, 119.2584666972338283, -1.350551005905172408 ) ) ;
#40704 = CARTESIAN_POINT ( 'NONE',  ( 0.1065646865915094443, 105.8844662015457061, -5.332932678536314697 ) ) ;
#40705 = CARTESIAN_POINT ( 'NONE',  ( 4.902823790339319032, 117.6536153060737320, 0.9411696025594519233 ) ) ;
#40706 = CARTESIAN_POINT ( 'NONE',  ( -11.47253659098481293, 56.76836532675864788, -5.016499999999999737 ) ) ;
#40707 = CARTESIAN_POINT ( 'NONE',  ( -0.3785707606483163512, 120.7331730230137623, 0.5164240810526173897 ) ) ;
#40708 = CARTESIAN_POINT ( 'NONE',  ( -2.136650056307613621, 10.86338872207680950, -4.114640003288728920 ) ) ;
#40709 = DIRECTION ( 'NONE',  ( 6.353134868986659519E-16, -1.000000000000000000, -0.000000000000000000 ) ) ;
#40710 = CARTESIAN_POINT ( 'NONE',  ( -5.158148607181098022, 114.7154334724729097, -1.455730150661056044 ) ) ;
#40711 = CARTESIAN_POINT ( 'NONE',  ( 2.626143189074743756, -14.75305764222682647, 4.894789397842846945 ) ) ;
#40712 = CARTESIAN_POINT ( 'NONE',  ( 4.812498123319315368, 116.8297769931967309, -0.8564213435964298515 ) ) ;
#40713 = ADVANCED_FACE ( 'NONE', ( #20105 ), #14074, .T. ) ;
#40714 = CARTESIAN_POINT ( 'NONE',  ( -5.034401795890290465, 27.85181560600499395, 0.5116811242461191123 ) ) ;
#40715 = B_SPLINE_CURVE_WITH_KNOTS ( 'NONE', 5,
 ( #15851, #17067, #36470, #6863, #28645, #26874 ),
 .UNSPECIFIED., .F., .F.,
 ( 6, 6 ),
 ( 0.7824693819017078944, 1.000000000000000000 ),
 .UNSPECIFIED. ) ;
#40716 = CARTESIAN_POINT ( 'NONE',  ( -0.2391844021489926142, 115.7030485465296579, 1.756103904555268214 ) ) ;
#40717 = CARTESIAN_POINT ( 'NONE',  ( -4.460028654926622593, 22.53297844546955631, 1.214995109042491528 ) ) ;
#40718 = VERTEX_POINT ( 'NONE', #759 ) ;
#40719 = CARTESIAN_POINT ( 'NONE',  ( -3.857417139088993530, 104.6144662015498881, -3.700432031744215866 ) ) ;
#40720 = CARTESIAN_POINT ( 'NONE',  ( 1.896617635523351053, -15.61750365820154052, 5.464805439086081407 ) ) ;
#40721 = CARTESIAN_POINT ( 'NONE',  ( -11.29660330931812240, 121.3367100885591015, 1.243740200939189133 ) ) ;
#40722 = CARTESIAN_POINT ( 'NONE',  ( 0.3817720443006957232, 19.93710050853265869, -0.8978640518339636722 ) ) ;
#40723 = EDGE_LOOP ( 'NONE', ( #37763, #29975, #14269, #41352 ) ) ;
#40724 = ORIENTED_EDGE ( 'NONE', *, *, #33879, .F. ) ;
#40725 = CARTESIAN_POINT ( 'NONE',  ( -17.14500000000466784, 71.11999999999886768, -1.524000000000000909 ) ) ;
#40726 = CARTESIAN_POINT ( 'NONE',  ( 3.894863181655531026, 121.5791280715047122, 0.3237234463424497610 ) ) ;
#40727 = CARTESIAN_POINT ( 'NONE',  ( -4.430366727502396351, 120.6578283891288379, 0.4452475156743749274 ) ) ;
#40728 = EDGE_CURVE ( 'NONE', #21382, #37685, #16897, .T. ) ;
#40729 = CARTESIAN_POINT ( 'NONE',  ( 4.605784392446712339, 118.0409339601070684, -0.6501282048334815489 ) ) ;
#40730 = CARTESIAN_POINT ( 'NONE',  ( 6.628409759326957307, 120.2999964176511014, -0.9194780514890085188 ) ) ;
#40731 = CARTESIAN_POINT ( 'NONE',  ( -20.38365538121576037, 147.8414448467482600, -2.482674703111230841 ) ) ;
#40732 = CARTESIAN_POINT ( 'NONE',  ( -17.14500000000466784, 71.11999999999886768, 1.269999999999998241 ) ) ;
#40733 = CARTESIAN_POINT ( 'NONE',  ( 4.385175369536176149, 118.1846130434793736, -0.4263825146163124358 ) ) ;
#40734 = CARTESIAN_POINT ( 'NONE',  ( 0.6772589037150074098, 156.3292479207028407, -0.3306685775513073522 ) ) ;
#40735 = ORIENTED_EDGE ( 'NONE', *, *, #27165, .F. ) ;
#40736 = CARTESIAN_POINT ( 'NONE',  ( 1.852819980464847305, -15.24972552306870455, 5.408883774200016425 ) ) ;
#40737 = EDGE_CURVE ( 'NONE', #38115, #20977, #29411, .T. ) ;
#40738 = VECTOR ( 'NONE', #38857, 1000.000000000000000 ) ;
#40739 = VECTOR ( 'NONE', #3239, 1000.000000000000114 ) ;
#40740 = CARTESIAN_POINT ( 'NONE',  ( -12.21488373879589240, 55.24499999999999034, 5.016499999999999737 ) ) ;
#40741 = ADVANCED_FACE ( 'NONE', ( #7148 ), #12042, .F. ) ;
#40742 = CARTESIAN_POINT ( 'NONE',  ( -58.43492521371286585, -0.3997831091909794798, 0.3282367010159537579 ) ) ;
#40743 = CARTESIAN_POINT ( 'NONE',  ( -4.120466288800530563, -1.808681497221679590, -2.133573495687988597 ) ) ;
#40744 = CARTESIAN_POINT ( 'NONE',  ( 16.71293428529030578, 146.3384789841921361, 1.780605135160314489 ) ) ;
#40745 = CARTESIAN_POINT ( 'NONE',  ( -3.151460842193158474, 28.87231940813492770, 1.610289367860948229 ) ) ;
#40746 = CARTESIAN_POINT ( 'NONE',  ( -2.741226102065176029, 109.4146836159258669, 3.767795064178312892 ) ) ;
#40747 = CARTESIAN_POINT ( 'NONE',  ( -4.288638401707804526, -7.253218809911426312, -1.756103832032595680 ) ) ;
#40748 = CARTESIAN_POINT ( 'NONE',  ( 7.557080711912756321, 122.4263405438208991, 0.1815966937148654481 ) ) ;
#40749 = EDGE_CURVE ( 'NONE', #14480, #1690, #33129, .T. ) ;
#40750 = CARTESIAN_POINT ( 'NONE',  ( -2.668541714186689617, -2.899408749949365038, -8.001679540268986202 ) ) ;
#40751 = CARTESIAN_POINT ( 'NONE',  ( -57.60038635073814817, 1.097546858218806376, -1.033898108845213542E-14 ) ) ;
#40752 = CARTESIAN_POINT ( 'NONE',  ( 2.154724539067322642, 116.5279165083215531, -0.3115280795628784238 ) ) ;
#40753 = CARTESIAN_POINT ( 'NONE',  ( -29.48103325898055971, 60.42855201934086296, -1.270000000000005347 ) ) ;
#40754 = CARTESIAN_POINT ( 'NONE',  ( 3.682264917456191888, 101.1854662015457365, 0.07358041635423968885 ) ) ;
#40755 = CARTESIAN_POINT ( 'NONE',  ( -5.586884702347495235, 68.92746620154572668, -0.1116392523995361763 ) ) ;
#40756 = CARTESIAN_POINT ( 'NONE',  ( -23.24761240069422286, 77.83567810938664877, 1.269999999999994023 ) ) ;
#40757 = CARTESIAN_POINT ( 'NONE',  ( -1.112825283668275045, 5.041181605477844663, 8.348645504544187190 ) ) ;
#40758 = CARTESIAN_POINT ( 'NONE',  ( -0.01811622957310190032, 118.1588881536610529, 0.9066104818223087447 ) ) ;
#40759 = DIRECTION ( 'NONE',  ( 0.8138664877804109299, -0.5810519254489895369, 0.000000000000000000 ) ) ;
#40760 = CARTESIAN_POINT ( 'NONE',  ( 2.233078627056604759, -15.14192004606506536, 5.083345892419886880 ) ) ;
#40761 = CARTESIAN_POINT ( 'NONE',  ( 0.4232488410868608941, 124.9344662015457317, 0.008457519121177021690 ) ) ;
#40762 = CARTESIAN_POINT ( 'NONE',  ( -5.670663496354099387, 159.1134716836843381, 0.2862304005612826274 ) ) ;
#40763 = VERTEX_POINT ( 'NONE', #7561 ) ;
#40764 = CARTESIAN_POINT ( 'NONE',  ( -58.43523997267251247, 0.9435442997105664142, -0.5849561510202232473 ) ) ;
#40765 = AXIS2_PLACEMENT_3D ( 'NONE', #37808, #15222, #17783 ) ;
#40766 = EDGE_LOOP ( 'NONE', ( #14342, #15186, #28435, #11451 ) ) ;
#40767 = CARTESIAN_POINT ( 'NONE',  ( -44.28332145682448839, 21.53821517059177637, -3.041508016573486461 ) ) ;
#40768 = CARTESIAN_POINT ( 'NONE',  ( -11.03183784343237583, 128.0124916018596650, -0.2204423744267034746 ) ) ;
#40769 = CARTESIAN_POINT ( 'NONE',  ( 5.769960013412655186, -14.74427453315851899, 2.495425615322755419 ) ) ;
#40770 = CARTESIAN_POINT ( 'NONE',  ( -11.79681931163876385, 156.4111399680655552, 1.533406117021610449 ) ) ;
#40771 = CARTESIAN_POINT ( 'NONE',  ( 3.922549711534259576, 117.3164332630744298, -0.5226386447273274616 ) ) ;
#40772 = CARTESIAN_POINT ( 'NONE',  ( 2.488009491785908800, 18.85968022696138391, -3.895047602898422223 ) ) ;
#40773 = CARTESIAN_POINT ( 'NONE',  ( -11.56079167746340097, 118.7825156662901378, -0.6096482884850569217 ) ) ;
#40774 = ADVANCED_FACE ( 'NONE', ( #16497 ), #36117, .T. ) ;
#40775 = CARTESIAN_POINT ( 'NONE',  ( -49.52772409537172393, 17.03862487098385969, -5.022027238426779228 ) ) ;
#40776 = ORIENTED_EDGE ( 'NONE', *, *, #41501, .F. ) ;
#40777 = CARTESIAN_POINT ( 'NONE',  ( 5.558084639757285395, 116.7153428098866641, 0.2417474866754134033 ) ) ;
#40778 = CARTESIAN_POINT ( 'NONE',  ( 6.059261036834405978, 56.51500000000000057, 5.016500000000001513 ) ) ;
#40779 = CARTESIAN_POINT ( 'NONE',  ( -17.71558884668074896, 147.6919162452172145, 1.529690151225475692 ) ) ;
#40780 = CARTESIAN_POINT ( 'NONE',  ( -53.26002898140129105, 10.27656598764010809, -3.765953445939742572 ) ) ;
#40781 = CARTESIAN_POINT ( 'NONE',  ( 19.07204494652734184, 148.5750135429820205, -1.735237764431467822 ) ) ;
#40782 = CARTESIAN_POINT ( 'NONE',  ( -13.88956208308366591, 122.0315337860429423, -1.683705570428295273 ) ) ;
#40783 = CARTESIAN_POINT ( 'NONE',  ( -53.00789483126595769, 12.40033530745290236, -4.180047681284821515 ) ) ;
#40784 = CARTESIAN_POINT ( 'NONE',  ( 15.79191249938946839, 148.1776054874778197, -0.7900072561285058637 ) ) ;
#40785 = VERTEX_POINT ( 'NONE', #29503 ) ;
#40786 = CARTESIAN_POINT ( 'NONE',  ( -2.153957835384924469, 157.2504501563031738, -1.632675037709188315 ) ) ;
#40787 = CARTESIAN_POINT ( 'NONE',  ( 4.539898764682361865, -15.38453816280940778, 0.3562021009913567959 ) ) ;
#40788 = CARTESIAN_POINT ( 'NONE',  ( -4.528373626541791985, 118.0896223068915276, -0.7655945527491994085 ) ) ;
#40789 = EDGE_CURVE ( 'NONE', #26194, #35651, #969, .T. ) ;
#40790 = CARTESIAN_POINT ( 'NONE',  ( -57.26626398570029863, 3.526386058942967860, -2.205039086913768820 ) ) ;
#40791 = DIRECTION ( 'NONE',  ( -1.000000000000000000, -6.353134868986659519E-16, -0.000000000000000000 ) ) ;
#40792 = CARTESIAN_POINT ( 'NONE',  ( 1.354060893033489643, 119.5584937100158243, 0.6194060083641332870 ) ) ;
#40793 = DIRECTION ( 'NONE',  ( -0.3256999990547876367, -0.9454731675810326141, -8.328397965208553695E-18 ) ) ;
#40794 = TOROIDAL_SURFACE ( 'NONE', #17628, 0.3809999999999990616, 0.2540000000000000036 ) ;
#40795 = CARTESIAN_POINT ( 'NONE',  ( -7.401523468229766145, -5.981721843848114339, 4.095665678060115944 ) ) ;
#40796 = CARTESIAN_POINT ( 'NONE',  ( 4.329655997251290245, 155.8404949922767742, 0.5159277680907120578 ) ) ;
#40797 = CARTESIAN_POINT ( 'NONE',  ( -56.21344593158320180, 5.939860726778031896, -2.828251681716873911 ) ) ;
#40799 = EDGE_LOOP ( 'NONE', ( #1847, #9839, #1792, #11313 ) ) ;
#40798 = CARTESIAN_POINT ( 'NONE',  ( -42.04356058215219605, 22.06167541775167606, -0.4953331422234020232 ) ) ;
#40800 = CARTESIAN_POINT ( 'NONE',  ( 3.837460294590816279, 108.9298176806530165, -3.710659438875620886 ) ) ;
#40801 = DIRECTION ( 'NONE',  ( 0.6294287539884032556, 0.7770581983690836303, 1.945484789722780312E-16 ) ) ;
#40802 = CARTESIAN_POINT ( 'NONE',  ( -58.31320831016853390, -0.1895118959954616988, 0.07592354283881128096 ) ) ;
#40803 = CARTESIAN_POINT ( 'NONE',  ( -52.80069327121181288, 17.37962920081948681, 0.7126778406583705872 ) ) ;
#40804 = CARTESIAN_POINT ( 'NONE',  ( -16.19138771801004495, 121.3864332154274877, -0.1624333549846387614 ) ) ;
#40805 = ORIENTED_EDGE ( 'NONE', *, *, #16999, .F. ) ;
#40806 = CARTESIAN_POINT ( 'NONE',  ( -49.18322560636019602, 21.37428572888716616, -2.217132718382757606 ) ) ;
#40807 = CARTESIAN_POINT ( 'NONE',  ( -5.910993448784967796, 121.3707704662934219, -0.3328318058967496551 ) ) ;
#40808 = PLANE ( 'NONE',  #40765 ) ;
#40809 = ORIENTED_EDGE ( 'NONE', *, *, #38613, .F. ) ;
#40810 = CARTESIAN_POINT ( 'NONE',  ( 0.7079803121674352884, 118.7629491485454025, -1.246627914299262896 ) ) ;
#40811 = CARTESIAN_POINT ( 'NONE',  ( -10.39558336183872989, 126.0814211662656419, -0.4651924986760611058 ) ) ;
#40812 = CARTESIAN_POINT ( 'NONE',  ( 2.652408316642993480, -15.27006336626107696, 5.836003982494253783 ) ) ;
#40813 = CARTESIAN_POINT ( 'NONE',  ( -3.977532531966777807, 117.6225627337916393, 0.6337845664926936573 ) ) ;
#40814 = CARTESIAN_POINT ( 'NONE',  ( 0.2297947187657226054, 117.3993836757579317, -1.488868525946095422 ) ) ;
#40815 = CARTESIAN_POINT ( 'NONE',  ( 16.18495160125058874, 121.3864332154274877, 0.4845229560194669327 ) ) ;
#40816 = CARTESIAN_POINT ( 'NONE',  ( 8.946522384465550815, 123.9641338091273894, 0.2230221356586828685 ) ) ;
#40817 = CARTESIAN_POINT ( 'NONE',  ( -5.924740142096584172, 65.21691166894066782, -1.269999999999994023 ) ) ;
#40818 = CARTESIAN_POINT ( 'NONE',  ( -0.2773724154211913984, 24.90860930217742464, 0.9350043038818249830 ) ) ;
#40819 = CARTESIAN_POINT ( 'NONE',  ( -11.70340384973345849, 118.7242475115495495, -0.3301557443347882259 ) ) ;
#40820 = DIRECTION ( 'NONE',  ( 0.1951894777626526079, 0.9807655518882905099, -6.538892540527681903E-17 ) ) ;
#40821 = CIRCLE ( 'NONE', #38743, 0.6350000000000001199 ) ;
#40822 = ORIENTED_EDGE ( 'NONE', *, *, #34765, .T. ) ;
#40823 = CARTESIAN_POINT ( 'NONE',  ( -5.348924234571052594, 56.51499999999999346, -4.492130288940743732 ) ) ;
#40824 = ORIENTED_EDGE ( 'NONE', *, *, #6916, .F. ) ;
#40825 = CARTESIAN_POINT ( 'NONE',  ( -8.365703719145541228, 119.9183728994499916, 1.113763724379078557 ) ) ;
#40826 = CARTESIAN_POINT ( 'NONE',  ( 1.173990663012069113, -13.46572784750561880, -4.469126434461346165 ) ) ;
#40827 = CARTESIAN_POINT ( 'NONE',  ( 21.45663756426498381, 150.2128557559047692, 2.007674378541679072 ) ) ;
#40828 = CARTESIAN_POINT ( 'NONE',  ( -58.30061145522432042, -0.1075020354497826652, -0.6732717543608098820 ) ) ;
#40829 = CARTESIAN_POINT ( 'NONE',  ( 8.970048054448124475, 157.0267672960688969, -1.675204009492540447 ) ) ;
#40830 = CARTESIAN_POINT ( 'NONE',  ( 0.04286443493920111952, 25.39157861068392208, -8.424000189867014043 ) ) ;
#40831 = CARTESIAN_POINT ( 'NONE',  ( -16.14352587498456160, 122.8183540351560907, -1.297681478882586115 ) ) ;
#40832 = CARTESIAN_POINT ( 'NONE',  ( 4.757004511144192094, 117.7257274568053873, -0.9115379262560657780 ) ) ;
#40833 = EDGE_LOOP ( 'NONE', ( #30791, #7937, #16950, #16124 ) ) ;
#40834 = CARTESIAN_POINT ( 'NONE',  ( -15.81463230642823170, 145.9351319680867221, 0.01551611691150908343 ) ) ;
#40835 = CARTESIAN_POINT ( 'NONE',  ( -0.4661379286531509014, 118.8635629087341954, -0.6143748731645414241 ) ) ;
#40836 = CARTESIAN_POINT ( 'NONE',  ( 4.192023472006414231, -15.34368243816432198, 4.862536176465709126 ) ) ;
#40837 = DIRECTION ( 'NONE',  ( -5.188838149069471174E-16, 1.699382548006136313E-16, 1.000000000000000000 ) ) ;
#40838 = CARTESIAN_POINT ( 'NONE',  ( -2.751821739654949805, 117.9496046090067125, -1.327625076587163111 ) ) ;
#40839 = ORIENTED_EDGE ( 'NONE', *, *, #24307, .T. ) ;
#40840 = B_SPLINE_SURFACE_WITH_KNOTS ( 'NONE', 3, 1, ( 
 ( #36182, #7002 ),
 ( #3815, #16778 ),
 ( #29782, #13590 ),
 ( #26579, #39587 ) ),
 .UNSPECIFIED., .F., .F., .F.,
 ( 4, 4 ),
 ( 2, 2 ),
 ( 0.000000000000000000, 0.6118630412642116490 ),
 ( 0.000000000000000000, 1.000000000000000000 ),
 .UNSPECIFIED. ) ;
#40841 = CARTESIAN_POINT ( 'NONE',  ( 1.279006062069942384, 119.0230276286704054, 0.6822954352362461394 ) ) ;
#40842 = DIRECTION ( 'NONE',  ( 0.8745520943968235761, -0.4849315768086558398, 0.000000000000000000 ) ) ;
#40843 = VECTOR ( 'NONE', #37787, 1000.000000000000000 ) ;
#40844 = CARTESIAN_POINT ( 'NONE',  ( -5.239701418611195649, 115.6909491485453003, -1.023982712389427840 ) ) ;
#40845 = CARTESIAN_POINT ( 'NONE',  ( -2.908797093395109723, 122.3314979878274045, 0.1372540494999659189 ) ) ;
#40846 = CARTESIAN_POINT ( 'NONE',  ( -2.668541714186689617, -2.899408749949365038, -8.001679540268986202 ) ) ;
#40847 = CARTESIAN_POINT ( 'NONE',  ( 16.13275712328120548, 147.4171829256358137, 1.433441054525536273 ) ) ;
#40848 = CARTESIAN_POINT ( 'NONE',  ( -45.67973391888839529, 25.66060799623228661, -1.524000000000008237 ) ) ;
#40849 = CARTESIAN_POINT ( 'NONE',  ( 22.91546036685015153, 149.1739538623130272, -0.5130544771887697308 ) ) ;
#40850 = DIRECTION ( 'NONE',  ( -0.1469470846586743984, -9.335746474409589170E-17, -0.9891443546370349837 ) ) ;
#40851 = CARTESIAN_POINT ( 'NONE',  ( -58.36906557521628258, -0.2900353211930308817, 0.03225343758777150793 ) ) ;
#40852 = CARTESIAN_POINT ( 'NONE',  ( -4.528182882554109945, 31.49130102246704155, -0.6941393877658236233 ) ) ;
#40853 = CARTESIAN_POINT ( 'NONE',  ( 1.897380780832737202, -15.05783359004130517, 5.662421594695138616 ) ) ;
#40854 = CARTESIAN_POINT ( 'NONE',  ( -4.282516613351655010, 118.2128436458740168, 0.3623403077545777617 ) ) ;
#40855 = DIRECTION ( 'NONE',  ( 0.1728608224830406603, -0.000000000000000000, -0.9849462604886047856 ) ) ;
#40856 = ORIENTED_EDGE ( 'NONE', *, *, #29039, .T. ) ;
#40857 = CARTESIAN_POINT ( 'NONE',  ( -48.08949201794742834, 19.91830422262442468, 5.194343260851632671 ) ) ;
#40858 =( BOUNDED_CURVE ( )  B_SPLINE_CURVE ( 3, ( #24335, #24757, #31579, #2205 ),
 .UNSPECIFIED., .F., .T. ) 
 B_SPLINE_CURVE_WITH_KNOTS ( ( 4, 4 ),
 ( 0.000000000000000000, 1.570796326794895670 ),
 .UNSPECIFIED. ) 
 CURVE ( )  GEOMETRIC_REPRESENTATION_ITEM ( )  RATIONAL_B_SPLINE_CURVE ( ( 1.000000000000000000, 0.8047378541243652705, 0.8047378541243652705, 1.000000000000000000 ) ) 
 REPRESENTATION_ITEM ( '' )  );
#40859 = CARTESIAN_POINT ( 'NONE',  ( -4.024596240589787044, 119.1709112288356494, -0.9240400258402845513 ) ) ;
#40860 = CARTESIAN_POINT ( 'NONE',  ( -5.332935397695336199, 116.0444662015457311, -0.1065647409268299234 ) ) ;
#40861 = CARTESIAN_POINT ( 'NONE',  ( 4.394896113366216994, 118.1799268271195160, 0.5694229943158597429 ) ) ;
#40862 = CARTESIAN_POINT ( 'NONE',  ( -16.02106284285062898, 145.8417561620165372, -1.176135107295964932 ) ) ;
#40863 = DIRECTION ( 'NONE',  ( 1.000000000000000000, 0.000000000000000000, -1.224646799147351728E-16 ) ) ;
#40864 = AXIS2_PLACEMENT_3D ( 'NONE', #21150, #34180, #24563 ) ;
#40865 = CARTESIAN_POINT ( 'NONE',  ( 0.8838529761740171464, 116.4325158421065680, 0.01766148591713737059 ) ) ;
#40866 = ORIENTED_EDGE ( 'NONE', *, *, #15701, .T. ) ;
#40867 = CARTESIAN_POINT ( 'NONE',  ( -4.631227783250409402, 22.10816835407601744, -0.05711764529929251599 ) ) ;
#40868 = CARTESIAN_POINT ( 'NONE',  ( -6.788801044988821864, 155.5980657034081105, -1.487835262196283814 ) ) ;
#40869 = CARTESIAN_POINT ( 'NONE',  ( 12.21488373879589240, 71.11999999999999034, -4.381499999999999950 ) ) ;
#40870 = CARTESIAN_POINT ( 'NONE',  ( -41.60680704299971922, 22.55277366187537780, 1.574601807764032468 ) ) ;
#40871 = CARTESIAN_POINT ( 'NONE',  ( -19.33375693323417011, 80.42273151551299293, -1.270000000000003570 ) ) ;
#40872 = CARTESIAN_POINT ( 'NONE',  ( 6.991496846172011281, 121.9383932547358427, 0.2731297716818573140 ) ) ;
#40873 = CARTESIAN_POINT ( 'NONE',  ( -4.621022795674669226, 27.76579825817536218, 0.1735962381356405959 ) ) ;
#40874 = CARTESIAN_POINT ( 'NONE',  ( 22.49588706318638387, 149.6594668941642681, 1.627141970658571912 ) ) ;
#40875 = DIRECTION ( 'NONE',  ( -0.4849315768086495115, -0.8745520943968271288, -7.999751396575051143E-15 ) ) ;
#40877 = CARTESIAN_POINT ( 'NONE',  ( 20.03018601867063708, 150.7967616730061593, -1.468133569223299739 ) ) ;
#40876 = CARTESIAN_POINT ( 'NONE',  ( 2.857130780617909149, -14.87311083204414786, 4.269097905712053276 ) ) ;
#40878 = AXIS2_PLACEMENT_3D ( 'NONE', #12797, #42001, #36025 ) ;
#40879 = CARTESIAN_POINT ( 'NONE',  ( -5.764372972839621134, 156.8407539676644546, 1.669942767410474094 ) ) ;
#40880 = CARTESIAN_POINT ( 'NONE',  ( -4.583145339711863109, 27.87760190725156662, 0.5120832130453706332 ) ) ;
#40881 = CARTESIAN_POINT ( 'NONE',  ( -22.80460045200421959, 149.7823008822066697, -1.306974408439632196 ) ) ;
#40882 = CARTESIAN_POINT ( 'NONE',  ( 0.6656887758738300187, 13.74536131906779879, -0.7131539583378491143 ) ) ;
#40883 = VERTEX_POINT ( 'NONE', #343 ) ;
#40884 = CARTESIAN_POINT ( 'NONE',  ( -56.42856387642236626, 3.193865871111118082, 0.1553879740655848829 ) ) ;
#40885 = CARTESIAN_POINT ( 'NONE',  ( -7.108627447324336934, 121.8675249661327626, 0.3373703349335459567 ) ) ;
#40886 = CARTESIAN_POINT ( 'NONE',  ( 4.090168366125579880, -14.63905918998462141, 5.005671547667302157 ) ) ;
#40887 = CARTESIAN_POINT ( 'NONE',  ( 17.30282355392125027, 146.5563353440282981, -1.366477706345457843 ) ) ;
#40888 = VERTEX_POINT ( 'NONE', #35908 ) ;
#40889 = CARTESIAN_POINT ( 'NONE',  ( 2.393094646133926862, 115.7029491485453434, 1.700721971483515560 ) ) ;
#40890 = CARTESIAN_POINT ( 'NONE',  ( 2.744913772555794385, -12.89811552070117884, 0.2544447123532062038 ) ) ;
#40891 = CARTESIAN_POINT ( 'NONE',  ( -4.717230826267398314, 117.7257772426691105, -1.100749342947852538 ) ) ;
#40892 = CARTESIAN_POINT ( 'NONE',  ( 15.53315888837586201, 147.5314071815517138, 0.1823436108899492425 ) ) ;
#40893 = ORIENTED_EDGE ( 'NONE', *, *, #29629, .T. ) ;
#40894 = CARTESIAN_POINT ( 'NONE',  ( 14.32444608545400300, 154.4775811199918110, 2.255247442408088165 ) ) ;
#40895 = CARTESIAN_POINT ( 'NONE',  ( -4.466782427718574588, 71.06098887363195615, 1.270000000000005791 ) ) ;
#40896 = AXIS2_PLACEMENT_3D ( 'NONE', #13264, #26037, #9852 ) ;
#40897 = CARTESIAN_POINT ( 'NONE',  ( 0.008148259816488066104, 159.5682499516715040, -0.4077722408685185429 ) ) ;
#40898 = CARTESIAN_POINT ( 'NONE',  ( 11.62351318166542669, 118.7506923092098674, -0.05658863777226865593 ) ) ;
#40899 = DIRECTION ( 'NONE',  ( 0.8745520943968235761, -0.4849315768086558398, 4.268512490100410909E-16 ) ) ;
#40900 = VECTOR ( 'NONE', #10233, 1000.000000000000000 ) ;
#40901 = CARTESIAN_POINT ( 'NONE',  ( 1.804633460655494570, -15.08373741368226817, 5.749549428864549228 ) ) ;
#40902 = CARTESIAN_POINT ( 'NONE',  ( -42.09814309847200064, 23.46876350539121248, 1.523999999999994026 ) ) ;
#40903 = DIRECTION ( 'NONE',  ( -6.146657985744592735E-16, 3.905054717696928257E-31, 1.000000000000000000 ) ) ;
#40904 = CARTESIAN_POINT ( 'NONE',  ( -4.809624879280043785, 117.8762316427875163, 0.6704367731218271453 ) ) ;
#40905 = ORIENTED_EDGE ( 'NONE', *, *, #39912, .T. ) ;
#40906 = ORIENTED_EDGE ( 'NONE', *, *, #5401, .F. ) ;
#40907 = FACE_OUTER_BOUND ( 'NONE', #38529, .T. ) ;
#40908 = CARTESIAN_POINT ( 'NONE',  ( 5.750380026109916720, 118.5999988179069362, -0.9867663322649924407 ) ) ;
#40909 = CARTESIAN_POINT ( 'NONE',  ( -2.972890788444433330, 110.6400929099055332, -3.409217096083849263 ) ) ;
#40910 = CARTESIAN_POINT ( 'NONE',  ( 4.959929520007769987, 117.4682222762912573, 0.9863292331654268663 ) ) ;
#40911 = DIRECTION ( 'NONE',  ( -4.017660918040594346E-17, 1.000000000000000000, 2.376309959284834438E-19 ) ) ;
#40912 = CARTESIAN_POINT ( 'NONE',  ( -0.3886773557329153972, 118.1497763966932695, 1.061209395727771732 ) ) ;
#40913 = CARTESIAN_POINT ( 'NONE',  ( 1.104432469574216480, -9.427232690354344413, -4.492858291722996888 ) ) ;
#40914 = DIRECTION ( 'NONE',  ( 5.188838149069472160E-16, -1.699382548006136559E-16, -1.000000000000000000 ) ) ;
#40915 = CARTESIAN_POINT ( 'NONE',  ( -6.550797450135577910E-14, 84.67546620154573134, 2.164564701558966795E-29 ) ) ;
#40916 = CARTESIAN_POINT ( 'NONE',  ( 3.507226199677831779, -13.17319675123219902, 2.199731216082013940 ) ) ;
#40917 = CARTESIAN_POINT ( 'NONE',  ( 5.114723271350645639, 118.2545999410811106, -0.5144770513779389765 ) ) ;
#40918 = CARTESIAN_POINT ( 'NONE',  ( -7.784012322544769269, 122.6313477034873074, -0.1555430911242075831 ) ) ;
#40919 = CARTESIAN_POINT ( 'NONE',  ( 1.400765281975942855, 35.96429942923645484, 2.374657561808434458 ) ) ;
#40920 = CARTESIAN_POINT ( 'NONE',  ( -0.5330231537557663657, 115.7033788390540963, 1.742913876867271838 ) ) ;
#40921 = CARTESIAN_POINT ( 'NONE',  ( -3.789191232057584902, 13.46218022696137773, 2.646434746401360893 ) ) ;
#40922 = ORIENTED_EDGE ( 'NONE', *, *, #9101, .T. ) ;
#40923 = CARTESIAN_POINT ( 'NONE',  ( 2.417140579268110656, 105.1243918821411825, -4.755895391891847623 ) ) ;
#40924 = CARTESIAN_POINT ( 'NONE',  ( 4.529877808639974468, -15.43662617131508163, 0.9000745948097405025 ) ) ;
#40925 = CARTESIAN_POINT ( 'NONE',  ( -19.34566907036586159, 149.3473233412102275, 1.724881794388704925 ) ) ;
#40926 = CARTESIAN_POINT ( 'NONE',  ( 0.7990752137124343957, 23.01725015362593396, -0.5559626729366093922 ) ) ;
#40927 = AXIS2_PLACEMENT_3D ( 'NONE', #12636, #25622, #22405 ) ;
#40928 = CARTESIAN_POINT ( 'NONE',  ( -0.9549105556349912760, 13.03813504644791976, -0.2014467441264284064 ) ) ;
#40929 = ORIENTED_EDGE ( 'NONE', *, *, #9182, .F. ) ;
#40930 = ORIENTED_EDGE ( 'NONE', *, *, #29088, .T. ) ;
#40931 = CARTESIAN_POINT ( 'NONE',  ( 14.73199999999999754, 12.96302561210691628, 1.804149664503880250E-15 ) ) ;
#40932 = CARTESIAN_POINT ( 'NONE',  ( 1.618304973946058878, 119.5945091202099348, 0.6420790694971424406 ) ) ;
#40933 = SURFACE_STYLE_USAGE ( .BOTH. , #1962 ) ;
#40934 = CARTESIAN_POINT ( 'NONE',  ( -16.60605961460005275, 147.5857818452174115, 1.108006280952565037 ) ) ;
#40935 = DIRECTION ( 'NONE',  ( -0.8745520943968235761, 0.4849315768086558398, -4.268512490100410909E-16 ) ) ;
#40936 = CARTESIAN_POINT ( 'NONE',  ( 3.383663933261424006, -14.10150345098371005, 4.318103191797684204 ) ) ;
#40937 = CARTESIAN_POINT ( 'NONE',  ( 9.808453647369967499, 155.3230018269108825, -1.667681936676747689 ) ) ;
#40938 = CIRCLE ( 'NONE', #25929, 5.588000000000006295 ) ;
#40939 = CARTESIAN_POINT ( 'NONE',  ( -19.42875987905505042, 141.0981142166620259, -2.503406319619450038 ) ) ;
#40940 = CARTESIAN_POINT ( 'NONE',  ( -36.43259636504752308, 28.15155085495446485, -1.270000000000003348 ) ) ;
#40941 = EDGE_CURVE ( 'NONE', #10310, #1232, #39247, .T. ) ;
#40942 = CARTESIAN_POINT ( 'NONE',  ( 4.074910602682932925, 118.2429491485453354, -0.1454311599470142491 ) ) ;
#40943 = CARTESIAN_POINT ( 'NONE',  ( 1.630522158633523011, 156.2764358050213787, -0.3353572448990092547 ) ) ;
#40944 = VERTEX_POINT ( 'NONE', #10112 ) ;
#40945 = CARTESIAN_POINT ( 'NONE',  ( 3.162130362391316840, -14.71481139081727640, 3.323541290955854599 ) ) ;
#40946 = VECTOR ( 'NONE', #29004, 1000.000000000000000 ) ;
#40947 = CARTESIAN_POINT ( 'NONE',  ( -0.9149567752697743694, 32.47697140010484418, 3.785418454572508473 ) ) ;
#40948 = CARTESIAN_POINT ( 'NONE',  ( -58.60151899684544929, -0.7129426177415260080, 0.1461293658716241728 ) ) ;
#40949 = EDGE_CURVE ( 'NONE', #33280, #41032, #20967, .T. ) ;
#40950 = CARTESIAN_POINT ( 'NONE',  ( -3.769861741716944881, -2.021032284792064093, -2.673854242032364326 ) ) ;
#40951 = CARTESIAN_POINT ( 'NONE',  ( 5.138962689587240007, 120.6777149489875569, 0.7548553450424397848 ) ) ;
#40952 = CARTESIAN_POINT ( 'NONE',  ( 2.962760531859824464, 39.20946620154573026, 1.117747612521613254 ) ) ;
#40953 = CARTESIAN_POINT ( 'NONE',  ( -3.089687104934498940, 107.8271213589905386, 4.353618003723240371 ) ) ;
#40954 = TOROIDAL_SURFACE ( 'NONE', #25941, 3.683000000000000718, 0.5080000000000000071 ) ;
#40955 = CARTESIAN_POINT ( 'NONE',  ( -4.274281473441157608, 3.541781053574249327, 1.790774723582081451 ) ) ;
#40956 = CARTESIAN_POINT ( 'NONE',  ( -1.820350978615107751, 35.44831059284695129, 0.3018992756893351115 ) ) ;
#40957 = CARTESIAN_POINT ( 'NONE',  ( 7.448509604456053701, -5.047432113992361025, -3.928768625439613693 ) ) ;
#40958 = CARTESIAN_POINT ( 'NONE',  ( -57.47393550255000605, 1.325481720219651161, -0.09114234605509195786 ) ) ;
#40959 = CARTESIAN_POINT ( 'NONE',  ( -5.520563110719297839, 116.8899318124889959, -0.5663404003195862124 ) ) ;
#40960 = CARTESIAN_POINT ( 'NONE',  ( -0.3260985403866875632, 116.4813942609866899, -1.528836360202051381 ) ) ;
#40961 = FACE_OUTER_BOUND ( 'NONE', #24899, .T. ) ;
#40962 = DIRECTION ( 'NONE',  ( 5.188838149069471174E-16, -1.699382548006136313E-16, -1.000000000000000000 ) ) ;
#40963 = CARTESIAN_POINT ( 'NONE',  ( 8.369700380136936957, -11.69135346447765933, 0.7700151973242596037 ) ) ;
#40964 = CARTESIAN_POINT ( 'NONE',  ( 0.1782134618826983208, 117.3993841988815205, 1.495935623649740309 ) ) ;
#40965 = LINE ( 'NONE', #24760, #38252 ) ;
#40966 = CARTESIAN_POINT ( 'NONE',  ( -6.439703808512989190E-14, 63.33946620154573282, 4.464395889055755859E-29 ) ) ;
#40967 = EDGE_CURVE ( 'NONE', #22781, #12250, #29659, .T. ) ;
#40968 = CARTESIAN_POINT ( 'NONE',  ( 0.1450076288960709392, 106.1446358501009826, -5.226538226828138178 ) ) ;
#40969 = CARTESIAN_POINT ( 'NONE',  ( -22.71658102202245999, 150.3666470947781022, 0.1371106802449220952 ) ) ;
#40970 = ORIENTED_EDGE ( 'NONE', *, *, #29229, .F. ) ;
#40971 = CARTESIAN_POINT ( 'NONE',  ( -58.23655390014408084, 1.485667022650544178, -0.5301823895692313604 ) ) ;
#40972 = VECTOR ( 'NONE', #18777, 1000.000000000000000 ) ;
#40973 = EDGE_CURVE ( 'NONE', #25156, #15597, #28605, .T. ) ;
#40974 = EDGE_LOOP ( 'NONE', ( #8118, #33674, #31383, #6834, #6604 ) ) ;
#40975 = CARTESIAN_POINT ( 'NONE',  ( -46.92937102808790684, 20.25120335581517850, -4.971330492145701108 ) ) ;
#40976 = CARTESIAN_POINT ( 'NONE',  ( -4.610571905486848365, 121.2017135396456098, -0.05649303170681751335 ) ) ;
#40977 = CARTESIAN_POINT ( 'NONE',  ( 3.031078967112608158, -15.50598464685963584, 5.611516622434578494 ) ) ;
#40978 = CARTESIAN_POINT ( 'NONE',  ( -20.82688902969348987, 148.9555414352193168, 1.562960617212841408 ) ) ;
#40979 = EDGE_CURVE ( 'NONE', #12640, #19740, #24963, .T. ) ;
#40980 = CARTESIAN_POINT ( 'NONE',  ( 21.25505906629468100, 136.5942649496780632, -0.9712689567086302267 ) ) ;
#40981 = CARTESIAN_POINT ( 'NONE',  ( -0.6244342276652131707, 19.93415720681881353, -4.586363120317934694 ) ) ;
#40982 = CARTESIAN_POINT ( 'NONE',  ( -1.396185014843847272, 159.5914066142653098, -0.2870382629871535141 ) ) ;
#40983 = CARTESIAN_POINT ( 'NONE',  ( -49.36731013057508477, 17.28484899067109737, -5.052703343809739955 ) ) ;
#40984 = ORIENTED_EDGE ( 'NONE', *, *, #25909, .F. ) ;
#40985 = CARTESIAN_POINT ( 'NONE',  ( -2.186569186605118009, 116.2037677190601386, -0.01283534594974703423 ) ) ;
#40986 = CARTESIAN_POINT ( 'NONE',  ( -4.329049305160163286, 120.0471566133196291, 0.6733469523851640659 ) ) ;
#40987 = CARTESIAN_POINT ( 'NONE',  ( -56.41675102093069682, 3.888360460423796905, -2.207292246800581115 ) ) ;
#40988 = CARTESIAN_POINT ( 'NONE',  ( 6.185003182635295360, 157.2590385278250267, -1.713690555389224102 ) ) ;
#40989 = CARTESIAN_POINT ( 'NONE',  ( -14.04349332752986257, 121.9525460547650226, -1.645664411013196382 ) ) ;
#40990 = CARTESIAN_POINT ( 'NONE',  ( -56.65231406860745977, 4.194353530936431262, -2.518504496425251205 ) ) ;
#40991 = VECTOR ( 'NONE', #22594, 1000.000000000000000 ) ;
#40992 = CARTESIAN_POINT ( 'NONE',  ( 6.511415066510850558, 121.4051597255373025, -0.4520850151541541684 ) ) ;
#40993 = ORIENTED_EDGE ( 'NONE', *, *, #31856, .F. ) ;
#40994 = CARTESIAN_POINT ( 'NONE',  ( -3.724242145611234012, 156.8112981010400802, -1.651639321868204391 ) ) ;
#40995 = CARTESIAN_POINT ( 'NONE',  ( 4.228667402019948618, -15.40433107038223426, 0.8683934293704824725 ) ) ;
#40996 = CARTESIAN_POINT ( 'NONE',  ( -4.378978151537658903, 118.1614286189266778, -0.6690952136889736224 ) ) ;
#40997 = CARTESIAN_POINT ( 'NONE',  ( -57.81953393267934160, 1.609514594907199392, -1.636666387507151432 ) ) ;
#40998 = AXIS2_PLACEMENT_3D ( 'NONE', #3234, #16193, #41591 ) ;
#40999 = DIRECTION ( 'NONE',  ( 0.01997839162482749689, 1.040247600000945640E-18, -0.9998004120163610509 ) ) ;
#41000 = CARTESIAN_POINT ( 'NONE',  ( 13.78152227852067213, 152.5163154464351294, 2.142015651154440814 ) ) ;
#41001 = DIRECTION ( 'NONE',  ( 0.9998004120163609398, 0.000000000000000000, 0.01997839162482749689 ) ) ;
#41002 = CARTESIAN_POINT ( 'NONE',  ( -4.785772612713214080, 1.365856510964248649, -6.940074030798050408 ) ) ;
#41003 = CARTESIAN_POINT ( 'NONE',  ( 6.012785076883544910, 155.3544091381320982, 0.3765917842305994134 ) ) ;
#41004 = DIRECTION ( 'NONE',  ( -9.627370216492862708E-17, -1.000000000000000000, 0.000000000000000000 ) ) ;
#41005 = EDGE_CURVE ( 'NONE', #329, #18659, #35871, .T. ) ;
#41007 = VERTEX_POINT ( 'NONE', #16356 ) ;
#41006 = CARTESIAN_POINT ( 'NONE',  ( -41.31025181302593552, 22.81788724727718076, -1.523999999999993804 ) ) ;
#41008 = CARTESIAN_POINT ( 'NONE',  ( -17.14500000000466784, 71.11999999999886768, 1.269999999999998241 ) ) ;
#41009 = CARTESIAN_POINT ( 'NONE',  ( -7.788926316761409119, 122.5994947058344593, -0.3062370965690639490 ) ) ;
#41010 = CARTESIAN_POINT ( 'NONE',  ( -57.91458998086623922, 0.5482684225795314559, 0.1438514718893008637 ) ) ;
#41011 = CARTESIAN_POINT ( 'NONE',  ( -51.68408071790322822, 18.36713515631302585, 1.546689197337238753 ) ) ;
#41012 = CARTESIAN_POINT ( 'NONE',  ( -18.71881220850887217, 125.2636347375217838, -0.1974931939226152733 ) ) ;
#41013 = EDGE_LOOP ( 'NONE', ( #33475, #36151, #32268, #36319 ) ) ;
#41014 = CARTESIAN_POINT ( 'NONE',  ( -48.35963184368405621, 21.82761434182101112, -2.838462189984265915 ) ) ;
#41015 = CARTESIAN_POINT ( 'NONE',  ( 6.916265728684992453, 121.8189303826054726, -0.2423212107496697243 ) ) ;
#41016 = CARTESIAN_POINT ( 'NONE',  ( -7.882738460396780056, 122.2119657951150629, 0.4812898729222708227 ) ) ;
#41017 = ORIENTED_EDGE ( 'NONE', *, *, #17931, .F. ) ;
#41018 = CARTESIAN_POINT ( 'NONE',  ( 0.3155153238127385018, 115.7029491485453150, -1.753375921699725115 ) ) ;
#41019 = CARTESIAN_POINT ( 'NONE',  ( -11.24781102592754145, 128.1602342495223468, -0.5025223919565848796 ) ) ;
#41020 = CARTESIAN_POINT ( 'NONE',  ( 5.396235140300779776, -11.83248475511457976, 0.6634469457710948648 ) ) ;
#41021 = CARTESIAN_POINT ( 'NONE',  ( -10.89609060007118835, 119.5270080912504653, 0.8636533125102806574 ) ) ;
#41022 = DIRECTION ( 'NONE',  ( 0.9998004120163609398, 0.000000000000000000, 0.01997839162482749689 ) ) ;
#41023 = VECTOR ( 'NONE', #25907, 1000.000000000000000 ) ;
#41024 = CARTESIAN_POINT ( 'NONE',  ( 23.42751387171875521, 146.8275480241000253, 0.6231101672962392479 ) ) ;
#41025 = ADVANCED_FACE ( 'NONE', ( #38122 ), #16023, .F. ) ;
#41026 = CARTESIAN_POINT ( 'NONE',  ( 4.609146067579531270, 121.2017137070652097, 0.1277310477265502786 ) ) ;
#41027 = CARTESIAN_POINT ( 'NONE',  ( -26.29578028364076658, 73.87584665086983193, 1.269999999999993134 ) ) ;
#41028 = CARTESIAN_POINT ( 'NONE',  ( 0.7179688673824197176, 19.28876970375581479, -0.6613080194383522681 ) ) ;
#41029 = CARTESIAN_POINT ( 'NONE',  ( -20.46883641438838453, 129.0748834149669904, -0.4693348210411829591 ) ) ;
#41030 = CARTESIAN_POINT ( 'NONE',  ( -46.98357728082498852, 20.33138823660016214, -5.073745951255736131 ) ) ;
#41031 = DIRECTION ( 'NONE',  ( 0.000000000000000000, 0.000000000000000000, 1.000000000000000000 ) ) ;
#41032 = VERTEX_POINT ( 'NONE', #5197 ) ;
#41033 = CARTESIAN_POINT ( 'NONE',  ( 5.762928754573319878, 118.2277084192942738, 1.125902124160973905 ) ) ;
#41034 = CARTESIAN_POINT ( 'NONE',  ( -7.461250000000053006, 83.56599999999998829, 9.137395930138198251E-16 ) ) ;
#41035 = CARTESIAN_POINT ( 'NONE',  ( 22.07943683853326178, 148.3267584643486146, 2.032026126618132533 ) ) ;
#41036 = CARTESIAN_POINT ( 'NONE',  ( -58.52535285190720060, -0.5719483744804805259, -0.2498204902909159641 ) ) ;
#41037 = CARTESIAN_POINT ( 'NONE',  ( 6.779039758441031793, 118.9580315507705706, -0.9776869392460786345 ) ) ;
#41038 = CARTESIAN_POINT ( 'NONE',  ( 5.629075615873821548, 21.71503808657377022, 6.277010319805454763 ) ) ;
#41039 = CARTESIAN_POINT ( 'NONE',  ( -21.87689675406264556, 150.0588410196355937, -1.874897916013938737 ) ) ;
#41040 = CARTESIAN_POINT ( 'NONE',  ( 4.899310882224675368, 117.5479452163036171, -0.9252960604191319272 ) ) ;
#41041 = CARTESIAN_POINT ( 'NONE',  ( 7.449435858333443683, 123.6645382909113664, 0.1834419053087676110 ) ) ;
#41042 = ORIENTED_EDGE ( 'NONE', *, *, #7412, .T. ) ;
#41043 = CARTESIAN_POINT ( 'NONE',  ( -0.6527697516718347082, 156.3069099058775748, 0.1169209421757348294 ) ) ;
#41044 = CARTESIAN_POINT ( 'NONE',  ( -18.66896445097611590, 144.8948545501563103, -2.490227693099508421 ) ) ;
#41045 = CARTESIAN_POINT ( 'NONE',  ( 4.849545180983690251, -15.35966036743073637, 3.882997576023691444 ) ) ;
#41046 = MECHANICAL_DESIGN_GEOMETRIC_PRESENTATION_REPRESENTATION (  '', ( #17219 ), #34933 ) ;
#41047 = CARTESIAN_POINT ( 'NONE',  ( -9.960492004070040650, 64.81807050032566053, -1.269999999999996021 ) ) ;
#41048 = CARTESIAN_POINT ( 'NONE',  ( 4.792324638247207780, 56.51998046905276141, 4.972049999977001811 ) ) ;
#41049 = ORIENTED_EDGE ( 'NONE', *, *, #11000, .T. ) ;
#41050 = CARTESIAN_POINT ( 'NONE',  ( 13.10180873912553068, 153.9517556018257096, 2.260155593826742582 ) ) ;
#41051 = CARTESIAN_POINT ( 'NONE',  ( 12.21488373879589240, 55.24500000000000455, -4.381499999999999950 ) ) ;
#41052 = CARTESIAN_POINT ( 'NONE',  ( -4.611806494114576438, 117.9324678712513759, -0.9633187536371230486 ) ) ;
#41053 = AXIS2_PLACEMENT_3D ( 'NONE', #8622, #31621, #5234 ) ;
#41054 = CARTESIAN_POINT ( 'NONE',  ( -1.490732016122501502, 115.2915405621345144, 1.797152713846303040 ) ) ;
#41055 = CARTESIAN_POINT ( 'NONE',  ( 7.865828698536367902, -6.344330755464622662, 3.006797519310529854 ) ) ;
#41056 = CARTESIAN_POINT ( 'NONE',  ( 9.347632431636288430, 123.5785764018267514, 0.8560492856234919179 ) ) ;
#41057 = CARTESIAN_POINT ( 'NONE',  ( -42.09814309847200064, 23.46876350539121248, -1.524000000000005794 ) ) ;
#41058 = CARTESIAN_POINT ( 'NONE',  ( 20.86923087398506027, 132.2939277659177151, -0.4710007621541094647 ) ) ;
#41059 = CARTESIAN_POINT ( 'NONE',  ( 5.570375128628212380, 56.51500000000003610, -4.419987129958417249 ) ) ;
#41060 = CARTESIAN_POINT ( 'NONE',  ( -58.30142669622183860, -0.1470572696064289253, 0.3334503007892540283 ) ) ;
#41061 = CYLINDRICAL_SURFACE ( 'NONE', #11232, 0.5080000000000000071 ) ;
#41062 = CARTESIAN_POINT ( 'NONE',  ( 1.848046085800037375, -15.12359198595263088, 5.521975501593074043 ) ) ;
#41063 = CARTESIAN_POINT ( 'NONE',  ( -4.289101050795583348, 118.2138500885050689, 0.3554350998168962494 ) ) ;
#41064 = CARTESIAN_POINT ( 'NONE',  ( -23.45208337669183152, 146.8499405026647651, -0.4686284387228153991 ) ) ;
#41065 = VERTEX_POINT ( 'NONE', #5404 ) ;
#41066 = CARTESIAN_POINT ( 'NONE',  ( -50.78166962549567387, 16.07998339508975860, 4.893817234114164805 ) ) ;
#41067 = EDGE_CURVE ( 'NONE', #39604, #18019, #39797, .T. ) ;
#41068 = CARTESIAN_POINT ( 'NONE',  ( 8.324009791931711533, 120.1221279132020783, -1.118190249840247397 ) ) ;
#41069 = CARTESIAN_POINT ( 'NONE',  ( 5.336581877858352030, 116.0444662015457595, -0.07592003752709637621 ) ) ;
#41070 = CIRCLE ( 'NONE', #28142, 0.2539999999999983937 ) ;
#41071 = CARTESIAN_POINT ( 'NONE',  ( 4.398790584699274753, 118.1654141809896288, 0.6513841008152672085 ) ) ;
#41072 = CARTESIAN_POINT ( 'NONE',  ( -9.518183030555464441, 123.9284174147966269, -0.7933090623874851088 ) ) ;
#41073 = CARTESIAN_POINT ( 'NONE',  ( -28.65049350906917880, 77.81814547195517662, 1.269999999999990248 ) ) ;
#41074 = CARTESIAN_POINT ( 'NONE',  ( 15.73471677569731142, 120.8416612192341972, 0.3144170877231856065 ) ) ;
#41075 = EDGE_CURVE ( 'NONE', #2842, #17342, #5826, .T. ) ;
#41076 = ORIENTED_EDGE ( 'NONE', *, *, #14506, .F. ) ;
#41077 = CARTESIAN_POINT ( 'NONE',  ( 4.622858883031034871, 26.85595184169372374, 0.2084198311932836112 ) ) ;
#41078 = CARTESIAN_POINT ( 'NONE',  ( -29.81772749323155836, 58.81923324275946641, 1.269999999999994023 ) ) ;
#41079 = CYLINDRICAL_SURFACE ( 'NONE', #41204, 0.6350000000000006750 ) ;
#41080 = CARTESIAN_POINT ( 'NONE',  ( -42.73979388487843067, 22.09733806376297238, 1.954747716863125984 ) ) ;
#41081 = DIRECTION ( 'NONE',  ( -0.9998004120163608288, 0.000000000000000000, -0.01997839162482750383 ) ) ;
#41082 = CARTESIAN_POINT ( 'NONE',  ( 6.083407471064808725, 121.3513819447846060, 0.4752266484690387260 ) ) ;
#41083 = CARTESIAN_POINT ( 'NONE',  ( -4.487480840803009130, 27.34045677879159442, -1.100063755011520872 ) ) ;
#41084 = CARTESIAN_POINT ( 'NONE',  ( 22.83601474261759989, 146.5373477140321938, 1.546791039490589492 ) ) ;
#41085 = CARTESIAN_POINT ( 'NONE',  ( 0.2217520613055987411, 104.6144662015457101, -4.831251598276631753 ) ) ;
#41087 = CARTESIAN_POINT ( 'NONE',  ( 20.77691070360829784, 149.9184980045912425, -1.462349339025473371 ) ) ;
#41086 = CARTESIAN_POINT ( 'NONE',  ( 2.849840736555561360, -14.15504780656048922, 0.1227973400909937313 ) ) ;
#41088 = CARTESIAN_POINT ( 'NONE',  ( -17.81946051592207070, 148.9562551477873740, 1.662425298156809506 ) ) ;
#41089 = CARTESIAN_POINT ( 'NONE',  ( 0.3943543298815788134, 25.17882533764851871, -4.623353113333005915 ) ) ;
#41090 = CARTESIAN_POINT ( 'NONE',  ( -14.80341400616319625, 120.8492938200443092, -1.052940121379140725 ) ) ;
#41091 = VECTOR ( 'NONE', #34511, 1000.000000000000000 ) ;
#41092 = CARTESIAN_POINT ( 'NONE',  ( -0.9708255322354510941, 17.08399857615920325, -0.1324238259073569901 ) ) ;
#41093 = VERTEX_POINT ( 'NONE', #41394 ) ;
#41094 = CARTESIAN_POINT ( 'NONE',  ( -55.83515739322318439, 4.224161455597882586, -9.574893020535344595E-15 ) ) ;
#41095 = CARTESIAN_POINT ( 'NONE',  ( -7.650102001921326611, 122.3449549946481056, 0.2051776793030278268 ) ) ;
#41096 = CARTESIAN_POINT ( 'NONE',  ( 4.521557965551993519, -14.38033123432501448, 4.565926699156682922 ) ) ;
#41097 = CARTESIAN_POINT ( 'NONE',  ( 16.73823235880707472, 147.9788754379930822, -1.246688593732825590 ) ) ;
#41098 = CIRCLE ( 'NONE', #31568, 0.2540000000000000036 ) ;
#41099 = ORIENTED_EDGE ( 'NONE', *, *, #10441, .F. ) ;
#41100 = CARTESIAN_POINT ( 'NONE',  ( 0.7365107854829129330, 115.7029383640674212, 1.756173502283182364 ) ) ;
#41101 = ORIENTED_EDGE ( 'NONE', *, *, #22719, .F. ) ;
#41102 = CARTESIAN_POINT ( 'NONE',  ( -4.896113279795653916, 117.6590624440263468, -0.9620818870509636467 ) ) ;
#41103 = CARTESIAN_POINT ( 'NONE',  ( 4.591655703643790609, 121.2030596905490540, 0.06445270968432179060 ) ) ;
#41104 = ORIENTED_EDGE ( 'NONE', *, *, #30723, .F. ) ;
#41105 = CARTESIAN_POINT ( 'NONE',  ( 12.79701950029124902, 155.3440856034525837, 2.194532851538729457 ) ) ;
#41106 = CARTESIAN_POINT ( 'NONE',  ( -5.475330206976867231, 57.14999999999999147, 5.107412922131463695 ) ) ;
#41107 = CIRCLE ( 'NONE', #36351, 0.3810000000000007825 ) ;
#41108 = CARTESIAN_POINT ( 'NONE',  ( -8.761523658392189162, 74.56051954986229191, -1.269999999999997131 ) ) ;
#41109 = CARTESIAN_POINT ( 'NONE',  ( 0.02615207601215727498, 159.0391464308674756, -1.308756824028193044 ) ) ;
#41110 = CARTESIAN_POINT ( 'NONE',  ( 5.816519783795321530, 117.0096406922080376, -0.1181936270109637949 ) ) ;
#41111 = DIRECTION ( 'NONE',  ( 0.9998004120163608288, 4.016384292689131511E-17, 0.01997839162482749342 ) ) ;
#41112 = CARTESIAN_POINT ( 'NONE',  ( 1.691696049192186857, -15.24586544832738610, 5.783975733521854679 ) ) ;
#41113 = CARTESIAN_POINT ( 'NONE',  ( -19.21741104974024594, 79.92823415920659613, -1.524000000000003352 ) ) ;
#41114 = CARTESIAN_POINT ( 'NONE',  ( -41.23752580366542020, 23.26788267949596190, -1.524000000000005128 ) ) ;
#41115 = CARTESIAN_POINT ( 'NONE',  ( -4.729254454615190895, 117.9669711668249619, 0.6196972108808941337 ) ) ;
#41116 = ORIENTED_EDGE ( 'NONE', *, *, #18498, .T. ) ;
#41117 = ORIENTED_EDGE ( 'NONE', *, *, #26125, .T. ) ;
#41118 = DIRECTION ( 'NONE',  ( 0.4849315768086426282, 0.8745520943968310146, 1.030032898892908135E-16 ) ) ;
#41119 = CARTESIAN_POINT ( 'NONE',  ( 3.245646068532854311, 118.3825688634768625, -0.7783404868572983970 ) ) ;
#41120 = CARTESIAN_POINT ( 'NONE',  ( -3.333432127168630021, 112.1633951907056996, -2.855042910325920502 ) ) ;
#41121 = CARTESIAN_POINT ( 'NONE',  ( 4.861520819079757416, 117.7423039542964318, 0.9146368285113327667 ) ) ;
#41122 = CARTESIAN_POINT ( 'NONE',  ( -4.755622421505391273, 117.4716786420896284, -1.195466823065375994 ) ) ;
#41123 = CARTESIAN_POINT ( 'NONE',  ( -0.06282972276048238991, 111.5577547982949227, 3.144256248693377387 ) ) ;
#41124 = FILL_AREA_STYLE_COLOUR ( '', #35604 ) ;
#41125 = CARTESIAN_POINT ( 'NONE',  ( -29.94429436251954613, 71.80236127745905605, 1.269999999999991580 ) ) ;
#41126 = DIRECTION ( 'NONE',  ( 1.000000000000000000, 0.000000000000000000, 0.000000000000000000 ) ) ;
#41127 = CARTESIAN_POINT ( 'NONE',  ( 3.247910276010201880, -14.18928037215049009, 3.960261243354706640 ) ) ;
#41128 = CARTESIAN_POINT ( 'NONE',  ( 0.3401008104887150441, 105.9117620634264370, -5.317146732969808554 ) ) ;
#41129 = CARTESIAN_POINT ( 'NONE',  ( -16.92358334414620913, 148.6336825499269310, -2.141768463193927552 ) ) ;
#41130 = ADVANCED_FACE ( 'NONE', ( #35007 ), #5283, .T. ) ;
#41131 = CARTESIAN_POINT ( 'NONE',  ( 5.135883789155748502, 116.9356663392523501, -0.1807461257199506066 ) ) ;
#41132 = CARTESIAN_POINT ( 'NONE',  ( -3.299905295350023415, 32.79871628568109543, 4.342002458138856547 ) ) ;
#41133 = CARTESIAN_POINT ( 'NONE',  ( -1.799679211148575542, 115.7029357389137090, 1.654552292944202030 ) ) ;
#41134 = CARTESIAN_POINT ( 'NONE',  ( -1.576536484031922480, 10.66345178295009788, -4.350723848753511369 ) ) ;
#41136 = VERTEX_POINT ( 'NONE', #41178 ) ;
#41135 = CARTESIAN_POINT ( 'NONE',  ( 7.949750681159606813, 158.6775731370129279, 0.5882489250746236742 ) ) ;
#41137 = CARTESIAN_POINT ( 'NONE',  ( -1.824400206236523658, 104.6144662015369278, -5.024575765548627615 ) ) ;
#41138 = CARTESIAN_POINT ( 'NONE',  ( 4.210067206397440032, -15.44688347603401191, 1.362376457177303157 ) ) ;
#41139 = CARTESIAN_POINT ( 'NONE',  ( -12.77186547895210467, 122.8260676081006153, 1.334005200199291252 ) ) ;
#41140 = CARTESIAN_POINT ( 'NONE',  ( -0.9746272421432693456, 17.39786500698104277, 0.06925455797152506310 ) ) ;
#41141 = CARTESIAN_POINT ( 'NONE',  ( 0.9750733387068674096, 18.20995955126885590, -0.03652159252302569076 ) ) ;
#41142 = ORIENTED_EDGE ( 'NONE', *, *, #27436, .T. ) ;
#41143 = VERTEX_POINT ( 'NONE', #11771 ) ;
#41144 = DIRECTION ( 'NONE',  ( -4.017660918040594346E-17, 1.000000000000000000, 2.376309959284832031E-19 ) ) ;
#41145 = CARTESIAN_POINT ( 'NONE',  ( 0.9980778803427338142, 110.6314368487224300, 3.458106935563856066 ) ) ;
#41146 = CARTESIAN_POINT ( 'NONE',  ( -9.968563030426437876, 123.7598584631124794, 0.7002966798862196862 ) ) ;
#41147 = DIRECTION ( 'NONE',  ( 0.01731298258488003436, -0.9998501190848634312, 0.000000000000000000 ) ) ;
#41148 = CARTESIAN_POINT ( 'NONE',  ( 2.953219771904812774, -14.51063682438745417, 4.500484459945554683 ) ) ;
#41149 = CARTESIAN_POINT ( 'NONE',  ( 17.86368224974575369, 148.4245508482893854, -1.618106657999740072 ) ) ;
#41150 = CARTESIAN_POINT ( 'NONE',  ( -19.41896158923250226, 149.6234262069624492, -2.479904253118717428 ) ) ;
#41151 = DIRECTION ( 'NONE',  ( -0.8745520943968249084, 0.4849315768086533418, -5.271987356194193006E-16 ) ) ;
#41152 = CARTESIAN_POINT ( 'NONE',  ( -4.218275339060285845, 155.8585684991085714, -0.08429118021179402009 ) ) ;
#41153 = CARTESIAN_POINT ( 'NONE',  ( 4.074910602682932925, 118.2429491485453354, -0.1454311599470142491 ) ) ;
#41154 = CARTESIAN_POINT ( 'NONE',  ( 12.26386414673826053, 130.6044139104978115, -0.2969705276545479555 ) ) ;
#41155 = ORIENTED_EDGE ( 'NONE', *, *, #34773, .F. ) ;
#41156 = CARTESIAN_POINT ( 'NONE',  ( 2.849840736555561360, -14.15504780656048922, 0.1227973400909937313 ) ) ;
#41157 = LINE ( 'NONE', #24159, #36710 ) ;
#41158 = CARTESIAN_POINT ( 'NONE',  ( -3.890668369019033790, 28.55756886444902065, 1.917437575001416539 ) ) ;
#41159 = B_SPLINE_CURVE_WITH_KNOTS ( 'NONE', 3,
 ( #35832, #6648, #3458, #38809, #9621, #32210, #6029, #35621, #6231, #16205, #39229 ),
 .UNSPECIFIED., .F., .F.,
 ( 4, 1, 1, 1, 1, 1, 1, 1, 4 ),
 ( 0.000000000000000000, 0.1249999999999979600, 0.2500000000000013878, 0.3749999999999938383, 0.4999999999999972800, 0.6249999999999980016, 0.7499999999999986677, 0.8749999999999993339, 1.000000000000000000 ),
 .UNSPECIFIED. ) ;
#41160 = CARTESIAN_POINT ( 'NONE',  ( -54.71920516548560443, 7.857264873391931026, 3.427457936775551328 ) ) ;
#41161 = CARTESIAN_POINT ( 'NONE',  ( 2.901706292870370518, -4.507343114274551255, -3.632229383212865592 ) ) ;
#41162 = CARTESIAN_POINT ( 'NONE',  ( 9.375340687752114377, 122.9055586947561522, 1.148039706409768490 ) ) ;
#41163 = CARTESIAN_POINT ( 'NONE',  ( 2.866728174840395216, 37.98889525090484653, 1.397978221435859147 ) ) ;
#41164 = CARTESIAN_POINT ( 'NONE',  ( -7.643874070029948342, 124.9344662015457317, -0.1527427953284559992 ) ) ;
#41165 = CARTESIAN_POINT ( 'NONE',  ( 1.968029828064305153, -3.592386099649644837, 4.203610184747879508 ) ) ;
#41166 = CARTESIAN_POINT ( 'NONE',  ( 9.049782359939477772, 124.0675141969884692, 0.1808361888366267212 ) ) ;
#41167 = ADVANCED_FACE ( 'NONE', ( #18360 ), #29746, .T. ) ;
#41168 = TOROIDAL_SURFACE ( 'NONE', #22772, 3.683000000000000718, 0.5080000000000000071 ) ;
#41169 = CARTESIAN_POINT ( 'NONE',  ( -7.266063235143556120, -1.810023253287891487, -4.326994388187479501 ) ) ;
#41170 = CARTESIAN_POINT ( 'NONE',  ( -57.43854689232674815, 1.757847328446637825, -1.624773336220253439 ) ) ;
#41171 = CARTESIAN_POINT ( 'NONE',  ( 2.154416292954056455, 116.4931154949332068, -0.2946284726465266401 ) ) ;
#41172 = CARTESIAN_POINT ( 'NONE',  ( -0.3746108773303726824, 122.5569158606515003, -0.2627672029693575717 ) ) ;
#41173 = LINE ( 'NONE', #11977, #17154 ) ;
#41174 = CARTESIAN_POINT ( 'NONE',  ( -5.719305292821792008, 76.92870498041706639, 1.270000000000003348 ) ) ;
#41175 = CARTESIAN_POINT ( 'NONE',  ( -6.853500063829680577, -7.707324007402828414, -4.930749982112237362 ) ) ;
#41176 = CARTESIAN_POINT ( 'NONE',  ( 0.07395884426403227796, 117.3993836134447690, 1.494938254265739896 ) ) ;
#41177 = CARTESIAN_POINT ( 'NONE',  ( -29.50431010628811990, 60.44740661353770150, 1.523999999999994026 ) ) ;
#41178 = CARTESIAN_POINT ( 'NONE',  ( -5.878298779570172883, 78.21245918282636467, -1.269999999999996243 ) ) ;
#41179 = EDGE_CURVE ( 'NONE', #37741, #13569, #16128, .T. ) ;
#41180 = CARTESIAN_POINT ( 'NONE',  ( 0.3798947725661321884, 120.3637084677653633, -0.5835535210198282696 ) ) ;
#41181 = CARTESIAN_POINT ( 'NONE',  ( -20.50889283491270376, 152.5656283612522657, 0.2944088047499980876 ) ) ;
#41182 = EDGE_LOOP ( 'NONE', ( #2530, #17992, #28979, #1241 ) ) ;
#41183 = CARTESIAN_POINT ( 'NONE',  ( -58.83227707057485389, -0.08366279997994163775, -5.785609034356198713E-15 ) ) ;
#41184 = ORIENTED_EDGE ( 'NONE', *, *, #32111, .T. ) ;
#41185 = LINE ( 'NONE', #42032, #38945 ) ;
#41186 = CARTESIAN_POINT ( 'NONE',  ( -8.903120925483809955, 123.9008333197534029, -0.1338047255859078355 ) ) ;
#41187 = CARTESIAN_POINT ( 'NONE',  ( 6.397261194921658678, -14.09295207620744961, -0.07176229933514734205 ) ) ;
#41188 = CARTESIAN_POINT ( 'NONE',  ( -14.21869788239195032, 123.4894365733723447, 1.306911315328640910 ) ) ;
#41189 = CARTESIAN_POINT ( 'NONE',  ( 7.640054841935559615, 158.5456267226934131, -0.8603666243017552562 ) ) ;
#41190 = CARTESIAN_POINT ( 'NONE',  ( -0.1328416520900886078, 24.48205809745167372, 4.627450821846854190 ) ) ;
#41191 = CARTESIAN_POINT ( 'NONE',  ( -10.73501234801834769, 157.9381345072164038, -0.5669044750022471657 ) ) ;
#41192 = CARTESIAN_POINT ( 'NONE',  ( -57.87347402819683850, 1.335634876923293746, -1.488528580188531736 ) ) ;
#41193 = EDGE_CURVE ( 'NONE', #35053, #15866, #28062, .T. ) ;
#41194 = EDGE_LOOP ( 'NONE', ( #21510, #3867, #42094, #22508 ) ) ;
#41195 = CARTESIAN_POINT ( 'NONE',  ( -5.562361497059077564, 116.7271819370821078, 0.05426658518331221870 ) ) ;
#41196 = CARTESIAN_POINT ( 'NONE',  ( -6.640726327341849406E-14, 100.6774662015457409, -1.320564745697255449E-18 ) ) ;
#41197 = B_SPLINE_SURFACE_WITH_KNOTS ( 'NONE', 3, 3, ( 
 ( #21584, #38233, #18616, #5441, #38015, #11598, #15423, #28425, #27997 ),
 ( #41006, #40592, #9049, #28212, #41431, #37384, #8200, #12237, #41219 ),
 ( #21374, #25228, #35044, #22015, #17775, #40798, #30773, #1623, #27583 ),
 ( #25014, #11812, #21171, #18399, #24582, #34202, #24803, #5028, #27789 ),
 ( #17985, #1823, #37796, #37588, #34400, #31190, #8416, #2034, #16045 ),
 ( #35668, #39278, #29048, #32673, #9460, #38652, #18827, #38855, #19658 ),
 ( #19453, #6478, #32463, #15628, #316, #42065, #3508, #31831, #13283 ),
 ( #19033, #2876, #15838, #32256, #26267, #22217, #16469, #25446, #2669 ),
 ( #35881, #28845, #5864, #3291, #35248, #35452, #12861, #6275, #16253 ),
 ( #22632, #22841, #29473, #28631, #10083, #26058, #29257, #38444, #23056 ),
 ( #6691, #19246, #6072, #9667, #9871, #25645, #32039, #3085, #41644 ),
 ( #12451, #9259, #41858, #12655, #103, #25848, #22424, #13068, #39069 ),
 ( #33310, #30305, #33101, #26701, #17518, #10297, #13912, #26905, #39706 ),
 ( #19874, #4354, #4139, #26487, #23692, #27328, #17100, #20711, #10508 ),
 ( #6903, #39918, #7744, #23478, #36503, #40340, #32888, #1358, #30518 ),
 ( #23910, #7123, #7324, #23266, #13499, #10712, #39491, #36301, #14117 ),
 ( #20078, #3932, #3720, #16891, #16679, #27114, #14316, #36926, #36711 ),
 ( #29893, #29683, #30103, #11133, #731, #13707, #7532, #20282, #527 ),
 ( #36089, #942, #20493, #33522, #17315, #1148, #40129, #10920, #33735 ),
 ( #4558, #33942, #34569, #14949, #11344, #5396, #2414, #15374, #8576 ),
 ( #24967, #37540, #24329, #27949, #28165, #1777, #37335, #11548, #8792 ),
 ( #41170, #37967, #28379, #41386, #37752, #5189, #4773, #11764, #30938 ),
 ( #21330, #18352, #21123, #14738, #5611, #40546, #1987, #40958, #27741 ),
 ( #7950, #31358, #34357, #14530, #24753, #24120, #18142, #21750, #40751 ),
 ( #37130, #21539, #34777, #24531, #8363, #20919, #17722, #31574, #18567 ),
 ( #11974, #8153, #31146, #34151, #1574, #2201, #27540, #4978, #15159 ),
 ( #17935, #30725, #22533, #35768, #9562, #3830, #36411, #13604, #422 ),
 ( #6585, #25744, #6795, #4039, #10088, #19552, #13392, #12961, #38753 ),
 ( #7229, #22952, #25955, #38962, #13182, #26169, #19762, #29588, #20188 ) ),
 .UNSPECIFIED., .F., .F., .F.,
 ( 4, 1, 1, 1, 1, 1, 1, 2, 1, 1, 1, 1, 1, 1, 1, 1, 1, 1, 1, 1, 1, 1, 1, 1, 1, 4 ),
 ( 4, 1, 1, 1, 1, 1, 4 ),
 ( 0.000000000000000000, 0.03307066603948304734, 0.06614133207896609468, 0.09921199811844919059, 0.1653533301974152714, 0.1984239962368983812, 0.2314946622763813522, 0.2645653283158643787, 0.3105299952961229071, 0.3564946622763812689, 0.4024593292566397418, 0.4484239962368982702, 0.5403533301974150493, 0.6322826641579321061, 0.7242119981184491628, 0.7701766650987074136, 0.8161413320789658865, 0.8850883325493537068, 0.8965794992944182695, 0.9080706660394826102, 0.9195618327845473949, 0.9310529995296121797, 0.9425441662746769644, 0.9540353330197415271, 0.9770176665098706525, 1.000000000000000000 ),
 ( 0.000000000000000000, 0.2500000000000000000, 0.4444444444444445308, 0.5000000000000000000, 0.7500000000000000000, 0.8333333333333333703, 1.000000000000000000 ),
 .UNSPECIFIED. ) ;
#41198 = CARTESIAN_POINT ( 'NONE',  ( -2.533752743582094347, 119.8406177399916714, 0.5716348071481811566 ) ) ;
#41199 = CARTESIAN_POINT ( 'NONE',  ( -57.36480510062817473, 1.874762252804534901, -1.516398777065382175 ) ) ;
#41200 = CARTESIAN_POINT ( 'NONE',  ( 12.19007131875806493, 155.0146010091537221, -1.747022140133383195 ) ) ;
#41201 = CARTESIAN_POINT ( 'NONE',  ( -20.99120442346859861, 145.7918284779248665, -2.367408383378773795 ) ) ;
#41202 = CARTESIAN_POINT ( 'NONE',  ( -50.78166962549567387, 16.07998339508975860, -4.893817234114181680 ) ) ;
#41203 = CARTESIAN_POINT ( 'NONE',  ( 0.006077178772615180087, 120.4695998130595598, -0.3041268764237434197 ) ) ;
#41204 = AXIS2_PLACEMENT_3D ( 'NONE', #4892, #27651, #8905 ) ;
#41205 = EDGE_CURVE ( 'NONE', #22781, #39868, #24286, .T. ) ;
#41206 = ORIENTED_EDGE ( 'NONE', *, *, #5292, .F. ) ;
#41207 = CARTESIAN_POINT ( 'NONE',  ( -18.11471409803314359, 146.9188445454784357, -2.346026295494533009 ) ) ;
#41208 = CARTESIAN_POINT ( 'NONE',  ( 4.228161069935173266, -15.38163066151135361, 0.6048619776675213666 ) ) ;
#41209 = CARTESIAN_POINT ( 'NONE',  ( -4.255713500455158282, 118.2236181106063242, -0.4577248347117505167 ) ) ;
#41210 = ADVANCED_FACE ( 'NONE', ( #37975 ), #8800, .F. ) ;
#41211 = CARTESIAN_POINT ( 'NONE',  ( -57.55343345497419705, 2.880119995625998630, -1.988856187846590018 ) ) ;
#41212 = CARTESIAN_POINT ( 'NONE',  ( -4.801647862231239294, 117.4032733357421137, 1.015449305854420503 ) ) ;
#41213 = CARTESIAN_POINT ( 'NONE',  ( 7.341258159293141183, 120.8389031223305352, 1.207285925005196825 ) ) ;
#41214 = DIRECTION ( 'NONE',  ( -4.017660918040594346E-17, 1.000000000000000000, 2.376309959284834438E-19 ) ) ;
#41215 = EDGE_CURVE ( 'NONE', #21005, #24253, #41312, .T. ) ;
#41216 = CARTESIAN_POINT ( 'NONE',  ( -6.147169039531121371, -7.901875862888119606, -5.777837204501876656 ) ) ;
#41217 = CARTESIAN_POINT ( 'NONE',  ( 4.265939155584976383, 155.8374496918941077, 0.3214930909109447454 ) ) ;
#41218 = CARTESIAN_POINT ( 'NONE',  ( 17.14500000000001023, 57.15000000000000568, -5.016499999999999737 ) ) ;
#41220 = EDGE_LOOP ( 'NONE', ( #3071, #2019, #19847, #30663 ) ) ;
#41219 = CARTESIAN_POINT ( 'NONE',  ( -41.41491986784954804, 22.70581808553406233, -6.121743196690467558E-15 ) ) ;
#41221 = CARTESIAN_POINT ( 'NONE',  ( -0.5465841182417748856, 117.9394513981711299, 1.387505131010090098 ) ) ;
#41222 = CARTESIAN_POINT ( 'NONE',  ( -58.75009580408200094, 0.1057190229620807997, 0.6617493214610802310 ) ) ;
#41223 = CARTESIAN_POINT ( 'NONE',  ( -7.850986424014909204, 122.2449432668186660, -0.7695275123436272624 ) ) ;
#41224 = CARTESIAN_POINT ( 'NONE',  ( -17.08598887363762131, 83.79821757228496892, -1.270000000000002904 ) ) ;
#41225 = CARTESIAN_POINT ( 'NONE',  ( -48.45250714818473625, 19.88962760504932348, 4.734234960885991050 ) ) ;
#41226 = CARTESIAN_POINT ( 'NONE',  ( -23.27479113596638527, 149.3390083238215595, -0.2346540593346968795 ) ) ;
#41227 = ORIENTED_EDGE ( 'NONE', *, *, #34053, .T. ) ;
#41228 = CARTESIAN_POINT ( 'NONE',  ( -48.87999295267864142, 23.89022491863793718, -0.5351834272454536467 ) ) ;
#41229 = CARTESIAN_POINT ( 'NONE',  ( 6.940171632852439210, 121.9095277527773220, -0.09994676863305257397 ) ) ;
#41230 = CARTESIAN_POINT ( 'NONE',  ( -8.325883379001959739, 120.1130057568718144, 1.118334525995478224 ) ) ;
#41231 = VERTEX_POINT ( 'NONE', #31583 ) ;
#41232 = CARTESIAN_POINT ( 'NONE',  ( 1.114896128613473536, 115.7029400299447985, -1.703466781126056873 ) ) ;
#41233 = CARTESIAN_POINT ( 'NONE',  ( -7.835359239711140233, 154.6110463214094182, -0.4315757689284724918 ) ) ;
#41234 = CARTESIAN_POINT ( 'NONE',  ( 4.746351668907457189, -13.71804649124164222, 3.839566941389735977 ) ) ;
#41235 = CARTESIAN_POINT ( 'NONE',  ( -21.87215423617524479, 148.4185114426368841, 1.275166548224079044 ) ) ;
#41236 = CARTESIAN_POINT ( 'NONE',  ( -5.274544067074297793, 115.7029491485453718, 0.8135768287290677803 ) ) ;
#41237 = CARTESIAN_POINT ( 'NONE',  ( 14.79880180360888708, 120.3086691715681695, 0.4511713404943136219 ) ) ;
#41238 = CARTESIAN_POINT ( 'NONE',  ( 15.52687642492882070, 147.5330934759543879, 0.3102639428822866474 ) ) ;
#41239 = DIRECTION ( 'NONE',  ( -0.8745520943968240202, 0.4849315768086551737, -5.361993529360572958E-16 ) ) ;
#41240 = CARTESIAN_POINT ( 'NONE',  ( 0.1081409728947390902, 20.38375149489202443, -0.9727671068919315767 ) ) ;
#41241 = CARTESIAN_POINT ( 'NONE',  ( -16.14716650825978306, 121.2501203052637493, -0.3739013473229989559 ) ) ;
#41242 = DIRECTION ( 'NONE',  ( -5.206863593109713661E-17, 1.000000000000000000, -1.077750396879097183E-30 ) ) ;
#41243 = CARTESIAN_POINT ( 'NONE',  ( -6.059261036834474368, 56.51499999999998636, -4.381499999999999950 ) ) ;
#41244 = ORIENTED_EDGE ( 'NONE', *, *, #22149, .F. ) ;
#41245 = CARTESIAN_POINT ( 'NONE',  ( -8.350588457312666080, 119.9924236745955994, 1.117253148572291188 ) ) ;
#41246 = CARTESIAN_POINT ( 'NONE',  ( 3.517175496330608997, 50.63946620154572997, -1.199971990511068398 ) ) ;
#41247 = CARTESIAN_POINT ( 'NONE',  ( 21.19565729220476058, 150.1117090729339623, 2.124842235463313855 ) ) ;
#41248 = CARTESIAN_POINT ( 'NONE',  ( 14.21869788239182242, 123.4894365733723447, -1.306911315328640910 ) ) ;
#41249 = CARTESIAN_POINT ( 'NONE',  ( 4.409325496788552456, -14.99073161069602911, -1.440227693534741782 ) ) ;
#41250 = CARTESIAN_POINT ( 'NONE',  ( -22.33586214876087794, 148.6363688457942942, -1.892951199575521937 ) ) ;
#41251 = CARTESIAN_POINT ( 'NONE',  ( 4.814721792459936367, 117.6728147345521336, -0.9185617900964898608 ) ) ;
#41252 = CARTESIAN_POINT ( 'NONE',  ( 2.481140172163616153, 107.2306503360107541, 4.727365043318366489 ) ) ;
#41253 = EDGE_CURVE ( 'NONE', #26546, #21011, #22902, .T. ) ;
#41254 = CARTESIAN_POINT ( 'NONE',  ( -15.79259660498981788, 146.2429432508320417, -0.1870566092231161215 ) ) ;
#41255 = CARTESIAN_POINT ( 'NONE',  ( -17.42401203395167286, 135.4862447717955547, -2.417378365323842537 ) ) ;
#41256 = CARTESIAN_POINT ( 'NONE',  ( 6.174787192795118784, -14.39888150296345160, 1.159817306988995211 ) ) ;
#41257 = CARTESIAN_POINT ( 'NONE',  ( -6.442660433036017764, 29.32943145771791649, -0.01012415147099491285 ) ) ;
#41258 = VECTOR ( 'NONE', #30850, 1000.000000000000114 ) ;
#41259 = CARTESIAN_POINT ( 'NONE',  ( -41.97746338594183868, 23.60773098774231826, -1.524000000000005794 ) ) ;
#41261 = VERTEX_POINT ( 'NONE', #2422 ) ;
#41260 = AXIS2_PLACEMENT_3D ( 'NONE', #20550, #23542, #3992 ) ;
#41262 = CARTESIAN_POINT ( 'NONE',  ( 18.66896445097598445, 144.8948545501563103, 2.490227693099508421 ) ) ;
#41263 = AXIS2_PLACEMENT_3D ( 'NONE', #27068, #39650, #26857 ) ;
#41264 = FILL_AREA_STYLE_COLOUR ( '', #22212 ) ;
#41265 = ADVANCED_FACE ( 'NONE', ( #31793 ), #77, .T. ) ;
#41266 = CARTESIAN_POINT ( 'NONE',  ( -10.12396263145945419, 65.41168055974398499, -1.523999999999996247 ) ) ;
#41267 = CARTESIAN_POINT ( 'NONE',  ( -0.1065646865916159008, 105.8844662015456777, 5.332932678536313809 ) ) ;
#41268 = EDGE_CURVE ( 'NONE', #27998, #18952, #19113, .T. ) ;
#41269 = CARTESIAN_POINT ( 'NONE',  ( 7.448509604456053701, -5.047432113992361025, -3.928768625439613693 ) ) ;
#41270 = CARTESIAN_POINT ( 'NONE',  ( -0.004350076772803485731, 120.7058980590201429, 0.2176956299261764427 ) ) ;
#41271 = CARTESIAN_POINT ( 'NONE',  ( -6.618965589514436111E-14, 97.88346620154572975, 1.207165459396359365E-19 ) ) ;
#41272 = CARTESIAN_POINT ( 'NONE',  ( 11.41934419072014784, 118.9229013597968247, -0.3849275771520423439 ) ) ;
#41273 = CARTESIAN_POINT ( 'NONE',  ( 6.059261036834405978, 57.14999999999999858, -5.016499999999999737 ) ) ;
#41274 = CARTESIAN_POINT ( 'NONE',  ( -58.30016403521963042, -0.1443550006728371859, 0.3367957002666301380 ) ) ;
#41275 = CARTESIAN_POINT ( 'NONE',  ( -8.797619116256065297, 117.6845724412130636, -0.1949819775001481181 ) ) ;
#41276 = CARTESIAN_POINT ( 'NONE',  ( -5.078986093043185157, 66.64146620154573952, -0.1014902294541238092 ) ) ;
#41277 = CARTESIAN_POINT ( 'NONE',  ( -4.269871265972513541, 118.2237297664921272, 0.2881146102117009833 ) ) ;
#41278 = CARTESIAN_POINT ( 'NONE',  ( -22.76738278397264281, 137.3906169244638136, -0.4549464913834381230 ) ) ;
#41279 = ORIENTED_EDGE ( 'NONE', *, *, #36137, .F. ) ;
#41280 = CARTESIAN_POINT ( 'NONE',  ( -50.29507671575587580, 15.72791930032350827, 4.796563717952097683 ) ) ;
#41281 = CARTESIAN_POINT ( 'NONE',  ( -8.272338380459794749, 120.1238670769245402, -1.449810942576005290 ) ) ;
#41282 = CARTESIAN_POINT ( 'NONE',  ( -4.559649833866270541, 116.0444662015457169, -3.750543233647261498 ) ) ;
#41283 = AXIS2_PLACEMENT_3D ( 'NONE', #39374, #5959, #18918 ) ;
#41284 = CARTESIAN_POINT ( 'NONE',  ( -6.480921187770144698, 121.5572409441427482, -0.5803991303062125962 ) ) ;
#41285 = B_SPLINE_CURVE_WITH_KNOTS ( 'NONE', 5,
 ( #552, #3538, #10325, #29710, #26728, #19902, #16705, #17129 ),
 .UNSPECIFIED., .F., .F.,
 ( 6, 2, 6 ),
 ( 0.000000000000000000, 0.0004921095964230317449, 0.0009842191928460634898 ),
 .UNSPECIFIED. ) ;
#41286 = DIRECTION ( 'NONE',  ( -0.9816537812491077375, -0.1906721105965137331, 6.205370029530848928E-16 ) ) ;
#41287 = CARTESIAN_POINT ( 'NONE',  ( 6.113380087472956159E-17, 0.6350000000000001199, 0.000000000000000000 ) ) ;
#41288 = EDGE_LOOP ( 'NONE', ( #35289, #25877, #30558, #29369 ) ) ;
#41289 = CARTESIAN_POINT ( 'NONE',  ( 4.537321141924904211, 26.63107350737006840, 0.8823464973398146283 ) ) ;
#41290 = CARTESIAN_POINT ( 'NONE',  ( -30.15519950990045572, 69.97033940222175374, 1.269999999999991358 ) ) ;
#41291 = CYLINDRICAL_SURFACE ( 'NONE', #39867, 0.6350000000000001199 ) ;
#41292 = CARTESIAN_POINT ( 'NONE',  ( -42.22422426686605945, 22.06987237837733673, 1.558155077124570242 ) ) ;
#41293 = TOROIDAL_SURFACE ( 'NONE', #15422, 3.683000000000000718, 0.5080000000000000071 ) ;
#41294 = DIRECTION ( 'NONE',  ( -1.000000000000000000, -6.353134868986659519E-16, 6.146657985744592735E-16 ) ) ;
#41295 = CARTESIAN_POINT ( 'NONE',  ( -6.065156332796640015, 121.4250553548456963, 0.04358041984482485115 ) ) ;
#41296 = CARTESIAN_POINT ( 'NONE',  ( -3.182929088426432074, 26.46582164074821009, -3.363547984189534379 ) ) ;
#41297 = CARTESIAN_POINT ( 'NONE',  ( 16.30933243092136919, 122.7783120765077030, 1.207982166786797373 ) ) ;
#41298 = CARTESIAN_POINT ( 'NONE',  ( -24.57769139521899149, 76.70147894597536720, 1.523999999999993804 ) ) ;
#41300 = CARTESIAN_POINT ( 'NONE',  ( 21.59954917983685263, 148.3057046726078170, -1.384394358321686447 ) ) ;
#41299 = CARTESIAN_POINT ( 'NONE',  ( 2.101618670382315646, -15.21789252882688182, 5.187277112784037136 ) ) ;
#41301 = CARTESIAN_POINT ( 'NONE',  ( -17.48755558824501932, 140.3598469681121514, 1.687825538285184779 ) ) ;
#41302 = CARTESIAN_POINT ( 'NONE',  ( -0.8806307086779237014, 20.21867702141905099, 4.540528814573361771 ) ) ;
#41303 = CARTESIAN_POINT ( 'NONE',  ( -22.58684024723483930, 150.0155710288180444, -1.417619447182237424 ) ) ;
#41304 = CARTESIAN_POINT ( 'NONE',  ( -0.5928395319016861453, 6.288998576159460008, -0.7801151024821093571 ) ) ;
#41305 = ORIENTED_EDGE ( 'NONE', *, *, #16531, .T. ) ;
#41306 = CARTESIAN_POINT ( 'NONE',  ( -56.90807066679607829, 2.849439543264234320, 1.873271221587421653 ) ) ;
#41307 = CARTESIAN_POINT ( 'NONE',  ( -15.78585801821222745, 147.2673792861271522, 0.2768292828507334935 ) ) ;
#41308 = CARTESIAN_POINT ( 'NONE',  ( 5.728675787863017455, -12.92793046001887447, 1.911514839944304045 ) ) ;
#41309 = CARTESIAN_POINT ( 'NONE',  ( 0.007600002268302612565, 120.2037396364829505, -0.3803351912374558497 ) ) ;
#41310 = ORIENTED_EDGE ( 'NONE', *, *, #18348, .F. ) ;
#41311 = CARTESIAN_POINT ( 'NONE',  ( 2.437877199975485798, 115.7029724319875044, 1.698779354361399596 ) ) ;
#41312 = CIRCLE ( 'NONE', #15443, 6.350000000000004974 ) ;
#41313 = ORIENTED_EDGE ( 'NONE', *, *, #363, .T. ) ;
#41314 = CARTESIAN_POINT ( 'NONE',  ( -4.811753004953239987, 117.8278766848995360, -0.8913836744279551860 ) ) ;
#41315 = CARTESIAN_POINT ( 'NONE',  ( 15.72550100231850223, 145.6881679641610674, 0.3142329346387552902 ) ) ;
#41316 = ORIENTED_EDGE ( 'NONE', *, *, #5566, .F. ) ;
#41317 = CARTESIAN_POINT ( 'NONE',  ( 16.37183938475173761, 128.5611466799914240, 2.176631273311136372 ) ) ;
#41318 = CARTESIAN_POINT ( 'NONE',  ( 2.884051542275651414, 156.0957788938021054, 0.05763021347587640730 ) ) ;
#41319 = AXIS2_PLACEMENT_3D ( 'NONE', #10350, #20757, #27164 ) ;
#41320 = CARTESIAN_POINT ( 'NONE',  ( 5.579075174912572876, 56.51499999999997925, 4.418274828058815551 ) ) ;
#41321 = EDGE_CURVE ( 'NONE', #40883, #20726, #35713, .T. ) ;
#41322 = CARTESIAN_POINT ( 'NONE',  ( 0.006534791579796636780, 156.3267223255430167, -0.3270276925529294054 ) ) ;
#41323 = TOROIDAL_SURFACE ( 'NONE', #19525, 0.7620000000000000107, 0.2540000000000000036 ) ;
#41324 = CARTESIAN_POINT ( 'NONE',  ( 3.277668934457457883, 159.4655167044000166, -0.1355973003551878275 ) ) ;
#41325 = CARTESIAN_POINT ( 'NONE',  ( 6.059261036834400649, 64.39150124418100063, -5.016499999999999737 ) ) ;
#41326 = CARTESIAN_POINT ( 'NONE',  ( -11.32678463655001266, 56.02547433970818958, 4.456118031212522368 ) ) ;
#41327 = CARTESIAN_POINT ( 'NONE',  ( -46.68395179480138069, 26.03198510454123848, 1.396999999999990250 ) ) ;
#41328 = CARTESIAN_POINT ( 'NONE',  ( 2.060994295209965355, -15.07716207348598658, 5.759911643239397527 ) ) ;
#41329 = CARTESIAN_POINT ( 'NONE',  ( -46.89970385779243855, 22.02655025333852379, 4.237790764466920379 ) ) ;
#41330 = DIRECTION ( 'NONE',  ( -1.000000000000000000, 0.000000000000000000, 0.000000000000000000 ) ) ;
#41331 = CARTESIAN_POINT ( 'NONE',  ( -4.804031589438218397, 117.8804387572236720, 0.6820340777931721554 ) ) ;
#41332 = ORIENTED_EDGE ( 'NONE', *, *, #33876, .T. ) ;
#41333 = ORIENTED_EDGE ( 'NONE', *, *, #40646, .T. ) ;
#41334 = FACE_OUTER_BOUND ( 'NONE', #20021, .T. ) ;
#41335 = CARTESIAN_POINT ( 'NONE',  ( -8.556729359846826810, 118.7615713437664482, -1.197783989955824246 ) ) ;
#41336 = CARTESIAN_POINT ( 'NONE',  ( -6.647360066588118066, 123.1390089711370166, -0.2039998645198904670 ) ) ;
#41337 = CARTESIAN_POINT ( 'NONE',  ( 4.844883236810956006, 117.7536488614241819, 0.9521362604971945753 ) ) ;
#41338 = CARTESIAN_POINT ( 'NONE',  ( 3.131015516031846690, -14.62848841321586946, 3.524024012273756501 ) ) ;
#41339 = CARTESIAN_POINT ( 'NONE',  ( -0.7761819157718372608, 120.0979018405971175, 0.5779541898223676810 ) ) ;
#41340 = AXIS2_PLACEMENT_3D ( 'NONE', #396, #13363, #18376 ) ;
#41341 = CARTESIAN_POINT ( 'NONE',  ( 2.862861873098513588, -10.07698056833738320, -3.640125809621840069 ) ) ;
#41342 = CARTESIAN_POINT ( 'NONE',  ( -10.75478607932181241, 82.07015292912137738, -1.523999999999999355 ) ) ;
#41343 = CARTESIAN_POINT ( 'NONE',  ( -5.586884702347497900, 130.0144662015457300, -0.1116392523995361624 ) ) ;
#41344 = CARTESIAN_POINT ( 'NONE',  ( 3.187032726610941946, -14.26951854355915117, 4.096494115788091861 ) ) ;
#41345 = CARTESIAN_POINT ( 'NONE',  ( 5.736215069875311379, 118.4654530710369329, -0.4324765805296820753 ) ) ;
#41346 = CARTESIAN_POINT ( 'NONE',  ( -8.120140396194459598, 121.3802920439979118, -1.244985559442681078 ) ) ;
#41347 = CARTESIAN_POINT ( 'NONE',  ( -48.28978369826177186, 19.63653578263565436, 5.206999999995388428 ) ) ;
#41348 = PLANE ( 'NONE',  #3365 ) ;
#41349 = CARTESIAN_POINT ( 'NONE',  ( -0.7744676708938487142, 115.7029696127382579, 1.727560791094020720 ) ) ;
#41350 = CARTESIAN_POINT ( 'NONE',  ( -3.234384296441582318, 11.31316835407710819, -3.315160845070126427 ) ) ;
#41352 = ORIENTED_EDGE ( 'NONE', *, *, #15989, .F. ) ;
#41351 = CARTESIAN_POINT ( 'NONE',  ( 16.70755423740138568, 155.2649736186859570, 0.8698744534657081307 ) ) ;
#41353 = CARTESIAN_POINT ( 'NONE',  ( 1.939419507827386813, 104.6144662015435927, -4.972011625062160434 ) ) ;
#41354 = CARTESIAN_POINT ( 'NONE',  ( 4.433333709997448580, -15.52846643035468688, 1.874498299855786421 ) ) ;
#41355 = CARTESIAN_POINT ( 'NONE',  ( -12.45504352496370792, 122.8403290575659526, 1.325700600460794742 ) ) ;
#41356 = CARTESIAN_POINT ( 'NONE',  ( -0.7739057699295280868, 27.87760190725158083, 0.5882008851359883383 ) ) ;
#41357 = CARTESIAN_POINT ( 'NONE',  ( 0.3789452347801735566, 6.767153838948093636, 0.8990310622920915096 ) ) ;
#41358 = ORIENTED_EDGE ( 'NONE', *, *, #23354, .F. ) ;
#41359 = ORIENTED_EDGE ( 'NONE', *, *, #13430, .T. ) ;
#41360 = CARTESIAN_POINT ( 'NONE',  ( -4.963705370159209984, 117.4628516566523047, -0.9731298996446248184 ) ) ;
#41361 = CARTESIAN_POINT ( 'NONE',  ( 3.552294876605459173, 120.2162445758188056, 0.4839898749706283976 ) ) ;
#41362 = CARTESIAN_POINT ( 'NONE',  ( -16.50777979357284408, 146.8700648836752691, 0.9466601202970256201 ) ) ;
#41363 = CARTESIAN_POINT ( 'NONE',  ( -8.487687333566288572, 123.3253871723413368, -0.1696041924978711757 ) ) ;
#41364 = CARTESIAN_POINT ( 'NONE',  ( 3.350179296191433398, -14.02378440268806159, 3.677192885962260682 ) ) ;
#41365 = CARTESIAN_POINT ( 'NONE',  ( 0.9105297513473562532, 157.1001331247151143, -1.431354397858309646 ) ) ;
#41366 = CARTESIAN_POINT ( 'NONE',  ( -19.54281269640877028, 149.4594839399872512, -2.484111515072796816 ) ) ;
#41367 = CARTESIAN_POINT ( 'NONE',  ( 4.795219958910193370, 117.6022194698829679, -0.9837822912906766248 ) ) ;
#41368 = CARTESIAN_POINT ( 'NONE',  ( 3.092642723064080279, -14.67800799544728285, 3.675123631970977911 ) ) ;
#41369 = CARTESIAN_POINT ( 'NONE',  ( 4.074910602682932925, 118.2429491485453354, -0.1454311599470142491 ) ) ;
#41370 = CARTESIAN_POINT ( 'NONE',  ( 10.49519746661477804, 153.0637448873655728, -0.1985316654307168194 ) ) ;
#41371 = ORIENTED_EDGE ( 'NONE', *, *, #22807, .F. ) ;
#41372 = CARTESIAN_POINT ( 'NONE',  ( 4.986952782468003775, 117.3993836136630904, 0.9005337760477702957 ) ) ;
#41373 = DIRECTION ( 'NONE',  ( -0.8745520943968250194, 0.4849315768086535638, -6.829619984160625506E-16 ) ) ;
#41374 =( BOUNDED_SURFACE ( )  B_SPLINE_SURFACE ( 3, 2, ( 
 ( #18086, #1930, #18711 ),
 ( #5543, #27892, #8936 ),
 ( #31721, #37698, #8520 ),
 ( #32554, #29361, #13384 ),
 ( #22730, #23152, #199 ),
 ( #22524, #2972, #16139 ),
 ( #26372, #16786, #36189 ),
 ( #35761, #6788, #6576 ),
 ( #39380, #19544, #19977 ),
 ( #415, #10183, #38955 ),
 ( #29581, #19754, #9765 ),
 ( #32346, #9970, #627 ) ),
 .UNSPECIFIED., .F., .F., .T. ) 
 B_SPLINE_SURFACE_WITH_KNOTS ( ( 4, 2, 2, 2, 2, 4 ),
 ( 3, 3 ),
 ( -1.344410693882025498E-17, 0.0001838632285168812104, 0.0003677264570337758650, 0.0007354529140675651741, 0.001103179371101354429, 0.001470905828135143792 ),
 ( 0.000000000000000000, 1.000000000000000000 ),
 .UNSPECIFIED. ) 
 GEOMETRIC_REPRESENTATION_ITEM ( )  RATIONAL_B_SPLINE_SURFACE ( (
 ( 1.000000000000000000, 0.7071067811865514585, 1.000000000000000000),
 ( 1.000000000000000000, 0.7071067811865514585, 1.000000000000000000),
 ( 1.000000000000000000, 0.7071067811865436870, 1.000000000000000000),
 ( 1.000000000000000000, 0.7071067811865436870, 1.000000000000000000),
 ( 1.000000000000000000, 0.7071067811865436870, 1.000000000000000000),
 ( 1.000000000000000000, 0.7071067811865436870, 1.000000000000000000),
 ( 1.000000000000000000, 0.7071067811865514585, 1.000000000000000000),
 ( 1.000000000000000000, 0.7071067811865514585, 1.000000000000000000),
 ( 1.000000000000000000, 0.7071067811865514585, 1.000000000000000000),
 ( 1.000000000000000000, 0.7071067811865514585, 1.000000000000000000),
 ( 1.000000000000000000, 0.7071067811865514585, 1.000000000000000000),
 ( 1.000000000000000000, 0.7071067811865514585, 1.000000000000000000) ) ) 
 REPRESENTATION_ITEM ( '' )  SURFACE ( )  );
#41375 = CARTESIAN_POINT ( 'NONE',  ( 5.010381036134592847, 117.3993854210250447, 0.7490851615034684885 ) ) ;
#41376 = CARTESIAN_POINT ( 'NONE',  ( -50.04979780823212820, 16.23027998584070275, 4.918765685678885724 ) ) ;
#41377 = CARTESIAN_POINT ( 'NONE',  ( 6.371402057089752269, 24.08812572624405135, -5.527521448792488634 ) ) ;
#41378 = CARTESIAN_POINT ( 'NONE',  ( 3.522522545432599017, 120.3814187630814132, 0.6186928868410388471 ) ) ;
#41379 = DIRECTION ( 'NONE',  ( -1.000000000000000000, 0.000000000000000000, 0.000000000000000000 ) ) ;
#41380 = CARTESIAN_POINT ( 'NONE',  ( 16.27668397883899232, 121.4070763266325628, 0.2738251655545990149 ) ) ;
#41381 = CARTESIAN_POINT ( 'NONE',  ( -5.461839458676769787, 117.5340897209903517, 0.6076615112082689452 ) ) ;
#41382 = STYLED_ITEM ( 'NONE', ( #24210 ), #10787 ) ;
#41383 = CARTESIAN_POINT ( 'NONE',  ( -2.395914033174281865, 1.367755174955888275, -3.957843245732672877 ) ) ;
#41384 = CARTESIAN_POINT ( 'NONE',  ( 15.72385166996613570, 146.8976323831864477, 0.3141999770531622160 ) ) ;
#41385 = CARTESIAN_POINT ( 'NONE',  ( 7.953355231451894269, -5.272462086923463076, -2.798479926915725891 ) ) ;
#41386 = CARTESIAN_POINT ( 'NONE',  ( -57.40070531792823516, 1.672101763895803117, -0.9705777051858199833 ) ) ;
#41387 = CARTESIAN_POINT ( 'NONE',  ( 2.156070218774666092, 116.4399559780022884, -0.2666908309453368542 ) ) ;
#41388 = CARTESIAN_POINT ( 'NONE',  ( 0.1065646865915095692, 105.8844662015456919, -5.332932678536313809 ) ) ;
#41389 = CARTESIAN_POINT ( 'NONE',  ( -19.15923810799328209, 79.68098548105338352, -1.524000000000003352 ) ) ;
#41390 = CARTESIAN_POINT ( 'NONE',  ( -0.2616981356411249848, 38.12352966651759090, 1.602708108658221553 ) ) ;
#41391 = CARTESIAN_POINT ( 'NONE',  ( 5.678980076864418969, -10.27674996446047828, -6.244917620322217644 ) ) ;
#41392 = CARTESIAN_POINT ( 'NONE',  ( 0.1786959197596161841, 117.9394491163083387, 1.410396274712311548 ) ) ;
#41393 = DIRECTION ( 'NONE',  ( -0.8745520943968236871, 0.4849315768086559508, -6.829619984160659032E-16 ) ) ;
#41394 = CARTESIAN_POINT ( 'NONE',  ( 3.682264917456192777, 85.18346620154574111, 0.07358041635424013294 ) ) ;
#41395 = CARTESIAN_POINT ( 'NONE',  ( 1.012635771704780252, 123.9312678891798640, -0.06995516121779309093 ) ) ;
#41396 = CARTESIAN_POINT ( 'NONE',  ( -3.247806582137030773, 159.4494809562368971, 0.3030341850868441544 ) ) ;
#41397 = VERTEX_POINT ( 'NONE', #19530 ) ;
#41398 = CARTESIAN_POINT ( 'NONE',  ( -58.29256068059346063, 1.279866164410503604, -0.9167068831667845030 ) ) ;
#41399 = EDGE_LOOP ( 'NONE', ( #33286, #5957, #34519, #23253 ) ) ;
#41400 = CARTESIAN_POINT ( 'NONE',  ( -42.32312746590514507, 22.34068395104271332, -1.752427511502158364 ) ) ;
#41401 = CARTESIAN_POINT ( 'NONE',  ( -10.95295744368173985, 127.9616006207616152, -0.1130554581393018038 ) ) ;
#41402 = CARTESIAN_POINT ( 'NONE',  ( 5.208953926857062378, -15.24612122244077561, 3.266433406317167165 ) ) ;
#41403 = CARTESIAN_POINT ( 'NONE',  ( -20.59420924110326823, 148.8605967840894095, 1.615102827552612252 ) ) ;
#41404 = CARTESIAN_POINT ( 'NONE',  ( 14.85424080674754244, 121.7713424311148032, -0.8456621969668064454 ) ) ;
#41405 = CARTESIAN_POINT ( 'NONE',  ( -4.460028654926622593, 22.53297844546955631, 1.214995109042491528 ) ) ;
#41406 = CARTESIAN_POINT ( 'NONE',  ( -20.61342602778661970, 152.5829384802601396, -0.8505107393516943004 ) ) ;
#41407 = CARTESIAN_POINT ( 'NONE',  ( -56.64692619791329520, 3.940143260488348176, -2.419031359405692250 ) ) ;
#41408 = ORIENTED_EDGE ( 'NONE', *, *, #31595, .T. ) ;
#41409 = CARTESIAN_POINT ( 'NONE',  ( -0.0002200197270987085075, 124.8375573595198063, 0.01101068683960104017 ) ) ;
#41410 = DIRECTION ( 'NONE',  ( -0.9998004120163609398, 0.000000000000000000, -0.01997839162482749689 ) ) ;
#41411 = CARTESIAN_POINT ( 'NONE',  ( -13.59099248324878850, 128.5255724691869830, 1.296117023882649155 ) ) ;
#41412 = CARTESIAN_POINT ( 'NONE',  ( -54.16325525233833815, 8.500792493645910497, -3.386179713691846782 ) ) ;
#41413 = AXIS2_PLACEMENT_3D ( 'NONE', #32997, #9557, #32557 ) ;
#41414 = CARTESIAN_POINT ( 'NONE',  ( 17.77426102521089035, 149.9241642446907292, -1.728420094174573096 ) ) ;
#41415 = CARTESIAN_POINT ( 'NONE',  ( -19.90801791207606897, 136.1824594150436383, -2.220825683169745712 ) ) ;
#41416 = CARTESIAN_POINT ( 'NONE',  ( -49.39021242113546606, 17.77731941784099234, -5.290631085210052653 ) ) ;
#41417 = CARTESIAN_POINT ( 'NONE',  ( 9.963230294258153208, 124.0638329749226330, -0.5989708749582570713 ) ) ;
#41418 = ORIENTED_EDGE ( 'NONE', *, *, #4040, .F. ) ;
#41419 = CARTESIAN_POINT ( 'NONE',  ( -17.72773402338109605, 148.0643276405518804, -2.286219595833943963 ) ) ;
#41420 = CARTESIAN_POINT ( 'NONE',  ( 4.512298201359578265, -15.31825885905126228, -0.4677400858729020006 ) ) ;
#41421 = EDGE_CURVE ( 'NONE', #1422, #359, #36238, .T. ) ;
#41422 = ADVANCED_FACE ( 'NONE', ( #183 ), #31894, .T. ) ;
#41423 = CARTESIAN_POINT ( 'NONE',  ( -58.87911280034276018, -0.2081424763510641984, -1.061797465414398100E-14 ) ) ;
#41424 = CARTESIAN_POINT ( 'NONE',  ( -4.869895933236811025, 117.5471251575243912, 0.9485355776679378348 ) ) ;
#41425 = CARTESIAN_POINT ( 'NONE',  ( 5.836546232834177061, 120.2771794157441008, 1.045480238269852702 ) ) ;
#41426 = CARTESIAN_POINT ( 'NONE',  ( 2.912792906754999578, 38.59631781016217644, -1.173005823891349442 ) ) ;
#41427 = CARTESIAN_POINT ( 'NONE',  ( -7.020956707233273697, 3.738713905105897517, 4.673168047251142099 ) ) ;
#41428 = CARTESIAN_POINT ( 'NONE',  ( 8.617107517140063067, 123.3364012560002578, 0.3915851211929423648 ) ) ;
#41429 = CARTESIAN_POINT ( 'NONE',  ( -29.89586364642802963, 71.55302121702176521, -1.270000000000007345 ) ) ;
#41430 = TOROIDAL_SURFACE ( 'NONE', #4043, 0.3809999999999999498, 0.2540000000000000036 ) ;
#41432 = VERTEX_POINT ( 'NONE', #7616 ) ;
#41431 = CARTESIAN_POINT ( 'NONE',  ( -41.36952270831616119, 22.75442529069328401, -0.6632742133606294166 ) ) ;
#41433 = DIRECTION ( 'NONE',  ( 5.188838149069472160E-16, -1.699382548006136559E-16, -1.000000000000000000 ) ) ;
#41434 = TOROIDAL_SURFACE ( 'NONE', #28505, 8.794749999999996959, 0.2540000000000000036 ) ;
#41435 = CARTESIAN_POINT ( 'NONE',  ( -57.50953982388014651, 1.662011999372992044, 1.631050346940570384 ) ) ;
#41436 = CARTESIAN_POINT ( 'NONE',  ( -52.00466655731695909, 12.92300787752876801, 4.416453009321314127 ) ) ;
#41437 = CARTESIAN_POINT ( 'NONE',  ( 3.160389755237984044, 118.7629491485453741, 1.175221893788974015 ) ) ;
#41438 = DIRECTION ( 'NONE',  ( 4.017660918040594346E-17, -1.000000000000000000, -2.376309959284834438E-19 ) ) ;
#41439 = CARTESIAN_POINT ( 'NONE',  ( -51.02231935970569054, 20.76374992004582154, 0.7877321375940166126 ) ) ;
#41440 = CARTESIAN_POINT ( 'NONE',  ( -22.52215935351600251, 150.7865899205276321, -0.2217371156544977739 ) ) ;
#41441 = ORIENTED_EDGE ( 'NONE', *, *, #34197, .T. ) ;
#41442 = CARTESIAN_POINT ( 'NONE',  ( -50.22242355904485578, 22.76272800790864181, -0.3424289802766569690 ) ) ;
#41443 = CARTESIAN_POINT ( 'NONE',  ( 7.806368754331440840, 122.5465026837492672, -0.09257337652142975937 ) ) ;
#41444 = DIRECTION ( 'NONE',  ( -5.188838149069471174E-16, 1.699382548006136313E-16, 1.000000000000000000 ) ) ;
#41445 = EDGE_LOOP ( 'NONE', ( #30364, #14543 ) ) ;
#41446 = CARTESIAN_POINT ( 'NONE',  ( 0.6753195804803343583, 115.7031287183464769, -1.734273028809747208 ) ) ;
#41447 = CARTESIAN_POINT ( 'NONE',  ( -9.171413160121694830, 124.0935018032023436, -0.3437271393031030575 ) ) ;
#41448 = CARTESIAN_POINT ( 'NONE',  ( 3.373230072307711325, -14.96631539557509427, 5.513067843180951222 ) ) ;
#41449 = CARTESIAN_POINT ( 'NONE',  ( -0.4065252312485121977, 117.6538564835029206, 0.4930844833531826676 ) ) ;
#41450 = CARTESIAN_POINT ( 'NONE',  ( -6.606344270946872901E-14, 95.34346620154573770, 1.014423412895214384E-29 ) ) ;
#41451 = CARTESIAN_POINT ( 'NONE',  ( 3.748677658115056044, 116.6824454826851820, 0.2320358872840704023 ) ) ;
#41452 = CARTESIAN_POINT ( 'NONE',  ( -0.001427378018337739293, 156.3034662015458593, 0.07143183283045266563 ) ) ;
#41453 = CARTESIAN_POINT ( 'NONE',  ( -4.997976212577941446, 117.5941873918911256, 0.6211058249704617396 ) ) ;
#41454 = CARTESIAN_POINT ( 'NONE',  ( 0.8051319862491574941, 7.640635046448309708, 0.5515409728216702501 ) ) ;
#41455 = EDGE_CURVE ( 'NONE', #35910, #31840, #29769, .T. ) ;
#41456 = CARTESIAN_POINT ( 'NONE',  ( -0.2977815589729818080, 116.4565202671238069, -0.07303518451646368037 ) ) ;
#41457 = DIRECTION ( 'NONE',  ( -1.000000000000000000, -9.299908063537918137E-16, 0.000000000000000000 ) ) ;
#41458 = DIRECTION ( 'NONE',  ( -0.6559537821943243197, 0.7548010569845282625, -8.537024980200743918E-16 ) ) ;
#41459 = ORIENTED_EDGE ( 'NONE', *, *, #18079, .T. ) ;
#41460 = CARTESIAN_POINT ( 'NONE',  ( -8.440481546668859636, 119.5496565118663028, 1.072135216671611380 ) ) ;
#41461 = CARTESIAN_POINT ( 'NONE',  ( -1.404924415901314561, -12.60368214249519703, -4.422195601339041993 ) ) ;
#41462 = CARTESIAN_POINT ( 'NONE',  ( -0.02615207601228607126, 159.0391464308674756, 1.308756824028193266 ) ) ;
#41463 = CARTESIAN_POINT ( 'NONE',  ( 11.27973791692641470, 156.1341193432522800, -1.681596738997434670 ) ) ;
#41464 = CARTESIAN_POINT ( 'NONE',  ( 3.793251108634954516, -14.54000584982637001, -2.652246991476435056 ) ) ;
#41465 = CARTESIAN_POINT ( 'NONE',  ( -17.05973152613374211, 125.2153959547233910, -1.608365543201426551 ) ) ;
#41466 = CARTESIAN_POINT ( 'NONE',  ( 4.782691188464728960, 117.8918938667789718, -0.7200855588195160806 ) ) ;
#41467 = CARTESIAN_POINT ( 'NONE',  ( 5.148946675963925301, 115.4673366222922368, 1.510641186666999980 ) ) ;
#41468 = CARTESIAN_POINT ( 'NONE',  ( -15.73072674608061483, 146.8994026175788008, -0.1860059585639195767 ) ) ;
#41469 = CARTESIAN_POINT ( 'NONE',  ( -2.337245495867256828, 157.7073581658784178, -1.721377379916720907 ) ) ;
#41471 = CARTESIAN_POINT ( 'NONE',  ( 5.218378134725943696, -15.03467804911627681, 3.623131781705042354 ) ) ;
#41470 = CIRCLE ( 'NONE', #27851, 2.285999999999998700 ) ;
#41472 = CIRCLE ( 'NONE', #36693, 8.794749999999993406 ) ;
#41473 = PLANE ( 'NONE',  #7060 ) ;
#41474 = EDGE_CURVE ( 'NONE', #4116, #26517, #20875, .T. ) ;
#41475 = CARTESIAN_POINT ( 'NONE',  ( -0.9713960331287118111, 118.1651005049585024, -0.8791694678672022922 ) ) ;
#41476 = ORIENTED_EDGE ( 'NONE', *, *, #2434, .F. ) ;
#41477 = CARTESIAN_POINT ( 'NONE',  ( 18.07722773961200602, 140.6071502257508143, 2.476399831607924540 ) ) ;
#41478 = LINE ( 'NONE', #2294, #16787 ) ;
#41479 = PLANE ( 'NONE',  #34792 ) ;
#41480 = CARTESIAN_POINT ( 'NONE',  ( -1.667199326422704297, 119.8612358676174949, 0.5251152081720656950 ) ) ;
#41481 = CARTESIAN_POINT ( 'NONE',  ( 1.876134371277577761, -7.842104223405461205, 8.241158351834352302 ) ) ;
#41482 = CARTESIAN_POINT ( 'NONE',  ( 9.255566420661640592, 123.6186430441458981, 0.7743267827205287945 ) ) ;
#41483 = ADVANCED_FACE ( 'NONE', ( #39358 ), #33195, .T. ) ;
#41484 = CARTESIAN_POINT ( 'NONE',  ( 18.27977197196852543, 154.1370782493726210, -0.5456809356757469365 ) ) ;
#41485 = CARTESIAN_POINT ( 'NONE',  ( 5.638141748396324537, 57.14999999999959357, -5.060111600445807767 ) ) ;
#41486 = CARTESIAN_POINT ( 'NONE',  ( -58.32006471847083873, -0.1868378168976956022, 0.2819915271595720418 ) ) ;
#41487 = CARTESIAN_POINT ( 'NONE',  ( 5.562407744872654547, 116.6996333493932809, 0.1111501445372368169 ) ) ;
#41488 = B_SPLINE_CURVE_WITH_KNOTS ( 'NONE', 3,
 ( #28907, #22496, #25508, #41922, #176, #38508, #13146, #42134, #28493, #25921, #38929, #38300, #5934 ),
 .UNSPECIFIED., .F., .F.,
 ( 4, 1, 1, 1, 1, 1, 1, 1, 1, 1, 4 ),
 ( 0.000000000000000000, 0.1250000000000002498, 0.2500000000000004996, 0.3750000000000000555, 0.4109712969816595729, 0.4999999999999996669, 0.6249999999999995559, 0.7500000000000001110, 0.8232913890944979496, 0.8750000000000001110, 1.000000000000000000 ),
 .UNSPECIFIED. ) ;
#41490 = CARTESIAN_POINT ( 'NONE',  ( -29.82321757229076908, 71.17901112636586447, 1.269999999999992690 ) ) ;
#41489 = CIRCLE ( 'NONE', #12230, 0.2540000000000000036 ) ;
#41491 = CARTESIAN_POINT ( 'NONE',  ( -23.36121599382910219, 148.8756354988261990, -0.4668126921608655722 ) ) ;
#41492 = EDGE_LOOP ( 'NONE', ( #31044, #7336, #15196, #2437 ) ) ;
#41493 = AXIS2_PLACEMENT_3D ( 'NONE', #24826, #31647, #15450 ) ;
#41494 = CARTESIAN_POINT ( 'NONE',  ( -4.406358471284682388, 119.5322704129101794, -0.9262837095330083148 ) ) ;
#41495 = CARTESIAN_POINT ( 'NONE',  ( 4.530977940126489578, 116.0444662015457595, 3.792717828883179543 ) ) ;
#41496 = CARTESIAN_POINT ( 'NONE',  ( -9.322631400391710343, 123.9819092696984910, -0.6064563484049504405 ) ) ;
#41497 = CARTESIAN_POINT ( 'NONE',  ( 4.801338745261147345, 117.3993836135855275, -1.016148444996444189 ) ) ;
#41498 = CARTESIAN_POINT ( 'NONE',  ( 23.36121599382897074, 148.8756354988261990, 0.4668126921608657942 ) ) ;
#41499 = ORIENTED_EDGE ( 'NONE', *, *, #15449, .F. ) ;
#41500 = CARTESIAN_POINT ( 'NONE',  ( 3.043391175932955495, 18.63480288530714191, -3.501419995799015528 ) ) ;
#41501 = EDGE_CURVE ( 'NONE', #6194, #35513, #547, .T. ) ;
#41502 = CARTESIAN_POINT ( 'NONE',  ( -32.57684172203629203, 51.47351799142593620, 1.524000000010915068 ) ) ;
#41503 = CARTESIAN_POINT ( 'NONE',  ( -4.801647862234980302, 117.4032733357427105, 1.015449305853463491 ) ) ;
#41504 = CARTESIAN_POINT ( 'NONE',  ( 6.604684614740960136, 78.82897922428260529, -3.487443616724450468 ) ) ;
#41505 = CARTESIAN_POINT ( 'NONE',  ( -5.639506490940112471, 64.42185452804264401, 1.270000000000005569 ) ) ;
#41506 = CARTESIAN_POINT ( 'NONE',  ( 7.789195200054391144, 122.5918894314571759, 0.3010967474846231173 ) ) ;
#41507 = EDGE_CURVE ( 'NONE', #3540, #5200, #35903, .T. ) ;
#41508 = CARTESIAN_POINT ( 'NONE',  ( 2.794707274389933715, 24.31675177525179876, -3.679445548267922916 ) ) ;
#41509 = CARTESIAN_POINT ( 'NONE',  ( 22.77131365710826572, 149.1304179266472261, 1.534847161028223939 ) ) ;
#41511 = CARTESIAN_POINT ( 'NONE',  ( 21.56827676951018091, 148.6087350971780836, -1.383610176320234864 ) ) ;
#41510 = CARTESIAN_POINT ( 'NONE',  ( 5.115874721082195542, 56.51499999999995083, 4.603382018213770799 ) ) ;
#41512 = CARTESIAN_POINT ( 'NONE',  ( -11.50890483677805420, 122.9335272575421669, 1.234163556480095236 ) ) ;
#41513 = CARTESIAN_POINT ( 'NONE',  ( 0.2779342515209439202, -14.33719732021959636, -0.9356842789569203012 ) ) ;
#41514 = CARTESIAN_POINT ( 'NONE',  ( -19.64956762203127738, 128.7577553591919752, -1.229466013835583516 ) ) ;
#41515 = ADVANCED_FACE ( 'NONE', ( #7405 ), #23640, .T. ) ;
#41516 = CARTESIAN_POINT ( 'NONE',  ( 0.7587898337924254832, 1.856531735440085207, 0.6142162870750064174 ) ) ;
#41517 = ORIENTED_EDGE ( 'NONE', *, *, #9429, .F. ) ;
#41518 = CARTESIAN_POINT ( 'NONE',  ( -55.66968704194594153, 5.419822863896792242, 2.567922718055065445 ) ) ;
#41519 = CARTESIAN_POINT ( 'NONE',  ( -15.74292597311053044, 147.5983985311728759, 0.4089823612135941588 ) ) ;
#41520 = CARTESIAN_POINT ( 'NONE',  ( 5.214050246812039546, -13.77884693253300696, 3.484500232556287269 ) ) ;
#41521 = CARTESIAN_POINT ( 'NONE',  ( 10.16557698404459131, 154.1059161911440469, -1.245122368702753723 ) ) ;
#41522 = ORIENTED_EDGE ( 'NONE', *, *, #40026, .T. ) ;
#41523 = B_SPLINE_CURVE_WITH_KNOTS ( 'NONE', 3,
 ( #20247, #23655, #1109, #14077, #23871, #20671 ),
 .UNSPECIFIED., .F., .F.,
 ( 4, 2, 4 ),
 ( -7.295512719012818938E-06, 0.0003601880853723633683, 0.0007276716834637395352 ),
 .UNSPECIFIED. ) ;
#41524 = DIRECTION ( 'NONE',  ( 5.188838149069472160E-16, -1.699382548006136559E-16, -1.000000000000000000 ) ) ;
#41525 = CARTESIAN_POINT ( 'NONE',  ( -4.724244202807499349, 117.6625551699878827, -1.131988795082268240 ) ) ;
#41526 = CARTESIAN_POINT ( 'NONE',  ( 2.836071964827284297, 121.0300505300837415, 0.05667146733340982373 ) ) ;
#41527 = CIRCLE ( 'NONE', #6822, 0.5080000000000002292 ) ;
#41528 = ORIENTED_EDGE ( 'NONE', *, *, #11578, .T. ) ;
#41529 = CARTESIAN_POINT ( 'NONE',  ( 18.11894642568437774, 135.6759721228443425, 2.431264806327576800 ) ) ;
#41530 = CARTESIAN_POINT ( 'NONE',  ( 9.104209967887914701, 153.9432936505793066, 0.1819237819739444872 ) ) ;
#41531 = CARTESIAN_POINT ( 'NONE',  ( -6.503981220335420706E-14, 66.64146620154573952, -9.408573323119121831E-18 ) ) ;
#41532 = CARTESIAN_POINT ( 'NONE',  ( 4.869448445130315051, 117.5470895026042086, -0.9486559672550266553 ) ) ;
#41533 = CARTESIAN_POINT ( 'NONE',  ( 23.28378132671070944, 148.8247458934765461, 0.01018146431420876089 ) ) ;
#41534 = CARTESIAN_POINT ( 'NONE',  ( 0.1036566276968575451, 106.2435128697216271, -5.187401519901567504 ) ) ;
#41535 = CARTESIAN_POINT ( 'NONE',  ( -11.47253659098475254, 56.76836532675849156, 5.016499999999999737 ) ) ;
#41536 = CARTESIAN_POINT ( 'NONE',  ( -47.09845139715251605, 25.49303147219070098, 0.5484243623142188717 ) ) ;
#41537 = VECTOR ( 'NONE', #10687, 1000.000000000000227 ) ;
#41538 = CARTESIAN_POINT ( 'NONE',  ( 1.688396205330639610, -15.30713883100645667, 5.828064177876307816 ) ) ;
#41539 = CARTESIAN_POINT ( 'NONE',  ( -47.04837031381860157, 23.61299024743492581, 3.054033755318061871 ) ) ;
#41540 = DIRECTION ( 'NONE',  ( 4.017660918040594346E-17, -1.000000000000000000, -2.376309959284834438E-19 ) ) ;
#41541 = CARTESIAN_POINT ( 'NONE',  ( -4.567869538816805353, 118.0323994909192180, 0.6817792069717166781 ) ) ;
#41542 = EDGE_CURVE ( 'NONE', #29748, #41570, #8671, .T. ) ;
#41543 = ORIENTED_EDGE ( 'NONE', *, *, #10758, .F. ) ;
#41544 = FACE_BOUND ( 'NONE', #26619, .T. ) ;
#41545 = CARTESIAN_POINT ( 'NONE',  ( -5.949495757309211541, 119.2098673763693597, -1.265899271510292134 ) ) ;
#41546 = CARTESIAN_POINT ( 'NONE',  ( -0.5964146925941966604, 106.0274289318137306, -5.278528196272315398 ) ) ;
#41548 = CARTESIAN_POINT ( 'NONE',  ( 4.723903736628679795, 117.9428513194235109, 0.8168244294066706601 ) ) ;
#41547 = AXIS2_PLACEMENT_3D ( 'NONE', #29463, #3498, #16457 ) ;
#41549 = FACE_OUTER_BOUND ( 'NONE', #3095, .T. ) ;
#41550 = CARTESIAN_POINT ( 'NONE',  ( -0.3884485718552637690, 122.8649044353670803, 0.2114733659581322922 ) ) ;
#41551 = CARTESIAN_POINT ( 'NONE',  ( 4.560443952884764229, -11.68867000232777542, 0.6947937212093100445 ) ) ;
#41552 = DIRECTION ( 'NONE',  ( 0.9998004120163608288, 0.000000000000000000, 0.01997839162482760791 ) ) ;
#41553 = CARTESIAN_POINT ( 'NONE',  ( 5.078986093043053707, 91.53346620154573543, 0.1014902294541244060 ) ) ;
#41554 = CARTESIAN_POINT ( 'NONE',  ( 6.805961295028007285, 123.7298400107579255, 0.09869924339446559114 ) ) ;
#41555 = CARTESIAN_POINT ( 'NONE',  ( -17.19591734316819753, 148.1877419978735873, -2.150982665507991776 ) ) ;
#41556 = DIRECTION ( 'NONE',  ( -0.01731298258488003436, 0.9998501190848634312, 0.000000000000000000 ) ) ;
#41557 = CARTESIAN_POINT ( 'NONE',  ( -4.639629343391110439, 32.09505926734769332, 4.043355921567692413 ) ) ;
#41558 = CARTESIAN_POINT ( 'NONE',  ( -2.240964803089219970, 115.7026167895974424, 1.621435518166598699 ) ) ;
#41559 = CARTESIAN_POINT ( 'NONE',  ( -0.2480930319908794535, 10.21371511114847053, -4.635561276548324727 ) ) ;
#41561 = VERTEX_POINT ( 'NONE', #14765 ) ;
#41560 = CARTESIAN_POINT ( 'NONE',  ( 20.55326960831561678, 152.5775223076369400, 0.9856637426460335139 ) ) ;
#41562 = CARTESIAN_POINT ( 'NONE',  ( -0.8083810056768732100, 105.1229538481459826, -5.283364377078966889 ) ) ;
#41563 = CARTESIAN_POINT ( 'NONE',  ( 1.834459164715513291, -15.41678468052755413, 5.387059099755636460 ) ) ;
#41564 = CARTESIAN_POINT ( 'NONE',  ( -18.94125265848544970, 149.4003703399637288, 1.737001818219200855 ) ) ;
#41565 = CARTESIAN_POINT ( 'NONE',  ( 0.4978855121113271442, 23.66801414613304289, -0.8366695591092367934 ) ) ;
#41566 = EDGE_CURVE ( 'NONE', #27127, #5804, #35231, .T. ) ;
#41567 = CARTESIAN_POINT ( 'NONE',  ( -0.7518944845272079736, 4.819152178039351142, 0.6255420797857809134 ) ) ;
#41568 = ORIENTED_EDGE ( 'NONE', *, *, #1518, .T. ) ;
#41569 = EDGE_CURVE ( 'NONE', #332, #40156, #30440, .T. ) ;
#41570 = VERTEX_POINT ( 'NONE', #4223 ) ;
#41571 = PLANE ( 'NONE',  #12665 ) ;
#41572 = CARTESIAN_POINT ( 'NONE',  ( 2.616318351458453595, 112.7379566594982663, 2.676765618731040242 ) ) ;
#41573 = CARTESIAN_POINT ( 'NONE',  ( -16.49265603038163519, 146.0252812507985141, 0.9509463687623793682 ) ) ;
#41574 = CARTESIAN_POINT ( 'NONE',  ( -0.03519895178523997636, 115.7029491485446613, 1.761499482104069703 ) ) ;
#41575 = CARTESIAN_POINT ( 'NONE',  ( 3.480220535011376182, -13.66934472092314046, 3.064489479733436106 ) ) ;
#41576 = CARTESIAN_POINT ( 'NONE',  ( 15.94706863659606633, 135.0473088626721392, -1.554726643320764934 ) ) ;
#41577 = CARTESIAN_POINT ( 'NONE',  ( -15.34515231418518155, 125.4902479783272184, -1.998699669873516438 ) ) ;
#41578 = CARTESIAN_POINT ( 'NONE',  ( 4.610436209567292387, 117.9340757871244847, 0.9619774773656434297 ) ) ;
#41579 = CIRCLE ( 'NONE', #8235, 6.985000000000000320 ) ;
#41580 = CARTESIAN_POINT ( 'NONE',  ( 8.314112694112955282, 119.9197418425491435, 1.454013855707701142 ) ) ;
#41581 = CARTESIAN_POINT ( 'NONE',  ( -6.346781410994640993, 30.04503731349425166, 1.591420273447385014 ) ) ;
#41582 = CARTESIAN_POINT ( 'NONE',  ( 15.46148294186153471, 147.8441550597069352, -0.1409636975754417765 ) ) ;
#41583 = VERTEX_POINT ( 'NONE', #30963 ) ;
#41584 = CARTESIAN_POINT ( 'NONE',  ( 3.116451998213339625, -14.00698646007624149, 1.619014592372306716 ) ) ;
#41585 = CARTESIAN_POINT ( 'NONE',  ( -15.70103477329412911, 145.5797129992483292, -0.3137440411564564879 ) ) ;
#41586 = CIRCLE ( 'NONE', #22474, 2.540000000000002256 ) ;
#41587 = CARTESIAN_POINT ( 'NONE',  ( 4.878198950886749152, 117.7629972649382069, 0.7300118938262585289 ) ) ;
#41588 = CARTESIAN_POINT ( 'NONE',  ( -58.68789525397752271, -0.3143212917563475983, 0.3020521592211556916 ) ) ;
#41589 = CARTESIAN_POINT ( 'NONE',  ( -8.411989387141455055, 18.26859176889432490, 0.3690887223902433734 ) ) ;
#41590 = CARTESIAN_POINT ( 'NONE',  ( 1.860601238663017298, 156.5995568990359175, 1.190227115183317697 ) ) ;
#41591 = DIRECTION ( 'NONE',  ( 0.000000000000000000, 0.000000000000000000, 1.000000000000000000 ) ) ;
#41592 = CARTESIAN_POINT ( 'NONE',  ( 18.84845417996773875, 125.3331924886369961, 0.3579177782036730981 ) ) ;
#41593 = CARTESIAN_POINT ( 'NONE',  ( -7.117363349590201338, 122.4243137415680280, -0.03262055675632253432 ) ) ;
#41594 = CARTESIAN_POINT ( 'NONE',  ( -24.24369025645185260, 82.02711331519694227, 1.269999999999992690 ) ) ;
#41595 = CARTESIAN_POINT ( 'NONE',  ( 15.38000172822621536, 147.8312228277220868, 0.3073290368998169431 ) ) ;
#41596 = CARTESIAN_POINT ( 'NONE',  ( 0.09500447679424951775, 1.427469433126556053, 8.421719372511704549 ) ) ;
#41597 = CARTESIAN_POINT ( 'NONE',  ( -5.492508718897443742, 117.1018086211233538, -0.7425764315396081727 ) ) ;
#41598 = CARTESIAN_POINT ( 'NONE',  ( -0.3855071059148542090, 123.1683257372383054, -0.1933446952578522504 ) ) ;
#41599 = LINE ( 'NONE', #42017, #6727 ) ;
#41600 = CARTESIAN_POINT ( 'NONE',  ( -36.43259636504752308, 28.15155085495446485, -1.524000000000003352 ) ) ;
#41601 = AXIS2_PLACEMENT_3D ( 'NONE', #11743, #18542, #41147 ) ;
#41602 = CARTESIAN_POINT ( 'NONE',  ( -5.045332104996713696, -5.333490553104357268, 6.775881858851239947 ) ) ;
#41603 = DIRECTION ( 'NONE',  ( -1.000000000000000000, 1.177520686924251719E-16, 0.000000000000000000 ) ) ;
#41604 = LINE ( 'NONE', #12414, #13058 ) ;
#41605 = CARTESIAN_POINT ( 'NONE',  ( 3.221527947697278904, -14.19553219070161809, 2.775880300951635071 ) ) ;
#41606 = CARTESIAN_POINT ( 'NONE',  ( 0.7593927098682741184, 117.6736730875354766, -1.153084249965024455 ) ) ;
#41607 = CARTESIAN_POINT ( 'NONE',  ( -5.603706277412657144, 159.0849926622337023, 0.4754325247485732819 ) ) ;
#41608 = ORIENTED_EDGE ( 'NONE', *, *, #27318, .T. ) ;
#41609 = DIRECTION ( 'NONE',  ( -0.9816537812491076265, -0.1906721105965138718, -4.769617732184456426E-16 ) ) ;
#41610 = EDGE_CURVE ( 'NONE', #12215, #4082, #16971, .T. ) ;
#41611 = ORIENTED_EDGE ( 'NONE', *, *, #32407, .F. ) ;
#41612 = CARTESIAN_POINT ( 'NONE',  ( -17.64290547347870941, 83.78857423953914463, -1.270000000000003126 ) ) ;
#41613 = CARTESIAN_POINT ( 'NONE',  ( 4.434149479847604880, -15.45467793902401077, 4.427262213160148896 ) ) ;
#41614 = CARTESIAN_POINT ( 'NONE',  ( -2.213227627077626547, 118.1205262787358663, 0.6644466414026561907 ) ) ;
#41615 = CARTESIAN_POINT ( 'NONE',  ( 21.81261666999463955, 141.9756885651356413, -1.158660305423542702 ) ) ;
#41616 = EDGE_CURVE ( 'NONE', #8970, #32222, #1210, .T. ) ;
#41617 = CARTESIAN_POINT ( 'NONE',  ( 2.801506786573456420, 9.139157206818806500, -3.684590140147142368 ) ) ;
#41618 = CARTESIAN_POINT ( 'NONE',  ( -57.59846039800395090, 1.925664279336513296, -1.733923949993310121 ) ) ;
#41619 = ORIENTED_EDGE ( 'NONE', *, *, #22688, .T. ) ;
#41620 = CARTESIAN_POINT ( 'NONE',  ( -0.07831152689652476351, 109.4728569552520838, 3.919029035233729363 ) ) ;
#41621 = DIRECTION ( 'NONE',  ( 4.017660918040594346E-17, -1.000000000000000000, -2.376309959284834438E-19 ) ) ;
#41622 = CARTESIAN_POINT ( 'NONE',  ( -10.73673663838201264, 123.5542795626547417, 1.004701191943994765 ) ) ;
#41623 = DIRECTION ( 'NONE',  ( -5.188838149069472160E-16, 1.699382548006136559E-16, 1.000000000000000000 ) ) ;
#41624 =( BOUNDED_SURFACE ( )  B_SPLINE_SURFACE ( 3, 2, ( 
 ( #6631, #23201, #36236 ),
 ( #29192, #20023, #26211 ),
 ( #19596, #32607, #10024 ),
 ( #16835, #22995, #30248 ),
 ( #37075, #37273, #27479 ),
 ( #29836, #7894, #26851 ),
 ( #14057, #24267, #4084 ),
 ( #7266, #13643, #33464 ),
 ( #39642, #23636, #17460 ),
 ( #17256, #23851, #1090 ),
 ( #24060, #4499, #8093 ),
 ( #30042, #20855, #11282 ),
 ( #33676, #27267, #30665 ),
 ( #882, #30458, #33883 ),
 ( #13852, #27062, #14469 ),
 ( #39858, #4711, #21066 ),
 ( #40069, #10654, #1302 ),
 ( #36655, #17665, #7478 ),
 ( #40488, #1513, #4293 ),
 ( #34091, #4920, #20227 ) ),
 .UNSPECIFIED., .F., .F., .T. ) 
 B_SPLINE_SURFACE_WITH_KNOTS ( ( 4, 2, 2, 2, 2, 2, 2, 2, 2, 4 ),
 ( 3, 3 ),
 ( -3.230922474006803213E-17, 0.0008043537003517264297, 0.001608707400703485169, 0.002413061101055244233, 0.003217414801407002863, 0.004021768501758761494, 0.004826122202110520558, 0.006434829602814037819, 0.009652244404221074076, 0.01286965920562810860 ),
 ( 0.000000000000000000, 1.000000000000000000 ),
 .UNSPECIFIED. ) 
 GEOMETRIC_REPRESENTATION_ITEM ( )  RATIONAL_B_SPLINE_SURFACE ( (
 ( 1.000000000000000000, 0.9815197824473230748, 1.000000000000000000),
 ( 1.000000000000000000, 0.9811767838541908260, 1.000000000000000000),
 ( 1.000000000000000000, 0.9804039767750601930, 1.000000000000000000),
 ( 1.000000000000000000, 0.9775760511956556043, 1.000000000000000000),
 ( 1.000000000000000000, 0.9755247961213088237, 1.000000000000000000),
 ( 1.000000000000000000, 0.9705275854490454934, 1.000000000000000000),
 ( 1.000000000000000000, 0.9675790768636264305, 1.000000000000000000),
 ( 1.000000000000000000, 0.9611010073734985726, 1.000000000000000000),
 ( 1.000000000000000000, 0.9576315359772256119, 1.000000000000000000),
 ( 1.000000000000000000, 0.9503812888618250465, 1.000000000000000000),
 ( 1.000000000000000000, 0.9466096088173908685, 1.000000000000000000),
 ( 1.000000000000000000, 0.9387890754394591086, 1.000000000000000000),
 ( 1.000000000000000000, 0.9347210935279032240, 1.000000000000000000),
 ( 1.000000000000000000, 0.9222591698797557580, 1.000000000000000000),
 ( 1.000000000000000000, 0.9133676415885699784, 1.000000000000000000),
 ( 1.000000000000000000, 0.8858621071863931329, 1.000000000000000000),
 ( 1.000000000000000000, 0.8667308185392221809, 1.000000000000000000),
 ( 1.000000000000000000, 0.8330124393846976005, 1.000000000000000000),
 ( 1.000000000000000000, 0.8190729568369321534, 1.000000000000000000),
 ( 1.000000000000000000, 0.8123912451051846784, 1.000000000000000000) ) ) 
 REPRESENTATION_ITEM ( '' )  SURFACE ( )  );
#41625 = CARTESIAN_POINT ( 'NONE',  ( 18.78841748004269974, 148.4604323410545987, -1.722921296925317147 ) ) ;
#41626 = TOROIDAL_SURFACE ( 'NONE', #38215, 0.7620000000000000107, 0.2540000000000000036 ) ;
#41627 = CARTESIAN_POINT ( 'NONE',  ( -20.57609261220312646, 150.0789294893613999, -2.287104906598478316 ) ) ;
#41628 = CARTESIAN_POINT ( 'NONE',  ( -55.60508136934060275, 7.116827924314645060, -3.170888472016298198 ) ) ;
#41629 = CARTESIAN_POINT ( 'NONE',  ( 12.53742732955027606, 130.7145975665201831, -0.5304871790577961876 ) ) ;
#41630 = EDGE_LOOP ( 'NONE', ( #39522, #26195, #25771, #10407 ) ) ;
#41631 = CARTESIAN_POINT ( 'NONE',  ( -11.43271672892790569, 123.4929228318607386, -1.641276387634013068 ) ) ;
#41632 = CARTESIAN_POINT ( 'NONE',  ( 3.879565938682602244, -15.27118588775909558, 0.8622231344456012803 ) ) ;
#41633 = AXIS2_PLACEMENT_3D ( 'NONE', #41287, #27857, #34678 ) ;
#41634 = CARTESIAN_POINT ( 'NONE',  ( -4.065972646788793554, 118.2429491485453070, -0.3080848862740693250 ) ) ;
#41635 = CIRCLE ( 'NONE', #24601, 0.2540000000000002811 ) ;
#41636 = B_SPLINE_CURVE_WITH_KNOTS ( 'NONE', 3,
 ( #35518, #19310, #32314, #9319, #28697, #16107 ),
 .UNSPECIFIED., .F., .F.,
 ( 4, 2, 4 ),
 ( 0.000000000000000000, 0.5000000000000000000, 1.000000000000000000 ),
 .UNSPECIFIED. ) ;
#41637 = CYLINDRICAL_SURFACE ( 'NONE', #20628, 0.6350000000000014522 ) ;
#41638 = CARTESIAN_POINT ( 'NONE',  ( -4.924535406822394989, 117.6632503266924061, 0.7817655496803809223 ) ) ;
#41639 = CARTESIAN_POINT ( 'NONE',  ( 17.82368987960353124, 147.7668373613703352, 2.290061161587757077 ) ) ;
#41640 = CARTESIAN_POINT ( 'NONE',  ( 6.349999999999945466, 85.80437499999999318, 0.000000000000000000 ) ) ;
#41641 = CARTESIAN_POINT ( 'NONE',  ( -4.598301960400187127, 22.30806413504685537, 0.5496829067130363233 ) ) ;
#41642 = CARTESIAN_POINT ( 'NONE',  ( -0.003550340867794020156, 156.3099534201614631, 0.1776735749810082476 ) ) ;
#41643 = CARTESIAN_POINT ( 'NONE',  ( -10.57002714855771686, 82.40335727708655611, -1.523999999999999355 ) ) ;
#41645 = EDGE_LOOP ( 'NONE', ( #20660, #32382, #18042, #9431 ) ) ;
#41644 = CARTESIAN_POINT ( 'NONE',  ( -49.14072577824711630, 13.89916973120783972, -8.531461402113531655E-15 ) ) ;
#41646 = CARTESIAN_POINT ( 'NONE',  ( -0.1336288617286333358, 117.3993836134496433, 1.490790157883304712 ) ) ;
#41647 = CARTESIAN_POINT ( 'NONE',  ( -58.87911280034276018, -0.2081424763510641984, 0.2451831517279786654 ) ) ;
#41648 = CARTESIAN_POINT ( 'NONE',  ( -53.87034488098446872, 9.496068333427519548, 3.775128525649497302 ) ) ;
#41649 = CARTESIAN_POINT ( 'NONE',  ( -8.744658474984799312, 117.8904183912612638, -0.6682122386599032016 ) ) ;
#41650 = CARTESIAN_POINT ( 'NONE',  ( -5.475330206976889436, 88.73331249999999670, -5.107412922131463695 ) ) ;
#41651 = CARTESIAN_POINT ( 'NONE',  ( -52.96141808003752516, 14.46028723511719960, 2.643142726894140537 ) ) ;
#41652 = CARTESIAN_POINT ( 'NONE',  ( -13.61761151811294290, 119.6358206793323404, -0.1207630679856301070 ) ) ;
#41653 = ORIENTED_EDGE ( 'NONE', *, *, #41697, .T. ) ;
#41654 = CARTESIAN_POINT ( 'NONE',  ( -47.35944255389389212, 21.37623662739411401, -4.722871667523173222 ) ) ;
#41655 = CARTESIAN_POINT ( 'NONE',  ( -6.024938603336340570, 121.4387431788835983, -0.1605761971259225818 ) ) ;
#41656 = DIRECTION ( 'NONE',  ( -0.9454731675810360558, 0.3256999990547780888, -5.459396135145339171E-16 ) ) ;
#41657 = ORIENTED_EDGE ( 'NONE', *, *, #38139, .T. ) ;
#41658 = CARTESIAN_POINT ( 'NONE',  ( 1.749836090240503017, 115.7029018622145600, -1.658193655284022183 ) ) ;
#41659 = CARTESIAN_POINT ( 'NONE',  ( -4.248167858406196373, 155.8413357349917021, -0.2489887396171406586 ) ) ;
#41660 = CARTESIAN_POINT ( 'NONE',  ( 2.071654280177509300, -15.34349575202162441, 5.977339193430266207 ) ) ;
#41661 = CARTESIAN_POINT ( 'NONE',  ( -14.11223987312423311, 121.6707806233237363, 1.016201875498928153 ) ) ;
#41662 = CARTESIAN_POINT ( 'NONE',  ( 9.638062024671789629, 56.51500000000000057, 4.786355703798467734E-15 ) ) ;
#41663 = TOROIDAL_SURFACE ( 'NONE', #163, 0.7620000000000000107, 0.2540000000000000036 ) ;
#41664 = CARTESIAN_POINT ( 'NONE',  ( 23.37685013984155091, 146.7932648766621639, 0.8013420975766075705 ) ) ;
#41665 = CARTESIAN_POINT ( 'NONE',  ( 3.788429304677606968, 121.0920094295889129, 0.1804846034801776133 ) ) ;
#41666 = CARTESIAN_POINT ( 'NONE',  ( 7.213960532363564937, 86.35999999999998522, -1.904999999999999805 ) ) ;
#41667 = CARTESIAN_POINT ( 'NONE',  ( -0.9148265087109853644, 12.81245955126885505, -0.3394028602373861392 ) ) ;
#41668 = CARTESIAN_POINT ( 'NONE',  ( -23.35646125964504094, 148.8716009884483071, -0.5438655406665984238 ) ) ;
#41669 = CARTESIAN_POINT ( 'NONE',  ( -17.14499999999999957, 71.11999999999999034, 5.714999999999999858 ) ) ;
#41670 = CARTESIAN_POINT ( 'NONE',  ( -8.798071503382049130, 117.6842349159514640, -0.1758064068840608507 ) ) ;
#41671 = ORIENTED_EDGE ( 'NONE', *, *, #17540, .T. ) ;
#41672 = CARTESIAN_POINT ( 'NONE',  ( 5.588576474492088941, 117.6380689354371185, 0.9556595479870083620 ) ) ;
#41673 = CARTESIAN_POINT ( 'NONE',  ( -58.35240408279319269, -0.2551309566431522735, -0.1643770683374448371 ) ) ;
#41674 = CARTESIAN_POINT ( 'NONE',  ( 13.72986513748882764, 121.3979351292862816, 1.556522170903472890 ) ) ;
#41675 = CARTESIAN_POINT ( 'NONE',  ( 3.234792161733059501, 118.6508749770327995, -0.7732002099368724402 ) ) ;
#41676 = CARTESIAN_POINT ( 'NONE',  ( -5.788041011255496748, 9.848169244510268427, 6.116426545680356597 ) ) ;
#41677 = CARTESIAN_POINT ( 'NONE',  ( 0.008308726997671040185, 117.3658353995175503, -0.4158026747930028688 ) ) ;
#41678 = CARTESIAN_POINT ( 'NONE',  ( 4.639512378974469442, 117.9546344694811495, -0.7582059329740499232 ) ) ;
#41679 = CARTESIAN_POINT ( 'NONE',  ( 2.934015389105384841, 107.8085536575111689, 4.480064466837520243 ) ) ;
#41680 = AXIS2_PLACEMENT_3D ( 'NONE', #31565, #25389, #35192 ) ;
#41681 = CARTESIAN_POINT ( 'NONE',  ( -2.899431565053971482, 156.0891579660883508, 0.02704053119243729833 ) ) ;
#41682 = CARTESIAN_POINT ( 'NONE',  ( -18.41451321397408947, 140.7300538122508726, -2.503121031321716039 ) ) ;
#41683 = CARTESIAN_POINT ( 'NONE',  ( 5.598737995799250911, -15.07077801197512201, 2.339151774602123979 ) ) ;
#41684 = CARTESIAN_POINT ( 'NONE',  ( 5.240064600364064518, 115.6909491485453145, 1.019995478573027414 ) ) ;
#41685 = CARTESIAN_POINT ( 'NONE',  ( -1.569852930085959608, 117.3993836557238239, -1.461717798063053797 ) ) ;
#41686 = VERTEX_POINT ( 'NONE', #6769 ) ;
#41687 = CARTESIAN_POINT ( 'NONE',  ( 18.62504088965185289, 146.9271955717142930, 2.448500584228244126 ) ) ;
#41688 = DIRECTION ( 'NONE',  ( 0.2883665106726556182, 0.9575201071113218498, -1.461927526771632227E-15 ) ) ;
#41689 = VECTOR ( 'NONE', #17331, 1000.000000000000000 ) ;
#41690 = CARTESIAN_POINT ( 'NONE',  ( -3.226952561781478934, 118.4615047536228047, 0.6622324852003674822 ) ) ;
#41691 = CARTESIAN_POINT ( 'NONE',  ( 1.958624548881832350, -3.744965520567712147, -8.202033116754515518 ) ) ;
#41692 = CARTESIAN_POINT ( 'NONE',  ( 15.56852431296066186, 143.6313904367523833, 1.174399326838564406 ) ) ;
#41693 = CARTESIAN_POINT ( 'NONE',  ( 19.68299761936897596, 128.7577553591919752, -0.4435077540095086479 ) ) ;
#41694 = DIRECTION ( 'NONE',  ( 0.8745520943968243532, -0.4849315768086547296, 6.829619984160642269E-16 ) ) ;
#41695 = CARTESIAN_POINT ( 'NONE',  ( -58.36603438765030916, -0.2837009127254847551, 0.07595423550348634478 ) ) ;
#41696 = CIRCLE ( 'NONE', #27422, 0.2539999999999989488 ) ;
#41697 = EDGE_CURVE ( 'NONE', #31392, #450, #5978, .T. ) ;
#41698 = CARTESIAN_POINT ( 'NONE',  ( -4.074955089416341991, 118.2429491485453497, 0.1454234154749720065 ) ) ;
#41699 = AXIS2_PLACEMENT_3D ( 'NONE', #27218, #17203, #16989 ) ;
#41700 = CARTESIAN_POINT ( 'NONE',  ( -21.90559427349704080, 151.4293160993575498, -0.4377259060014663805 ) ) ;
#41701 = VERTEX_POINT ( 'NONE', #1024 ) ;
#41702 = CARTESIAN_POINT ( 'NONE',  ( -4.749839897611219719, 119.8691466069420386, -0.9036556220809790485 ) ) ;
#41703 = CARTESIAN_POINT ( 'NONE',  ( 6.003782516340518072, -14.18168619767446970, 2.149731705819561078 ) ) ;
#41704 = CARTESIAN_POINT ( 'NONE',  ( -12.02994987064033161, 151.9703418938154584, -0.9209848757141018138 ) ) ;
#41705 = CARTESIAN_POINT ( 'NONE',  ( -41.05189575270519242, 23.09451173561982529, 1.270000000000008233 ) ) ;
#41706 = CARTESIAN_POINT ( 'NONE',  ( 16.17518884899999421, 121.2571949256804089, 0.3403554851049458430 ) ) ;
#41707 = ADVANCED_FACE ( 'NONE', ( #19735 ), #11394, .T. ) ;
#41708 = ORIENTED_EDGE ( 'NONE', *, *, #37275, .F. ) ;
#41709 = CARTESIAN_POINT ( 'NONE',  ( -4.157303687089163979, 2.242350289152962528, -2.029258473605290103 ) ) ;
#41710 = CARTESIAN_POINT ( 'NONE',  ( -30.53944104307796081, 56.31939948586154543, 1.523999999999138932 ) ) ;
#41711 = DIRECTION ( 'NONE',  ( 1.000000000000000000, 0.000000000000000000, 0.000000000000000000 ) ) ;
#41712 = CYLINDRICAL_SURFACE ( 'NONE', #10864, 3.175000000000001155 ) ;
#41713 = CARTESIAN_POINT ( 'NONE',  ( -14.79536922792821052, 61.64024183321802752, 1.905000000000008686 ) ) ;
#41714 = CARTESIAN_POINT ( 'NONE',  ( -6.104897796072584981, 120.8184930544039162, 0.6511854637274143709 ) ) ;
#41715 = CARTESIAN_POINT ( 'NONE',  ( -25.54582022140424868, 74.24898932292961717, 1.269999999999993356 ) ) ;
#41716 = CARTESIAN_POINT ( 'NONE',  ( -0.01645572339174201579, 159.4324016994384010, 0.8235116888278194436 ) ) ;
#41717 = CARTESIAN_POINT ( 'NONE',  ( 4.430104212713525058, 104.6144662015457527, -1.942668526382494543 ) ) ;
#41719 = CARTESIAN_POINT ( 'NONE',  ( 1.228124343680933261, 158.9035955689636523, -1.375095950729813943 ) ) ;
#41718 = CARTESIAN_POINT ( 'NONE',  ( 2.829627719599027369, -13.65247383265987757, 0.5238048331051645690 ) ) ;
#41720 = TOROIDAL_SURFACE ( 'NONE', #23321, 8.794749999999998735, 0.2540000000000000036 ) ;
#41721 = CARTESIAN_POINT ( 'NONE',  ( -13.17493328878366299, 125.9194590699508893, 1.341157253524417170 ) ) ;
#41722 = CARTESIAN_POINT ( 'NONE',  ( 4.382351430540762927, 4.226039240006542741, -1.512498627010908647 ) ) ;
#41723 = CARTESIAN_POINT ( 'NONE',  ( -21.82912119472394252, 136.8312970274703844, -1.482621438090450106 ) ) ;
#41724 = ORIENTED_EDGE ( 'NONE', *, *, #17876, .F. ) ;
#41725 = EDGE_CURVE ( 'NONE', #35651, #26787, #22933, .T. ) ;
#41726 = CARTESIAN_POINT ( 'NONE',  ( -54.90394170586843359, 6.776736168479208011, 2.460356751892049942 ) ) ;
#41727 = CARTESIAN_POINT ( 'NONE',  ( -15.85992372348541579, 147.2950763206921181, 0.4080883723285145814 ) ) ;
#41728 = CARTESIAN_POINT ( 'NONE',  ( 2.063686733023943898, -15.30319371230426384, 5.972472134935498111 ) ) ;
#41729 = CARTESIAN_POINT ( 'NONE',  ( -5.008552712180506461, 117.3993836135855560, 0.7755994290793736257 ) ) ;
#41730 = CIRCLE ( 'NONE', #15194, 7.461249999999999716 ) ;
#41731 = CARTESIAN_POINT ( 'NONE',  ( -4.586119793225739372, 118.0663795823288353, -0.7418019183852817555 ) ) ;
#41732 = CARTESIAN_POINT ( 'NONE',  ( 14.67586190579446814, 148.8475317811793559, 0.2426438148417039697 ) ) ;
#41733 = EDGE_LOOP ( 'NONE', ( #20956, #29243, #19094, #12092 ) ) ;
#41734 = ADVANCED_FACE ( 'NONE', ( #12430 ), #7346, .T. ) ;
#41735 = CARTESIAN_POINT ( 'NONE',  ( 12.85210230480885585, 122.5866728308148055, 1.831397601346916648 ) ) ;
#41736 = CARTESIAN_POINT ( 'NONE',  ( -41.28107547821692691, 23.22158991241129300, -1.523999999999999355 ) ) ;
#41737 = CARTESIAN_POINT ( 'NONE',  ( -10.92199999999999704, 16.51000000000000156, 5.016499999999999737 ) ) ;
#41738 = ADVANCED_BREP_SHAPE_REPRESENTATION ( '', ( #24793, #3275 ), #20939 ) ;
#41739 = CARTESIAN_POINT ( 'NONE',  ( -18.18789719519578441, 154.1160801429439857, 0.6523539814353516153 ) ) ;
#41740 = EDGE_CURVE ( 'NONE', #37188, #31966, #24993, .T. ) ;
#41741 = CARTESIAN_POINT ( 'NONE',  ( 4.897476660045440688, 117.4787344905149098, -0.9609658134757302905 ) ) ;
#41742 = CARTESIAN_POINT ( 'NONE',  ( 13.35275951139058215, 156.9675713949798421, -0.1105600748258539628 ) ) ;
#41743 = EDGE_CURVE ( 'NONE', #13790, #6891, #36266, .T. ) ;
#41744 = CARTESIAN_POINT ( 'NONE',  ( -13.99440778436217592, 79.95103047660883533, -1.270000000000000240 ) ) ;
#41745 = AXIS2_PLACEMENT_3D ( 'NONE', #40199, #13774, #7192 ) ;
#41746 = CARTESIAN_POINT ( 'NONE',  ( -10.45722248778793428, 56.52709681235294426, 5.016499999999999737 ) ) ;
#41747 = CARTESIAN_POINT ( 'NONE',  ( -46.67763236942723637, 26.04755295256607539, 0.6632588273528772227 ) ) ;
#41748 = CARTESIAN_POINT ( 'NONE',  ( 1.998290986358403076, -15.32462849664768889, 5.352800482084254519 ) ) ;
#41749 = CARTESIAN_POINT ( 'NONE',  ( -46.42538233320968288, 20.85422009098716956, 4.815137874471020041 ) ) ;
#41750 = DIRECTION ( 'NONE',  ( 0.7770581983690701966, -0.6294287539884197979, 8.537024980200731099E-16 ) ) ;
#41751 = VECTOR ( 'NONE', #21416, 1000.000000000000114 ) ;
#41752 = CARTESIAN_POINT ( 'NONE',  ( -4.634698098077384643, 118.0229612706176852, 0.6599311673777064069 ) ) ;
#41753 = ORIENTED_EDGE ( 'NONE', *, *, #26140, .F. ) ;
#41754 = ORIENTED_EDGE ( 'NONE', *, *, #25333, .T. ) ;
#41755 = CARTESIAN_POINT ( 'NONE',  ( -0.9591419137607016809, 118.7629491485454025, -1.264665336164764176 ) ) ;
#41756 = CARTESIAN_POINT ( 'NONE',  ( 8.418152194937446708, 119.6600584949201789, -1.087643031981900821 ) ) ;
#41757 = CARTESIAN_POINT ( 'NONE',  ( -5.124638537096644519, 121.7269124416356192, -0.3048162158978747760 ) ) ;
#41758 = CARTESIAN_POINT ( 'NONE',  ( 4.716237012333075462, 117.9479786380103832, 0.8297904974140549728 ) ) ;
#41759 = CARTESIAN_POINT ( 'NONE',  ( 2.768561164044480272, -13.57843041371762460, 0.3119852368007841603 ) ) ;
#41760 = CARTESIAN_POINT ( 'NONE',  ( -14.94238115049602555, 139.3652335140928074, -1.424457715676853420 ) ) ;
#41761 = CIRCLE ( 'NONE', #24069, 0.2539999999999998925 ) ;
#41762 = CARTESIAN_POINT ( 'NONE',  ( -3.234620543671446136, 115.7029687495403465, -1.652800550241499078 ) ) ;
#41763 = CYLINDRICAL_SURFACE ( 'NONE', #29894, 0.6349999999999966782 ) ;
#41764 = CARTESIAN_POINT ( 'NONE',  ( -8.723850037987370243, 68.58388863026051752, -1.523999999999996025 ) ) ;
#41765 = CARTESIAN_POINT ( 'NONE',  ( 7.280302209287049742, 123.0424313102424492, 0.07662657258806362948 ) ) ;
#41766 = CARTESIAN_POINT ( 'NONE',  ( -7.123980356064119945, 155.7895407640516510, -1.727872795330590128 ) ) ;
#41767 = CARTESIAN_POINT ( 'NONE',  ( 23.42514220145532988, 142.8382549600662799, 0.4680900899251592140 ) ) ;
#41768 = CARTESIAN_POINT ( 'NONE',  ( -5.495523183683927115, 31.57050297546189199, 3.325088329614593885 ) ) ;
#41769 = CARTESIAN_POINT ( 'NONE',  ( -2.411564736306322398, 115.7029271828744328, 1.607687481377515049 ) ) ;
#41770 = CARTESIAN_POINT ( 'NONE',  ( 0.7007450612751181529, 9.901275517365906609, -4.597291952374415125 ) ) ;
#41772 = EDGE_LOOP ( 'NONE', ( #32425, #22928, #21318, #14375 ) ) ;
#41771 = CARTESIAN_POINT ( 'NONE',  ( 18.41332411163117655, 154.1649927243852858, 1.048538238682171997 ) ) ;
#41773 = CARTESIAN_POINT ( 'NONE',  ( 4.564577935816950038, 105.1216013620187937, -2.766951086067501731 ) ) ;
#41774 = TOROIDAL_SURFACE ( 'NONE', #24747, 0.7620000000000000107, 0.2540000000000000036 ) ;
#41775 = CARTESIAN_POINT ( 'NONE',  ( 3.037377538037926428, -15.29769487807139328, 4.066060606540134792 ) ) ;
#41776 = CARTESIAN_POINT ( 'NONE',  ( -13.67124846526819404, 154.1626644387825991, 1.747499485815532383 ) ) ;
#41777 = CARTESIAN_POINT ( 'NONE',  ( -0.9708255322354510941, 17.08399857615920325, -0.1324238259073569901 ) ) ;
#41778 = CARTESIAN_POINT ( 'NONE',  ( 0.1248384507886338285, 1.166626901725996035, -0.9703616065359238485 ) ) ;
#41779 = VERTEX_POINT ( 'NONE', #22196 ) ;
#41780 = ORIENTED_EDGE ( 'NONE', *, *, #34161, .F. ) ;
#41781 = CARTESIAN_POINT ( 'NONE',  ( -41.05189575270517111, 23.09451173561986081, 1.396999999999993358 ) ) ;
#41782 = CARTESIAN_POINT ( 'NONE',  ( 3.948369173669610266, 116.4303826247378026, 1.336099082351541956 ) ) ;
#41783 = CARTESIAN_POINT ( 'NONE',  ( -11.42136869062017546, 126.1532465342912985, 0.7903108812046737430 ) ) ;
#41784 = DIRECTION ( 'NONE',  ( -0.9816537812491094028, -0.1906721105965052399, -7.903751763042053911E-15 ) ) ;
#41785 = CARTESIAN_POINT ( 'NONE',  ( 3.507226199677831779, -13.17319675123219902, 2.199731216082013940 ) ) ;
#41786 = CARTESIAN_POINT ( 'NONE',  ( 0.009931517865167266770, 119.6374844068871397, -0.4970137656763585210 ) ) ;
#41787 =( REPRESENTATION_RELATIONSHIP ('NONE','NONE', #30767, #22056 ) REPRESENTATION_RELATIONSHIP_WITH_TRANSFORMATION ( #14045 )SHAPE_REPRESENTATION_RELATIONSHIP( ) );
#41788 = AXIS2_PLACEMENT_3D ( 'NONE', #17545, #26935, #23721 ) ;
#41789 = CARTESIAN_POINT ( 'NONE',  ( -18.11894642568450919, 135.6759721228443425, -2.431264806327576800 ) ) ;
#41790 = CARTESIAN_POINT ( 'NONE',  ( -48.24248240369263385, 19.61030762366437585, -5.299013890195634957 ) ) ;
#41791 = CARTESIAN_POINT ( 'NONE',  ( 7.920580043951711779, 121.8826771451813613, 1.006826982956816163 ) ) ;
#41792 = CARTESIAN_POINT ( 'NONE',  ( -4.834802360910630981, 32.27718159487177729, 0.9856153350916395661 ) ) ;
#41793 = CARTESIAN_POINT ( 'NONE',  ( 0.002455802209136731355, 120.8958299794632438, -0.1228983847502213983 ) ) ;
#41794 = EDGE_CURVE ( 'NONE', #13695, #4510, #8817, .T. ) ;
#41795 = VERTEX_POINT ( 'NONE', #37993 ) ;
#41796 = DIRECTION ( 'NONE',  ( -0.8745520943968249084, 0.4849315768086536194, -5.575199987069925217E-16 ) ) ;
#41797 = EDGE_CURVE ( 'NONE', #9538, #9715, #6638, .T. ) ;
#41798 = FACE_OUTER_BOUND ( 'NONE', #13487, .T. ) ;
#41799 = AXIS2_PLACEMENT_3D ( 'NONE', #2353, #25536, #38537 ) ;
#41800 = CARTESIAN_POINT ( 'NONE',  ( 5.005814566362175810, 117.5914570300447224, -0.5468859341934453333 ) ) ;
#41801 = CARTESIAN_POINT ( 'NONE',  ( -1.191460153279743750, 25.61543958765020434, -8.344265960924422743 ) ) ;
#41802 = CARTESIAN_POINT ( 'NONE',  ( 8.439375761976323886, 122.5794309061019618, 0.8715591655942096505 ) ) ;
#41803 = DIRECTION ( 'NONE',  ( 0.9998004120163608288, 0.000000000000000000, 0.01997839162482760791 ) ) ;
#41804 = CARTESIAN_POINT ( 'NONE',  ( 23.34248308131507343, 149.0646716566344026, 0.3893018266236030200 ) ) ;
#41805 = ADVANCED_FACE ( 'NONE', ( #11575 ), #16154, .T. ) ;
#41806 = CARTESIAN_POINT ( 'NONE',  ( -5.755298473670496406, 118.4539739381501988, 0.4326931426192711094 ) ) ;
#41807 = AXIS2_PLACEMENT_3D ( 'NONE', #3166, #12329, #41939 ) ;
#41808 = EDGE_CURVE ( 'NONE', #4943, #41561, #27730, .T. ) ;
#41809 = DIRECTION ( 'NONE',  ( -1.000000000000000000, 0.000000000000000000, 0.000000000000000000 ) ) ;
#41810 = CARTESIAN_POINT ( 'NONE',  ( 9.163388821854780986, 124.2347608867413413, 0.1831063163140475014 ) ) ;
#41811 = CARTESIAN_POINT ( 'NONE',  ( 4.854614700615579537, 158.3981005702974016, 1.674235554132198711 ) ) ;
#41812 = CARTESIAN_POINT ( 'NONE',  ( 7.497756367663003019, 26.09243224653669913, 3.946719672664338319 ) ) ;
#41813 = CARTESIAN_POINT ( 'NONE',  ( -2.155743978310675324, 116.6960643046747350, -0.4748305728995025898 ) ) ;
#41814 = CARTESIAN_POINT ( 'NONE',  ( -1.051265659380997475, 124.5996987749017109, -0.05046802306060373805 ) ) ;
#41815 = AXIS2_PLACEMENT_3D ( 'NONE', #8312, #11498, #11711 ) ;
#41816 = CARTESIAN_POINT ( 'NONE',  ( -8.336765840796966032, 73.19241104973453105, -1.523999999999996691 ) ) ;
#41817 = ADVANCED_FACE ( 'NONE', ( #31171 ), #40013, .T. ) ;
#41818 = DIRECTION ( 'NONE',  ( 0.9998004120163610509, 4.016384292689131511E-17, 0.01997839162482749689 ) ) ;
#41819 = CARTESIAN_POINT ( 'NONE',  ( -3.699395962244802050, 104.6144662015720144, 3.858360345332156882 ) ) ;
#41820 = CARTESIAN_POINT ( 'NONE',  ( 3.655561289726139140, 27.93047918286777076, -2.829280713513928180 ) ) ;
#41821 = CARTESIAN_POINT ( 'NONE',  ( -46.96327221648707706, 24.95754849389498276, -2.007562630684416316 ) ) ;
#41822 = CARTESIAN_POINT ( 'NONE',  ( -6.654617103318593247E-14, 104.6144662015457243, 1.534725424433578570E-31 ) ) ;
#41823 = CARTESIAN_POINT ( 'NONE',  ( 3.075357915497110017, -13.94103813162880989, 1.416127232796946966 ) ) ;
#41824 = CARTESIAN_POINT ( 'NONE',  ( 0.3780739950604312671, 121.2597428844643161, -0.4280417039577731342 ) ) ;
#41825 = CARTESIAN_POINT ( 'NONE',  ( -0.005431400947739175623, 116.8580640273661118, 0.2718095133625909043 ) ) ;
#41826 = ORIENTED_EDGE ( 'NONE', *, *, #1086, .F. ) ;
#41827 = CARTESIAN_POINT ( 'NONE',  ( 5.475330206976798841, 65.30181249999998272, 5.107412922131463695 ) ) ;
#41828 = ORIENTED_EDGE ( 'NONE', *, *, #12591, .T. ) ;
#41829 = DIRECTION ( 'NONE',  ( -5.188838149069471174E-16, 1.699382548006136313E-16, 1.000000000000000000 ) ) ;
#41830 = CARTESIAN_POINT ( 'NONE',  ( 2.247313541653549240, -15.69307202063721718, 5.732350583303913893 ) ) ;
#41831 = CARTESIAN_POINT ( 'NONE',  ( -1.201082828432692873, 118.2527139659984101, 0.6198154079389068816 ) ) ;
#41832 = CARTESIAN_POINT ( 'NONE',  ( 1.297493386698500339, 159.2526592949493534, -1.079139715401668198 ) ) ;
#41833 = CARTESIAN_POINT ( 'NONE',  ( -4.157303687089163979, 2.242350289152962528, -2.029258473605290103 ) ) ;
#41834 = CARTESIAN_POINT ( 'NONE',  ( -58.41621559020261145, 0.1608283494537381952, -0.8351736514677311485 ) ) ;
#41835 = EDGE_LOOP ( 'NONE', ( #17784, #40930, #28365, #3228 ) ) ;
#41836 = CARTESIAN_POINT ( 'NONE',  ( -58.42460811326409242, -0.3780437665165939931, -0.3615838660060010090 ) ) ;
#41837 = CARTESIAN_POINT ( 'NONE',  ( -0.01180776362034474322, 120.3637084677655764, 0.5909087754569243289 ) ) ;
#41838 =( LENGTH_UNIT ( ) NAMED_UNIT ( * ) SI_UNIT ( .MILLI., .METRE. ) );
#41839 = CARTESIAN_POINT ( 'NONE',  ( -17.26811951358317643, 148.1877419978735873, 1.462309189260816877 ) ) ;
#41840 = DIRECTION ( 'NONE',  ( 1.000000000000000000, 0.000000000000000000, 0.000000000000000000 ) ) ;
#41841 = CARTESIAN_POINT ( 'NONE',  ( 12.95103886519473768, 123.9867020804889961, -1.362965731555214832 ) ) ;
#41842 = CARTESIAN_POINT ( 'NONE',  ( -1.137402291071538230, 117.9723128000925669, -0.6313431152059613138 ) ) ;
#41843 = CARTESIAN_POINT ( 'NONE',  ( -57.39043856515510811, 2.569568763584578974, -1.997829887931768411 ) ) ;
#41844 = ORIENTED_EDGE ( 'NONE', *, *, #5898, .F. ) ;
#41845 = CARTESIAN_POINT ( 'NONE',  ( 12.68314523066099575, 130.7634385742845780, -0.6346334167959435391 ) ) ;
#41846 = ORIENTED_EDGE ( 'NONE', *, *, #29867, .T. ) ;
#41847 = CARTESIAN_POINT ( 'NONE',  ( -5.064401052258248548, 119.9665122172617231, -0.9903757029826917302 ) ) ;
#41848 = CARTESIAN_POINT ( 'NONE',  ( 3.351832917607362461, -15.21525542808549503, 3.277475278119628133 ) ) ;
#41849 = CARTESIAN_POINT ( 'NONE',  ( -5.586884702347495235, 66.64146620154573952, -0.1116392523995361763 ) ) ;
#41850 = CARTESIAN_POINT ( 'NONE',  ( -51.86985193027736329, 10.34936321858908492, -9.208787596046330052E-15 ) ) ;
#41851 = CARTESIAN_POINT ( 'NONE',  ( -4.755838299276228476, 117.7575533002713541, 0.8920572051838923100 ) ) ;
#41852 = CARTESIAN_POINT ( 'NONE',  ( 1.368713796474816391, 119.6596719632383383, 0.6021288208518276175 ) ) ;
#41853 = FACE_OUTER_BOUND ( 'NONE', #37774, .T. ) ;
#41854 = ADVANCED_FACE ( 'NONE', ( #9236 ), #24779, .T. ) ;
#41855 = CARTESIAN_POINT ( 'NONE',  ( 1.141857472271699425, 24.90688314728939190, 4.478778191171412182 ) ) ;
#41856 = CARTESIAN_POINT ( 'NONE',  ( 14.70702164887880770, 148.8393470518043955, 0.6194100056173929003 ) ) ;
#41857 = DIRECTION ( 'NONE',  ( 0.8745520943968250194, -0.4849315768086534528, 5.361993529360573944E-16 ) ) ;
#41859 = ORIENTED_EDGE ( 'NONE', *, *, #30286, .F. ) ;
#41858 = CARTESIAN_POINT ( 'NONE',  ( -49.65974013515536711, 15.91765330076391116, -3.790917083309719438 ) ) ;
#41860 = DIRECTION ( 'NONE',  ( 5.188838149069472160E-16, -1.699382548006136559E-16, -1.000000000000000000 ) ) ;
#41861 = CARTESIAN_POINT ( 'NONE',  ( -46.72244981118252838, 25.93862755320720836, -1.367307599761695025 ) ) ;
#41862 = CARTESIAN_POINT ( 'NONE',  ( -51.46667322576657000, 13.85963790048950628, 4.568971727754695955 ) ) ;
#41863 = DIRECTION ( 'NONE',  ( 5.188838149069472160E-16, -1.699382548006136066E-16, -1.000000000000000000 ) ) ;
#41864 = CARTESIAN_POINT ( 'NONE',  ( -5.305748947172302721, 77.01756249999996840, -5.247078976224250013 ) ) ;
#41865 = CARTESIAN_POINT ( 'NONE',  ( -57.42300747107054093, 3.318281940618617032, 1.876676483338158619 ) ) ;
#41866 = CARTESIAN_POINT ( 'NONE',  ( -0.3092006194328519864, 116.5226405152084652, 0.1184213420814131668 ) ) ;
#41867 = ORIENTED_EDGE ( 'NONE', *, *, #1409, .F. ) ;
#41868 = CARTESIAN_POINT ( 'NONE',  ( -54.99893072520226411, 10.64604335972153137, -1.135982259999790855 ) ) ;
#41869 = CARTESIAN_POINT ( 'NONE',  ( -6.930752631510202377, 121.9162265043544835, -0.3522179438235389370 ) ) ;
#41870 = CARTESIAN_POINT ( 'NONE',  ( -5.586884702347496123, 81.62746620154572952, -0.1116392523995361624 ) ) ;
#41871 = ORIENTED_EDGE ( 'NONE', *, *, #38602, .F. ) ;
#41872 = CARTESIAN_POINT ( 'NONE',  ( 2.568899511553136783, 115.7029491485453292, -1.594678113571031286 ) ) ;
#41873 = CARTESIAN_POINT ( 'NONE',  ( -15.78659908163013093, 146.5797798787131399, -0.5456203974801296930 ) ) ;
#41874 = CARTESIAN_POINT ( 'NONE',  ( 5.096701352355580639, -14.12304281641942083, 3.871056799387667002 ) ) ;
#41875 = CARTESIAN_POINT ( 'NONE',  ( -7.150008447151775748, 158.1912585135832785, 1.373277972272069825 ) ) ;
#41876 = CARTESIAN_POINT ( 'NONE',  ( 5.249547376965405299, 56.51500000000000767, -4.563748390642682118 ) ) ;
#41877 = CARTESIAN_POINT ( 'NONE',  ( 15.99642297876436459, 121.2237126890796191, 0.5535212332769011701 ) ) ;
#41878 = CARTESIAN_POINT ( 'NONE',  ( 3.778529602317638680, 121.0927827002991819, 0.1453591938630250935 ) ) ;
#41879 = CARTESIAN_POINT ( 'NONE',  ( 15.15189561879875768, 77.97492127061545375, 1.904999999999999583 ) ) ;
#41880 = CARTESIAN_POINT ( 'NONE',  ( -0.5393284202071846334, 5.265691905141185458, 0.8139242273222374591 ) ) ;
#41881 = CARTESIAN_POINT ( 'NONE',  ( -0.3005257795023814071, 116.4832816433156069, -0.09989594597631674955 ) ) ;
#41882 = CARTESIAN_POINT ( 'NONE',  ( 10.28897677580358128, 57.14999999999999858, 4.381499999999999950 ) ) ;
#41883 = LINE ( 'NONE', #3110, #24092 ) ;
#41884 = ORIENTED_EDGE ( 'NONE', *, *, #1140, .F. ) ;
#41885 = STYLED_ITEM ( 'NONE', ( #1878 ), #38535 ) ;
#41886 = CARTESIAN_POINT ( 'NONE',  ( -5.555942344568563840, 117.1561234432993643, 0.5128540820207154738 ) ) ;
#41887 = EDGE_LOOP ( 'NONE', ( #20554, #1921, #41517, #7468 ) ) ;
#41888 = CARTESIAN_POINT ( 'NONE',  ( -58.36886504962463107, -0.2896226415746989691, -0.03617577931945905462 ) ) ;
#41889 = CARTESIAN_POINT ( 'NONE',  ( 3.058686590879918565, 117.8293475852256904, 0.7841115193421155372 ) ) ;
#41890 = CARTESIAN_POINT ( 'NONE',  ( 5.005942668485452884, 118.7197616721209670, -0.8869178833313972055 ) ) ;
#41891 = CARTESIAN_POINT ( 'NONE',  ( 8.241158353334730791, 13.74789577914289929, -1.876134369653635448 ) ) ;
#41892 = CARTESIAN_POINT ( 'NONE',  ( -12.60858107845361786, 120.1953580586475567, -1.309872962259287732 ) ) ;
#41893 = CARTESIAN_POINT ( 'NONE',  ( 4.623501416330991987, 117.9757844860477718, -0.7388109444679361593 ) ) ;
#41894 = CARTESIAN_POINT ( 'NONE',  ( 4.396974916608523465, 111.2411499886600268, 3.139452135551013434 ) ) ;
#41895 = CARTESIAN_POINT ( 'NONE',  ( -15.38626016046121237, 147.8278496344100859, -0.1795882337043282206 ) ) ;
#41896 = CARTESIAN_POINT ( 'NONE',  ( -18.29546242682556567, 149.1773161885088825, -2.457454238777247557 ) ) ;
#41897 = CARTESIAN_POINT ( 'NONE',  ( 4.231574481101612051, -15.55479495760878095, 4.522910428756792278 ) ) ;
#41898 = CARTESIAN_POINT ( 'NONE',  ( 4.973152232786927307, 117.3993868326352015, 0.9753084504214339923 ) ) ;
#41899 = CARTESIAN_POINT ( 'NONE',  ( -41.45218294293373162, 22.69057396248467384, -1.547390787314429472 ) ) ;
#41900 = VERTEX_POINT ( 'NONE', #32016 ) ;
#41901 = B_SPLINE_SURFACE_WITH_KNOTS ( 'NONE', 5, 5, ( 
 ( #23290, #36113, #33332, #3743, #3955, #548, #32698, #20517, #16916, #339, #29499, #39942 ),
 ( #4162, #33546, #26292, #26510, #39300, #36328, #10108, #10321, #7144, #23079, #965, #13934 ),
 ( #26930, #4504, #27067, #20234, #1309, #17882, #1520, #17048, #7900, #24275, #11083, #20444 ),
 ( #36452, #10660, #33260, #30884, #24070, #37279, #17671, #26856, #14265, #888, #4089, #1095 ),
 ( #14682, #14476, #1724, #33471, #27486, #11290, #39649, #10454, #37082, #20656, #7272, #27276 ),
 ( #40075, #7484, #10870, #40290, #30254, #21072, #13861, #17467, #4718, #23424, #7695, #30051 ),
 ( #33682, #39863, #20863, #23641, #30464, #8099, #14063, #23858, #36663, #33888, #34098, #30672 ),
 ( #40495, #4301, #4925, #36877, #17264, #41538, #34308, #11705, #34512, #38124, #31092, #37699 ),
 ( #27689, #1933, #24693, #5339, #8521, #41112, #25334, #21278, #12131, #8307, #37907, #18295 ),
 ( #11918, #31294, #12345, #11491, #22111, #5967, #24907, #5762, #37482, #38336, #8729, #2139 ),
 ( #21691, #18927, #5136, #34717, #24477, #28532, #18087, #28318, #21479, #14891, #8941, #9154 ),
 ( #31724, #31938, #31508, #27893, #40901, #35140, #5546, #15100, #28101, #18503, #2355, #15313 ),
 ( #2774, #41328, #2568, #40697, #25122, #21906, #34936, #18715, #15528, #12754, #38958, #41748 ),
 ( #6580, #7012, #9355, #9769, #3610, #13388, #29584, #41953, #22733, #3177, #38540, #19547 ),
 ( #19758, #35343, #26165, #418, #29364, #38749, #26375, #12549, #28935, #22317, #36192, #202 ) ),
 .UNSPECIFIED., .F., .F., .F.,
 ( 6, 3, 3, 3, 6 ),
 ( 6, 3, 3, 6 ),
 ( -0.3376510965135046116, -0.1035049821101841905, 0.07539719332481736869, 0.1467263880009520016, 0.3285558174568177781 ),
 ( -0.3370903632277621464, -0.1505698787908571201, 0.08591144153787821924, 0.3290542212108050757 ),
 .UNSPECIFIED. ) ;
#41902 = CARTESIAN_POINT ( 'NONE',  ( -0.03212616895158381530, 157.6269964811067155, 1.607724863813389415 ) ) ;
#41903 = DIRECTION ( 'NONE',  ( 0.9998004120163609398, 0.000000000000000000, 0.01997839162482749689 ) ) ;
#41904 = CARTESIAN_POINT ( 'NONE',  ( -8.816700480405424756, 73.94613776634058411, -1.523999999999996913 ) ) ;
#41905 = CARTESIAN_POINT ( 'NONE',  ( -2.174325380064969337, 109.8863472468248119, 3.630110603364346655 ) ) ;
#41906 = CARTESIAN_POINT ( 'NONE',  ( 3.722543281321895936, 25.13347685689727484, 7.580879713197038683 ) ) ;
#41907 = CARTESIAN_POINT ( 'NONE',  ( 9.371428955827163065, 153.8930958044198576, 0.9350090023289894248 ) ) ;
#41908 = CIRCLE ( 'NONE', #24857, 0.2540000000000010583 ) ;
#41909 = CARTESIAN_POINT ( 'NONE',  ( 0.9959262657076558556, 116.9078805053781025, -0.3180477371503354633 ) ) ;
#41910 = DIRECTION ( 'NONE',  ( 1.000000000000000000, 0.000000000000000000, 0.000000000000000000 ) ) ;
#41911 = CARTESIAN_POINT ( 'NONE',  ( -10.44685452804832160, 82.62549350906336088, 1.269999999999999796 ) ) ;
#41912 = CARTESIAN_POINT ( 'NONE',  ( -0.8865878252963214079, 116.4323782974132513, -0.004867729696705670045 ) ) ;
#41913 = EDGE_LOOP ( 'NONE', ( #1587, #8837, #40283, #12573 ) ) ;
#41914 = CARTESIAN_POINT ( 'NONE',  ( -8.163272593483668516, 120.6601310837433374, -1.404696122763769761 ) ) ;
#41915 = CARTESIAN_POINT ( 'NONE',  ( 4.691512992717155051, -14.98359649487970913, 4.483035719664550278 ) ) ;
#41916 = CARTESIAN_POINT ( 'NONE',  ( -9.476112355320577052, 124.1929984354129175, -0.6154534730440988088 ) ) ;
#41917 = CARTESIAN_POINT ( 'NONE',  ( -41.05189575270520663, 23.09451173561983595, 1.523999999999993138 ) ) ;
#41918 = CARTESIAN_POINT ( 'NONE',  ( 16.86202032626302483, 155.2029898760372646, 0.3369432954968345495 ) ) ;
#41919 = EDGE_LOOP ( 'NONE', ( #11413, #1014, #7181, #4786 ) ) ;
#41920 = CARTESIAN_POINT ( 'NONE',  ( 3.345514242732226418, 6.565394131763864216, 3.211428121085859733 ) ) ;
#41921 = CARTESIAN_POINT ( 'NONE',  ( -29.30242189341234393, 66.59148765007115855, 1.270000000000377272 ) ) ;
#41922 = CARTESIAN_POINT ( 'NONE',  ( -18.63504953328976299, 154.1157618415863624, -0.3723726386282264489 ) ) ;
#41923 = DIRECTION ( 'NONE',  ( -5.188838149069472160E-16, 1.699382548006136559E-16, 1.000000000000000000 ) ) ;
#41924 = CARTESIAN_POINT ( 'NONE',  ( -5.586884702347497011, 117.3144662015457271, -0.1116392523995361624 ) ) ;
#41925 = CARTESIAN_POINT ( 'NONE',  ( -6.999189161217031163, 121.8522563078195589, 0.1888263321353615132 ) ) ;
#41926 = CARTESIAN_POINT ( 'NONE',  ( 2.245307460665866728, 11.68515688572553479, 4.070821060848484940 ) ) ;
#41927 = CARTESIAN_POINT ( 'NONE',  ( 21.90872843939978409, 150.3855106993079005, 1.734217137259093322 ) ) ;
#41928 = CARTESIAN_POINT ( 'NONE',  ( -54.28468382810587656, 8.706709151468123409, -3.613316249068738717 ) ) ;
#41930 = CARTESIAN_POINT ( 'NONE',  ( 21.09608681602914615, 148.7375953542188256, -1.514114011542639249 ) ) ;
#41929 = CARTESIAN_POINT ( 'NONE',  ( 4.575565686387192521, 113.7932280819714208, 2.209540002265822700 ) ) ;
#41931 = CARTESIAN_POINT ( 'NONE',  ( 3.547999066118234346, 14.38381850277834317, -2.990331240093012877 ) ) ;
#41932 = CARTESIAN_POINT ( 'NONE',  ( -3.159869787290223719, 159.3937097445585778, -0.6918644357365442144 ) ) ;
#41933 = AXIS2_PLACEMENT_3D ( 'NONE', #28746, #9365, #28541 ) ;
#41934 = EDGE_LOOP ( 'NONE', ( #25255, #32563, #11949, #10741 ) ) ;
#41935 = VECTOR ( 'NONE', #12450, 1000.000000000000000 ) ;
#41936 = CARTESIAN_POINT ( 'NONE',  ( -9.493134470504971389, 124.1929984354129175, 0.2364027771656556087 ) ) ;
#41937 = VECTOR ( 'NONE', #33683, 1000.000000000000000 ) ;
#41938 = CARTESIAN_POINT ( 'NONE',  ( 3.203739484688298500, -15.10556029324786032, 5.619401687775556375 ) ) ;
#41939 = DIRECTION ( 'NONE',  ( 0.6294287539884133587, 0.7770581983690755257, 0.000000000000000000 ) ) ;
#41940 = CARTESIAN_POINT ( 'NONE',  ( -4.627789221742965253, 118.0321741321441777, -0.7763224823049538204 ) ) ;
#41941 = CARTESIAN_POINT ( 'NONE',  ( 15.21351360038791789, 143.4186079242267340, 0.3040022078858843346 ) ) ;
#41942 = ORIENTED_EDGE ( 'NONE', *, *, #27222, .F. ) ;
#41943 = CARTESIAN_POINT ( 'NONE',  ( 13.90099558903402510, 123.5874490550988014, 1.899532866591826741 ) ) ;
#41944 = DIRECTION ( 'NONE',  ( 0.000000000000000000, -1.000000000000000000, 0.000000000000000000 ) ) ;
#41945 = CARTESIAN_POINT ( 'NONE',  ( -23.69188486464780752, 78.08202335040543574, -1.270000000000005347 ) ) ;
#41946 = CARTESIAN_POINT ( 'NONE',  ( -21.34935411394468119, 151.2846570542378117, 0.7363345373129177585 ) ) ;
#41947 = EDGE_CURVE ( 'NONE', #29906, #37417, #15816, .T. ) ;
#41948 = CARTESIAN_POINT ( 'NONE',  ( 4.997691741573370372, 117.4661756457942090, -0.7742298431118354030 ) ) ;
#41949 = CARTESIAN_POINT ( 'NONE',  ( 0.004355829920537035785, 116.7171338949676738, -0.2179835409713598016 ) ) ;
#41950 = CARTESIAN_POINT ( 'NONE',  ( -5.237832120027548832, 115.7029491485453860, -1.023639123012231034 ) ) ;
#41951 = CARTESIAN_POINT ( 'NONE',  ( -48.86515451709912838, 17.99370625226629983, 5.095019330712561967 ) ) ;
#41952 = CARTESIAN_POINT ( 'NONE',  ( -46.81330379368907302, 25.73549360603863434, 1.450859712031378201 ) ) ;
#41953 = CARTESIAN_POINT ( 'NONE',  ( 1.790976758586900752, -15.16497236253652758, 5.485886819307857820 ) ) ;
#41954 = CARTESIAN_POINT ( 'NONE',  ( -45.68084146533627887, 21.25878370237693815, 4.188014402015102000 ) ) ;
#41955 = DIRECTION ( 'NONE',  ( 0.6294287539884068083, 0.7770581983690809658, -6.679558114607132635E-15 ) ) ;
#41956 = CARTESIAN_POINT ( 'NONE',  ( -4.644072755505800565, 118.0368553417439443, 0.6066355437525197125 ) ) ;
#41957 = CIRCLE ( 'NONE', #41260, 5.080000000000006288 ) ;
#41958 = EDGE_LOOP ( 'NONE', ( #39265, #2118, #17330, #1524 ) ) ;
#41959 = ORIENTED_EDGE ( 'NONE', *, *, #26593, .F. ) ;
#41960 = CARTESIAN_POINT ( 'NONE',  ( -6.135835944515187101, 77.40800365160224317, 1.270000000000002904 ) ) ;
#41961 = CARTESIAN_POINT ( 'NONE',  ( 8.410696399698803560, 119.6968806642600214, -1.092398566202036569 ) ) ;
#41962 = CARTESIAN_POINT ( 'NONE',  ( -3.889650775106716196, 109.8300753404742096, -3.673692233826463482 ) ) ;
#41963 = CARTESIAN_POINT ( 'NONE',  ( 4.648831033999298867, 117.8874912827738797, 1.000901579481272119 ) ) ;
#41964 = CARTESIAN_POINT ( 'NONE',  ( 1.852819980464847305, -15.24972552306870455, 5.408883774200016425 ) ) ;
#41965 = CARTESIAN_POINT ( 'NONE',  ( -16.19371004148921855, 147.7868695473139553, -1.594401216537396415 ) ) ;
#41966 = CARTESIAN_POINT ( 'NONE',  ( -3.605926315104273971, 115.7029500413796228, -1.621950352474985868 ) ) ;
#41967 = LINE ( 'NONE', #12766, #3369 ) ;
#41968 = CARTESIAN_POINT ( 'NONE',  ( 14.39766717389552042, 60.87500489999898434, -1.904999999999999583 ) ) ;
#41969 = CARTESIAN_POINT ( 'NONE',  ( 2.162697817503714592, 106.7001829816230725, -4.879784414745867771 ) ) ;
#41970 = CARTESIAN_POINT ( 'NONE',  ( -5.840731033150244222, 120.5744318282211651, -0.9509518217554207009 ) ) ;
#41971 = DIRECTION ( 'NONE',  ( 0.1469470846586743984, 9.335746474409589170E-17, -0.9891443546370349837 ) ) ;
#41972 = CARTESIAN_POINT ( 'NONE',  ( -1.004127523102863684, 36.15709238714742924, 2.777694508738604906 ) ) ;
#41973 = CARTESIAN_POINT ( 'NONE',  ( -2.338242410153924755, 115.7028053385901956, 1.613663431231236567 ) ) ;
#41974 = CARTESIAN_POINT ( 'NONE',  ( -1.825063964020108065, -4.879331645356781877, 4.256838567046823840 ) ) ;
#41976 = ORIENTED_EDGE ( 'NONE', *, *, #17099, .F. ) ;
#41975 = CARTESIAN_POINT ( 'NONE',  ( 13.27770485956316904, 119.7426348059052685, 0.8357656065649389232 ) ) ;
#41977 = DIRECTION ( 'NONE',  ( -5.188838149069472160E-16, 1.699382548006136559E-16, 1.000000000000000000 ) ) ;
#41978 = CARTESIAN_POINT ( 'NONE',  ( 3.302563718500166612, -15.23312206205887342, 3.441858572223985391 ) ) ;
#41979 = CARTESIAN_POINT ( 'NONE',  ( -4.356286657365888715, 157.6046910967438066, 1.678189947947347216 ) ) ;
#41980 = CARTESIAN_POINT ( 'NONE',  ( 0.6674325042100914818, 1.652014723813869823, 0.7093539244141242595 ) ) ;
#41981 = AXIS2_PLACEMENT_3D ( 'NONE', #34132, #15140, #4958 ) ;
#41982 = CARTESIAN_POINT ( 'NONE',  ( 0.7576854961709549308, -2.078890728193560467, 0.6140693529290401909 ) ) ;
#41983 = EDGE_CURVE ( 'NONE', #15637, #31392, #25694, .T. ) ;
#41984 = ORIENTED_EDGE ( 'NONE', *, *, #37045, .F. ) ;
#41985 = ORIENTED_EDGE ( 'NONE', *, *, #39384, .F. ) ;
#41986 = CARTESIAN_POINT ( 'NONE',  ( -28.09515292912719175, 77.51021392068167870, -1.524000000000007571 ) ) ;
#41987 = CARTESIAN_POINT ( 'NONE',  ( 3.169910341315082647, 118.2446163226072713, 0.8422023655252532937 ) ) ;
#41988 = CARTESIAN_POINT ( 'NONE',  ( -0.7532517793759884173, 156.4767055779393559, 0.8130599351363750893 ) ) ;
#41989 =( BOUNDED_CURVE ( )  B_SPLINE_CURVE ( 3, ( #41662, #28651, #19474, #29496 ),
 .UNSPECIFIED., .F., .T. ) 
 B_SPLINE_CURVE_WITH_KNOTS ( ( 4, 4 ),
 ( 1.570796326794895892, 3.141592653589793560 ),
 .UNSPECIFIED. ) 
 CURVE ( )  GEOMETRIC_REPRESENTATION_ITEM ( )  RATIONAL_B_SPLINE_CURVE ( ( 1.000000000000000000, 0.8047378541243646044, 0.8047378541243646044, 1.000000000000000000 ) ) 
 REPRESENTATION_ITEM ( '' )  );
#41990 = CARTESIAN_POINT ( 'NONE',  ( 4.309079644119920616, -12.27988108232860931, 1.651494482198018199 ) ) ;
#41991 = CARTESIAN_POINT ( 'NONE',  ( 9.495682976374265394, 155.1592096034013366, -1.579384785498886945 ) ) ;
#41992 = AXIS2_PLACEMENT_3D ( 'NONE', #20588, #32988, #39806 ) ;
#41993 = CARTESIAN_POINT ( 'NONE',  ( -8.537619249161426893, 156.7723266660784986, -2.072230564756332161 ) ) ;
#41994 = DIRECTION ( 'NONE',  ( -0.8745520943968247973, 0.4849315768086537304, -5.361993529360573944E-16 ) ) ;
#41995 = CARTESIAN_POINT ( 'NONE',  ( 1.979187190576821465, -15.21425526833739639, 5.301287498526151332 ) ) ;
#41996 = CARTESIAN_POINT ( 'NONE',  ( -4.968091682766383244, 32.48584459999275253, 1.440197358048235010 ) ) ;
#41997 = CARTESIAN_POINT ( 'NONE',  ( 6.492420186392267922, 121.7431354732680973, -0.05225946255319164485 ) ) ;
#41998 = TOROIDAL_SURFACE ( 'NONE', #38587, 0.3809999999999990616, 0.2540000000000000036 ) ;
#41999 = ORIENTED_EDGE ( 'NONE', *, *, #10985, .T. ) ;
#42000 = CARTESIAN_POINT ( 'NONE',  ( -3.009276887026423264, 50.13146620154573441, 1.210121013456480377 ) ) ;
#42001 = DIRECTION ( 'NONE',  ( 5.206863593109713661E-17, -1.000000000000000000, 1.077750396879097183E-30 ) ) ;
#42002 = CARTESIAN_POINT ( 'NONE',  ( -4.581648513977574666, 27.87760232565343088, 0.5121129833925254227 ) ) ;
#42003 = CARTESIAN_POINT ( 'NONE',  ( 6.495892026627585913, 121.2869106855140018, 0.7936256953933333858 ) ) ;
#42004 = DIRECTION ( 'NONE',  ( 0.9454731675810336133, -0.3256999990547843615, 5.459396135145337199E-16 ) ) ;
#42005 = CARTESIAN_POINT ( 'NONE',  ( 0.0002734175338629627090, 159.6054662015457382, -0.01368293144939973158 ) ) ;
#42006 = CARTESIAN_POINT ( 'NONE',  ( -4.518882305193469229, 111.2411499886600268, 2.961292089698490226 ) ) ;
#42007 = VECTOR ( 'NONE', #29869, 1000.000000000000000 ) ;
#42008 = CARTESIAN_POINT ( 'NONE',  ( -6.538677740023618411E-14, 75.27746620154573520, -7.356392042280733227E-18 ) ) ;
#42009 = CARTESIAN_POINT ( 'NONE',  ( 4.560281875334545099, -11.68902278883368595, 0.6958564903332965512 ) ) ;
#42010 = CARTESIAN_POINT ( 'NONE',  ( -2.834545168019937389, 33.34007952871795766, 0.9740110680454012737 ) ) ;
#42011 = ADVANCED_FACE ( 'NONE', ( #8392 ), #21354, .F. ) ;
#42012 = CARTESIAN_POINT ( 'NONE',  ( 13.83539046132045414, 122.2371923977168109, 1.727333621972642064 ) ) ;
#42013 = CARTESIAN_POINT ( 'NONE',  ( -2.961220487682185709, 16.77021669962341477, -3.573240411402743621 ) ) ;
#42014 = CARTESIAN_POINT ( 'NONE',  ( 8.348643983786249834, 26.63118458923209175, 1.112826146890550483 ) ) ;
#42015 = CARTESIAN_POINT ( 'NONE',  ( 8.747260340425302871, 117.9889815745654715, -0.4087459456760704213 ) ) ;
#42016 = CARTESIAN_POINT ( 'NONE',  ( -1.574582893473529532, 118.9836165220538504, -0.7747311016372977477 ) ) ;
#42017 = CARTESIAN_POINT ( 'NONE',  ( -30.15519950990045572, 69.97033940222175374, -1.524000000000007349 ) ) ;
#42018 = CARTESIAN_POINT ( 'NONE',  ( -7.772068811996249771, 69.25462295839062676, 1.524000000000003796 ) ) ;
#42019 = CARTESIAN_POINT ( 'NONE',  ( -1.777383475896760157, 104.6144662015478985, 5.032164064983053464 ) ) ;
#42020 = CARTESIAN_POINT ( 'NONE',  ( -3.854280124997887746, 21.23357344512866973, -2.551540157904111261 ) ) ;
#42021 = CARTESIAN_POINT ( 'NONE',  ( 13.85159022459153988, 12.96416000000000146, 5.016499999999999737 ) ) ;
#42022 = CARTESIAN_POINT ( 'NONE',  ( -18.88649316419433788, 79.99958772249931371, -1.524000000000003130 ) ) ;
#42023 = CARTESIAN_POINT ( 'NONE',  ( 3.176652145978316355, -13.92691374863060183, 2.072386176210903486 ) ) ;
#42024 = CARTESIAN_POINT ( 'NONE',  ( 1.389742127967388718, 109.2701902778323557, -3.915166117862841411 ) ) ;
#42025 = CARTESIAN_POINT ( 'NONE',  ( -23.09710566998045067, 146.6371693212631158, 0.4017528712124326384 ) ) ;
#42026 = TOROIDAL_SURFACE ( 'NONE', #41933, 6.905624999999998792, 0.5556250000000014788 ) ;
#42027 = VERTEX_POINT ( 'NONE', #14975 ) ;
#42028 = ADVANCED_FACE ( 'NONE', ( #37776 ), #35024, .T. ) ;
#42029 = CARTESIAN_POINT ( 'NONE',  ( 5.965356522962838248, 88.73331249999999670, 5.016499999999999737 ) ) ;
#42030 = APPLICATION_CONTEXT ( 'automotive_design' ) ;
#42031 = ORIENTED_EDGE ( 'NONE', *, *, #18745, .F. ) ;
#42032 = CARTESIAN_POINT ( 'NONE',  ( -10.44685452804831804, 82.62549350906336088, -1.523999999999999355 ) ) ;
#42033 = CARTESIAN_POINT ( 'NONE',  ( 5.755466747078162193, -14.97439463182292840, 1.832642420680269613 ) ) ;
#42034 = CARTESIAN_POINT ( 'NONE',  ( -13.21705611421152149, 122.1656469061080514, 1.250183119358982742 ) ) ;
#42035 = CARTESIAN_POINT ( 'NONE',  ( 3.977532531966649465, 117.6225627337916393, -0.6337845664926935463 ) ) ;
#42036 = CARTESIAN_POINT ( 'NONE',  ( 4.219463811995017188, -1.205994944679912306, -1.932895124392335573 ) ) ;
#42037 = CARTESIAN_POINT ( 'NONE',  ( -56.39531427985796341, 4.462078775273103481, -2.567773104673984452 ) ) ;
#42038 = VERTEX_POINT ( 'NONE', #18800 ) ;
#42039 = CARTESIAN_POINT ( 'NONE',  ( -55.35389262108408559, 6.100188123699015641, -2.822635004244650414 ) ) ;
#42040 = CARTESIAN_POINT ( 'NONE',  ( -0.09934209769104777876, 106.7790779034713324, 4.971484795507142174 ) ) ;
#42041 = CARTESIAN_POINT ( 'NONE',  ( -4.792200577477630397, 117.5371802918334225, 0.9878184568134641408 ) ) ;
#42042 = CARTESIAN_POINT ( 'NONE',  ( -9.186197600956550247, 155.0058477609193801, 1.458900829815476197 ) ) ;
#42043 = CARTESIAN_POINT ( 'NONE',  ( -19.33375693323417011, 80.42273151551299293, -1.524000000000003574 ) ) ;
#42044 = EDGE_CURVE ( 'NONE', #16174, #21262, #4617, .T. ) ;
#42045 = CARTESIAN_POINT ( 'NONE',  ( 9.549337214233879934, 121.2752502669211339, -1.156350410895870207 ) ) ;
#42046 = CARTESIAN_POINT ( 'NONE',  ( -20.38236371569470506, 141.4490678312372722, -2.395676066357400824 ) ) ;
#42047 = CARTESIAN_POINT ( 'NONE',  ( -57.78858274104275949, 1.044662872677112997, -1.355440516197766732 ) ) ;
#42048 = AXIS2_PLACEMENT_3D ( 'NONE', #22403, #13262, #3269 ) ;
#42049 = EDGE_CURVE ( 'NONE', #13325, #11900, #32601, .T. ) ;
#42050 = ORIENTED_EDGE ( 'NONE', *, *, #36776, .F. ) ;
#42051 = CARTESIAN_POINT ( 'NONE',  ( 4.421201411745116161, 118.1651805457867539, -0.4751133233741948736 ) ) ;
#42052 = CARTESIAN_POINT ( 'NONE',  ( 3.102522256439363080, 156.1450793681712241, -0.6153187215006972188 ) ) ;
#42053 = ORIENTED_EDGE ( 'NONE', *, *, #5898, .T. ) ;
#42054 = CARTESIAN_POINT ( 'NONE',  ( -1.387234972287347379, 119.7856413326322667, -0.5781392410077788035 ) ) ;
#42055 = CARTESIAN_POINT ( 'NONE',  ( 3.434117431421463973, -14.91634622600368587, 0.6670077989445850619 ) ) ;
#42056 = CARTESIAN_POINT ( 'NONE',  ( -6.401666570281891566, 64.12941061790216679, -1.523999999999994026 ) ) ;
#42057 = CARTESIAN_POINT ( 'NONE',  ( -50.02669608763528686, 12.78473261814649931, -8.449425852006687485E-15 ) ) ;
#42058 = EDGE_CURVE ( 'NONE', #28714, #40169, #36597, .T. ) ;
#42059 = CARTESIAN_POINT ( 'NONE',  ( -4.949223898456546422, 117.6231127316777645, 0.7510713373028163886 ) ) ;
#42060 = CARTESIAN_POINT ( 'NONE',  ( 17.31991401741507630, 147.8988302317391117, 2.155506138210265821 ) ) ;
#42061 = CARTESIAN_POINT ( 'NONE',  ( -2.317791448294674872, 31.60761946039689008, 1.124105164688197211 ) ) ;
#42062 = CARTESIAN_POINT ( 'NONE',  ( 0.2927481059715184020, -9.205330264445118260, -8.420370646799414160 ) ) ;
#42063 = CARTESIAN_POINT ( 'NONE',  ( 13.60737276370606885, 150.2179846313823930, 0.4949411041190266980 ) ) ;
#42064 = FACE_OUTER_BOUND ( 'NONE', #20067, .T. ) ;
#42066 = ORIENTED_EDGE ( 'NONE', *, *, #14611, .F. ) ;
#42065 = CARTESIAN_POINT ( 'NONE',  ( -46.53889185657398286, 18.10826295091780835, -1.459106928557441618 ) ) ;
#42067 = DIRECTION ( 'NONE',  ( 0.5149185422762221354, -0.8572391118119438991, 4.128606161907600514E-16 ) ) ;
#42068 = CARTESIAN_POINT ( 'NONE',  ( -46.74256434184148645, 25.89113524595070359, -1.391884290063961416 ) ) ;
#42069 = CARTESIAN_POINT ( 'NONE',  ( -49.06145255062209287, 17.74692478680227836, 5.108567701946085116 ) ) ;
#42070 = PLANE ( 'NONE',  #39254 ) ;
#42071 = DIRECTION ( 'NONE',  ( -0.9998004120163609398, -4.016384292689130894E-17, -0.01997839162482749689 ) ) ;
#42072 = DIRECTION ( 'NONE',  ( 9.627370216492862708E-17, 1.000000000000000000, -0.000000000000000000 ) ) ;
#42073 = CARTESIAN_POINT ( 'NONE',  ( -56.90441949580814196, 4.712873715160811550, 1.842411344577081556 ) ) ;
#42074 = EDGE_CURVE ( 'NONE', #16433, #1232, #10707, .T. ) ;
#42075 = CARTESIAN_POINT ( 'NONE',  ( -57.55343345497419705, 2.880119995625998630, 1.988856187846569146 ) ) ;
#42076 = CARTESIAN_POINT ( 'NONE',  ( -6.916478980584567005, 117.2343425291504104, 0.1085122952249095302 ) ) ;
#42077 = EDGE_CURVE ( 'NONE', #17780, #24610, #28411, .T. ) ;
#42078 = ORIENTED_EDGE ( 'NONE', *, *, #40453, .F. ) ;
#42079 = CARTESIAN_POINT ( 'NONE',  ( -49.59816314059868603, 17.91649583374772092, -5.069000701391663810 ) ) ;
#42080 = CARTESIAN_POINT ( 'NONE',  ( -6.942438739474686926, 121.9314933722027234, -0.3079128108755967430 ) ) ;
#42081 = ORIENTED_EDGE ( 'NONE', *, *, #27666, .T. ) ;
#42082 = CARTESIAN_POINT ( 'NONE',  ( 2.676737444774203833, 115.7033390179947787, -1.585144796910018306 ) ) ;
#42083 = CARTESIAN_POINT ( 'NONE',  ( -11.89867495700692857, 130.3805625696445816, -0.3456363086864548961 ) ) ;
#42084 = CARTESIAN_POINT ( 'NONE',  ( 5.208971126070756519, -14.02307540452116186, 3.677211492609324228 ) ) ;
#42085 = CARTESIAN_POINT ( 'NONE',  ( -21.50873886539585556, 148.9071063441643048, 1.383230070950766999 ) ) ;
#42086 = CARTESIAN_POINT ( 'NONE',  ( -22.98045850745951313, 78.35500052582088415, 1.523999999999994248 ) ) ;
#42087 = CARTESIAN_POINT ( 'NONE',  ( 4.752142575032201499, 116.8068435238802465, 0.2604826270010439093 ) ) ;
#42088 = CARTESIAN_POINT ( 'NONE',  ( 4.619048842463770121, 121.2009516319313178, 0.1635582688743358881 ) ) ;
#42089 = DIRECTION ( 'NONE',  ( 0.7770581983690852956, -0.6294287539884014793, 6.050078592469978860E-15 ) ) ;
#42090 = CARTESIAN_POINT ( 'NONE',  ( 0.3213417908193094141, 16.26526798020547204, 0.9222100932699727194 ) ) ;
#42091 = CARTESIAN_POINT ( 'NONE',  ( -22.97436839085991878, 150.1579452496398801, -0.6125673049107096535 ) ) ;
#42092 = DIRECTION ( 'NONE',  ( 0.4849315768086533973, 0.8745520943968251304, 1.030032898892973955E-16 ) ) ;
#42093 = FACE_OUTER_BOUND ( 'NONE', #18273, .T. ) ;
#42094 = ORIENTED_EDGE ( 'NONE', *, *, #10470, .F. ) ;
#42095 = CARTESIAN_POINT ( 'NONE',  ( 8.629495036404707164, 118.4212787258601338, 1.048420227482702582 ) ) ;
#42096 = ORIENTED_EDGE ( 'NONE', *, *, #5827, .T. ) ;
#42097 = CARTESIAN_POINT ( 'NONE',  ( -58.36945504494742920, -0.2908306025726871136, -0.02357894785790005943 ) ) ;
#42098 = CARTESIAN_POINT ( 'NONE',  ( 15.52234330115196137, 154.9569273371780298, 1.915578030012927258 ) ) ;
#42099 = CARTESIAN_POINT ( 'NONE',  ( 2.272333812996608415, 118.4336326928681729, -0.6977090181727382268 ) ) ;
#42100 = CARTESIAN_POINT ( 'NONE',  ( -7.544985805786585509, 7.895591250050960852, -3.771097921825450783 ) ) ;
#42101 = TOROIDAL_SURFACE ( 'NONE', #29136, 0.7620000000000000107, 0.2540000000000000036 ) ;
#42102 = CARTESIAN_POINT ( 'NONE',  ( -15.52234330115209104, 154.9569273371780298, -1.915578030012927258 ) ) ;
#42103 = CARTESIAN_POINT ( 'NONE',  ( 4.645634966785371134, 117.9566108303512095, -0.7541813577493102771 ) ) ;
#42104 = EDGE_CURVE ( 'NONE', #27131, #31875, #18192, .T. ) ;
#42105 = CARTESIAN_POINT ( 'NONE',  ( 5.045732318125604188, 114.3381464724725447, 1.964647476694348471 ) ) ;
#42106 = CARTESIAN_POINT ( 'NONE',  ( -15.77260762454802467, 146.5697412905949477, -0.2637713227210858324 ) ) ;
#42107 = CARTESIAN_POINT ( 'NONE',  ( -11.42611330002560877, 154.6851215890897038, -2.167138196937119066 ) ) ;
#42108 = CARTESIAN_POINT ( 'NONE',  ( 5.007622726684139991, -15.39085649315211057, 3.402342850907996041 ) ) ;
#42109 = FACE_OUTER_BOUND ( 'NONE', #13924, .T. ) ;
#42110 = CARTESIAN_POINT ( 'NONE',  ( -44.13308345971568514, 24.21351174012166396, -1.567149544246662973 ) ) ;
#42111 = ORIENTED_EDGE ( 'NONE', *, *, #24028, .T. ) ;
#42112 = CARTESIAN_POINT ( 'NONE',  ( 6.601024023181092382, 120.1594786313440011, 1.214938174674062843 ) ) ;
#42113 = CARTESIAN_POINT ( 'NONE',  ( -15.72385166996626715, 146.8976323831864477, -0.3141999770531619940 ) ) ;
#42114 = CIRCLE ( 'NONE', #36661, 0.6350000000000014522 ) ;
#42115 = AXIS2_PLACEMENT_3D ( 'NONE', #24822, #21820, #21605 ) ;
#42116 = DIRECTION ( 'NONE',  ( -1.000000000000000000, 0.000000000000000000, -5.975917486140574681E-16 ) ) ;
#42117 = CARTESIAN_POINT ( 'NONE',  ( -4.831936455160952271, 120.7138498849978987, 0.2122769985084471123 ) ) ;
#42118 = CARTESIAN_POINT ( 'NONE',  ( 5.478597439045088890, 28.15663318097115209, -6.435035585623773535 ) ) ;
#42119 = CARTESIAN_POINT ( 'NONE',  ( 16.06762827093114154, 146.3760696504137684, 1.175121962453930857 ) ) ;
#42120 = CARTESIAN_POINT ( 'NONE',  ( 15.21238092238748507, 121.1469641333237917, -0.4626880538419668731 ) ) ;
#42121 = CARTESIAN_POINT ( 'NONE',  ( -26.07365872405947727, 72.73903180058835005, -1.524000000000005794 ) ) ;
#42122 = CARTESIAN_POINT ( 'NONE',  ( 4.581716828367337513, -15.30239761468843973, -0.5121115983836379559 ) ) ;
#42123 = CARTESIAN_POINT ( 'NONE',  ( -17.29948542670054223, 122.7677429521249053, -0.3279718759250787041 ) ) ;
#42124 = ORIENTED_EDGE ( 'NONE', *, *, #17305, .T. ) ;
#42125 = CARTESIAN_POINT ( 'NONE',  ( -4.985608112044036311, 120.1171868300749281, -0.8736999896306448798 ) ) ;
#42126 = DIRECTION ( 'NONE',  ( 4.017660918040594346E-17, -1.000000000000000000, -2.376309959284834438E-19 ) ) ;
#42127 = CARTESIAN_POINT ( 'NONE',  ( -13.34275001191909205, 134.1388935151753401, -0.9731691531512424165 ) ) ;
#42128 = CARTESIAN_POINT ( 'NONE',  ( 4.309079644119920616, -12.27988108232860931, 1.651494482198018199 ) ) ;
#42129 = CARTESIAN_POINT ( 'NONE',  ( -10.57002714855771686, 82.40335727708655611, 1.524000000000000243 ) ) ;
#42130 = CARTESIAN_POINT ( 'NONE',  ( 20.50094783971091772, 129.0975500345852822, 0.4299227524276376111 ) ) ;
#42131 = VERTEX_POINT ( 'NONE', #16228 ) ;
#42132 = CARTESIAN_POINT ( 'NONE',  ( -3.640175008984333882, 11.51306413504884318, -2.862805987297033727 ) ) ;
#42133 = CARTESIAN_POINT ( 'NONE',  ( -3.013063373304370796, 105.1243314539317453, 4.412133481903750543 ) ) ;
#42134 = CARTESIAN_POINT ( 'NONE',  ( -10.83330528665015891, 157.8980211815716928, -0.2164752214609687586 ) ) ;
#42135 = CARTESIAN_POINT ( 'NONE',  ( -11.58677707360137532, 17.14500000000000313, -4.474811398758258285 ) ) ;
#42136 = LINE ( 'NONE', #41924, #466 ) ;
#42137 = CARTESIAN_POINT ( 'NONE',  ( -7.829604799548672389, 122.4485675125339839, 0.2503763010704491143 ) ) ;
#42138 = AXIS2_PLACEMENT_3D ( 'NONE', #32959, #16746, #19096 ) ;
#42139 = CARTESIAN_POINT ( 'NONE',  ( 3.490194016315742331, 12.22236127277748174, 3.029891289224248219 ) ) ;
#42140 = CARTESIAN_POINT ( 'NONE',  ( 12.91997107708620263, 119.9671592456446803, 1.126112081325366665 ) ) ;
#42142 = AXIS2_PLACEMENT_3D ( 'NONE', #1533, #14076, #16854 ) ;
#42141 = CYLINDRICAL_SURFACE ( 'NONE', #11594, 0.2539999999999989488 ) ;
#42144 = CARTESIAN_POINT ( 'NONE',  ( 0.01023305610364113119, 117.8848902025789158, -0.5121039721716187376 ) ) ;
#42143 = CARTESIAN_POINT ( 'NONE',  ( 5.177913976931212581, 57.14999999999999147, 5.372099999999999653 ) ) ;
#42145 = CARTESIAN_POINT ( 'NONE',  ( -4.623654898565560778, 8.549082320728111029, 0.09932813335659773646 ) ) ;
#42146 = CARTESIAN_POINT ( 'NONE',  ( -0.3408176794666137877, 116.9919054422455531, -0.3412737040790791432 ) ) ;
#42147 = ORIENTED_EDGE ( 'NONE', *, *, #2962, .T. ) ;
#42148 = CARTESIAN_POINT ( 'NONE',  ( -5.269990328701569915, 121.3020066425206807, 0.06069006697729623090 ) ) ;
#42149 = CARTESIAN_POINT ( 'NONE',  ( 5.341071565670632459, -14.32387631201759248, 3.633538872802142716 ) ) ;
#42150 = DIRECTION ( 'NONE',  ( -0.8745520943968235761, 0.4849315768086558953, -5.361993529360570985E-16 ) ) ;
#42151 = ORIENTED_EDGE ( 'NONE', *, *, #1982, .T. ) ;
#42152 = CARTESIAN_POINT ( 'NONE',  ( 17.05522983032404483, 131.5760549582342094, 2.311017189013932605 ) ) ;
#42153 = DIRECTION ( 'NONE',  ( 9.627370216492862708E-17, 1.000000000000000000, -0.000000000000000000 ) ) ;
#42154 = CARTESIAN_POINT ( 'NONE',  ( -5.526300601521442424, 159.0395019988757781, 0.6540312330581289357 ) ) ;
#42155 = CIRCLE ( 'NONE', #21723, 5.334000000000001407 ) ;
#42156 = CARTESIAN_POINT ( 'NONE',  ( 0.006534887713546109859, 159.5822087645323393, -0.3270325034788579277 ) ) ;
#42157 = CIRCLE ( 'NONE', #8129, 0.6350000000000006750 ) ;
#42158 = CARTESIAN_POINT ( 'NONE',  ( -6.583861033951825950E-14, 91.02546620154572565, 1.480257718193877056E-29 ) ) ;
#42159 = CARTESIAN_POINT ( 'NONE',  ( -50.74392696651327839, 14.91217558840365953, 4.616263131616780591 ) ) ;
#42160 = CARTESIAN_POINT ( 'NONE',  ( -46.68114719912644262, 26.04180998113828238, 1.171086909392312636 ) ) ;
#42161 = CARTESIAN_POINT ( 'NONE',  ( 8.399484405886864735, 119.7521803362377568, -1.098797162006715844 ) ) ;
#42162 = NEXT_ASSEMBLY_USAGE_OCCURRENCE ( 'NAUO1', ' ', ' ', #26370, #37297, $ ) ;
#42163 = NEXT_ASSEMBLY_USAGE_OCCURRENCE ( 'NAUO2', ' ', ' ', #26370, #10216, $ ) ;
#42164 = NEXT_ASSEMBLY_USAGE_OCCURRENCE ( 'NAUO3', ' ', ' ', #26370, #20881, $ ) ;
#42165 = NEXT_ASSEMBLY_USAGE_OCCURRENCE ( 'NAUO4', ' ', ' ', #26370, #24009, $ ) ;
#42166 = NEXT_ASSEMBLY_USAGE_OCCURRENCE ( 'NAUO5', ' ', ' ', #26370, #31572, $ ) ;
#42167 = NEXT_ASSEMBLY_USAGE_OCCURRENCE ( 'NAUO6', ' ', ' ', #26370, #20881, $ ) ;
#42168 = NEXT_ASSEMBLY_USAGE_OCCURRENCE ( 'NAUO7', ' ', ' ', #26370, #10216, $ ) ;
ENDSEC;
END-ISO-10303-21;
